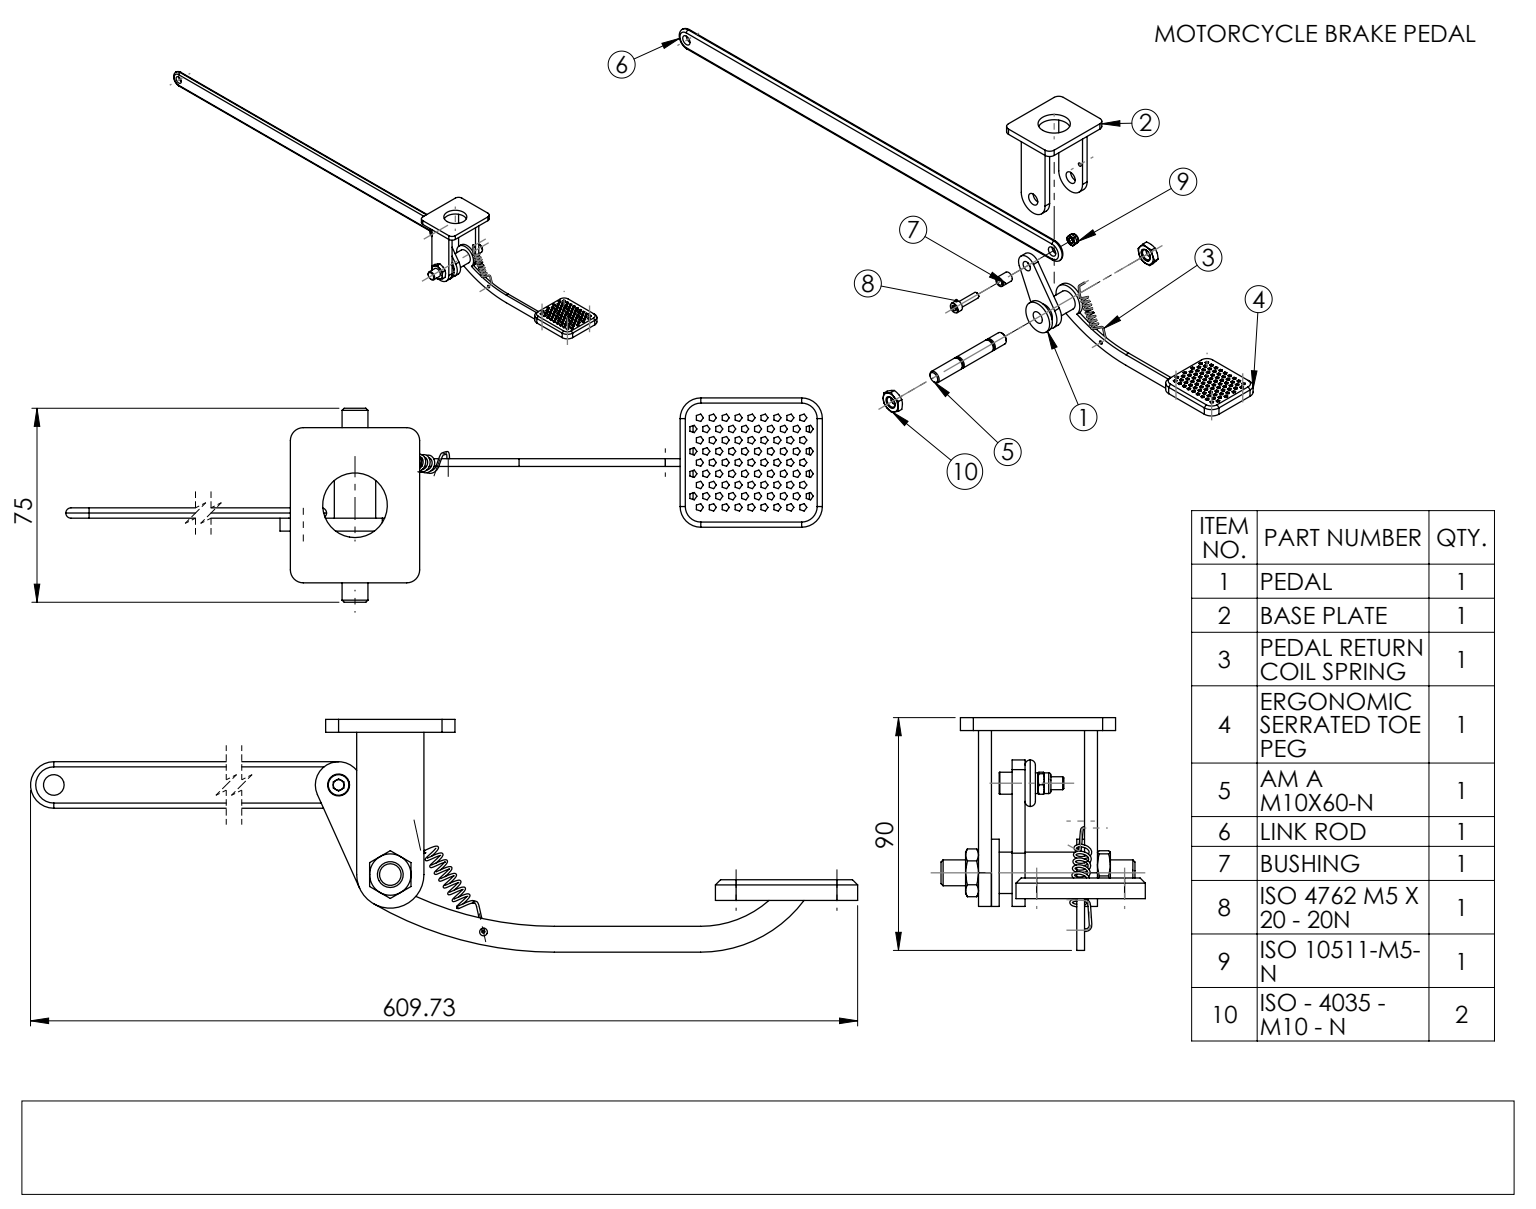
ISO-10303-21;
HEADER;
FILE_DESCRIPTION (('STEP AP214'),
    '1' );
FILE_NAME ('BR-593',
    '2026-09-30T16:28:02',
    ( '' ),
    ( '' ),
    'SwSTEP 2.0',
    'SolidWorks 2026',
    '' );
FILE_SCHEMA (( 'AUTOMOTIVE_DESIGN' ));
ENDSEC;

DATA;
#1 = CARTESIAN_POINT ( 'NONE',  ( 171.1922820468852819, -9.999999999999996447, -4.936203717676158398 ) ) ;
#2 = LINE ( 'NONE', #9287, #2166 ) ;
#3 = CARTESIAN_POINT ( 'NONE',  ( 10.46436961932593945, 16.48727764291732711, -17.33901581970886241 ) ) ;
#4 = PLANE ( 'NONE',  #18463 ) ;
#5 = CARTESIAN_POINT ( 'NONE',  ( 33.35202879388211983, -12.33251541790028760, -19.68467382345759376 ) ) ;
#6 = ORIENTED_EDGE ( 'NONE', *, *, #8201, .T. ) ;
#7 = CARTESIAN_POINT ( 'NONE',  ( 11.86544027865023843, 7.919735734555668039, -16.84125344233394372 ) ) ;
#8 = EDGE_LOOP ( 'NONE', ( #13410, #18933, #24855, #7147 ) ) ;
#9 = CARTESIAN_POINT ( 'NONE',  ( 158.6922820468853104, -1.999999999999974909, -0.6060766987539614181 ) ) ;
#10 = CARTESIAN_POINT ( 'NONE',  ( 20.51249478307574847, 1.942573248051725709, -13.31196225760961838 ) ) ;
#11 = CARTESIAN_POINT ( 'NONE',  ( 11.27738072919014911, 16.67146171448561276, -16.78403338633166442 ) ) ;
#12 = CARTESIAN_POINT ( 'NONE',  ( 35.03938282813840743, -19.89690018161999419, -20.20402626681843117 ) ) ;
#13 = AXIS2_PLACEMENT_3D ( 'NONE', #28994, #19329, #14737 ) ;
#14 = VERTEX_POINT ( 'NONE', #15281 ) ;
#15 = CARTESIAN_POINT ( 'NONE',  ( 9.776119957569173735, 17.05082265352876547, -16.72288386497739765 ) ) ;
#16 = CARTESIAN_POINT ( 'NONE',  ( 176.1922820468852535, -9.999999999999994671, -4.936203717676158398 ) ) ;
#17 = AXIS2_PLACEMENT_3D ( 'NONE', #6944, #25711, #22673 ) ;
#18 = CARTESIAN_POINT ( 'NONE',  ( 9.641351338355821810, 17.66888872024471624, -17.91303689663363130 ) ) ;
#19 = CARTESIAN_POINT ( 'NONE',  ( 129.5152310637605524, -10.00000000000000888, -21.71180489736090991 ) ) ;
#20 = LINE ( 'NONE', #28431, #3804 ) ;
#21 = ADVANCED_BREP_SHAPE_REPRESENTATION ( '', ( #979, #13190 ), #8326 ) ;
#22 = ORIENTED_EDGE ( 'NONE', *, *, #9858, .T. ) ;
#23 = DIRECTION ( 'NONE',  ( -0.5877852522924731371, 0.000000000000000000, 0.8090169943749474513 ) ) ;
#24 = EDGE_LOOP ( 'NONE', ( #18208, #203, #15820, #9762, #20509 ) ) ;
#25 = CARTESIAN_POINT ( 'NONE',  ( 10.43477690885096720, 16.62299358534909288, -17.37687480348504820 ) ) ;
#26 = EDGE_CURVE ( 'NONE', #4351, #19336, #2033, .T. ) ;
#27 = EDGE_CURVE ( 'NONE', #25495, #12783, #12701, .T. ) ;
#28 = CARTESIAN_POINT ( 'NONE',  ( 36.54859390953724585, -22.18451583373416014, -17.64281456791166036 ) ) ;
#29 = CARTESIAN_POINT ( 'NONE',  ( 24.62590367393082502, -9.567571807129121808, -15.85044010117769098 ) ) ;
#30 = ORIENTED_EDGE ( 'NONE', *, *, #5505, .F. ) ;
#31 = EDGE_CURVE ( 'NONE', #25811, #28060, #3559, .T. ) ;
#32 = FACE_OUTER_BOUND ( 'NONE', #14723, .T. ) ;
#33 = CARTESIAN_POINT ( 'NONE',  ( 142.0152310637605524, -1.999999999999978684, 1.702185954127501066 ) ) ;
#34 = VECTOR ( 'NONE', #18733, 1000.000000000000000 ) ;
#35 = CARTESIAN_POINT ( 'NONE',  ( 0.000000000000000000, 0.000000000000000000, 0.000000000000000000 ) ) ;
#36 = AXIS2_PLACEMENT_3D ( 'NONE', #24795, #28817, #15305 ) ;
#37 = CARTESIAN_POINT ( 'NONE',  ( 19.85258860919307367, 6.732389232436280402, -16.96582824858274208 ) ) ;
#38 = VECTOR ( 'NONE', #16062, 999.9999999999998863 ) ;
#39 = CARTESIAN_POINT ( 'NONE',  ( 29.40876261992080032, -8.787110225502646088, -16.42709622331022956 ) ) ;
#40 = ORIENTED_EDGE ( 'NONE', *, *, #8836, .F. ) ;
#41 = DIRECTION ( 'NONE',  ( -2.698458740408365879E-16, 1.000000000000000000, 0.000000000000000000 ) ) ;
#42 = STYLED_ITEM ( 'NONE', ( #6036 ), #28104 ) ;
#43 = EDGE_LOOP ( 'NONE', ( #10791, #17120, #27313, #27403, #18272 ) ) ;
#44 = CARTESIAN_POINT ( 'NONE',  ( 10.00000000000007816, 17.32050807568872486, -23.00000000000000711 ) ) ;
#45 = DIRECTION ( 'NONE',  ( 2.908569913943825554E-16, -1.000000000000000000, 0.000000000000000000 ) ) ;
#46 = ORIENTED_EDGE ( 'NONE', *, *, #12896, .F. ) ;
#47 = CARTESIAN_POINT ( 'NONE',  ( 149.7287565553229456, -10.00000000000000355, 0.8205080756887930260 ) ) ;
#48 = CARTESIAN_POINT ( 'NONE',  ( 10.33812866905494587, 18.38613571942487113, -17.90056368370468931 ) ) ;
#49 = LINE ( 'NONE', #2798, #15810 ) ;
#50 = EDGE_LOOP ( 'NONE', ( #6565, #21196, #16941, #11430, #26912 ) ) ;
#51 = CARTESIAN_POINT ( 'NONE',  ( 4.000000000000019540, 6.928203230275512325, 0.000000000000000000 ) ) ;
#52 = EDGE_LOOP ( 'NONE', ( #7879, #12886, #2199, #3337, #17093, #20123 ) ) ;
#53 = AXIS2_PLACEMENT_3D ( 'NONE', #5832, #6438, #24451 ) ;
#54 = CARTESIAN_POINT ( 'NONE',  ( 9.917712295358372288, 16.40146214360271770, -16.50402730409559027 ) ) ;
#55 = ORIENTED_EDGE ( 'NONE', *, *, #7367, .F. ) ;
#56 = CARTESIAN_POINT ( 'NONE',  ( 28.55476651072185845, -11.97999099613336504, -13.94805024529803994 ) ) ;
#57 = CARTESIAN_POINT ( 'NONE',  ( 142.2287565553230309, -10.00000000000000533, -29.49038105676660138 ) ) ;
#58 = CARTESIAN_POINT ( 'NONE',  ( 25.71553203045151292, -8.406338935355361031, -18.42709291467145150 ) ) ;
#59 = ORIENTED_EDGE ( 'NONE', *, *, #1895, .T. ) ;
#60 = LINE ( 'NONE', #7229, #30116 ) ;
#61 = CARTESIAN_POINT ( 'NONE',  ( 11.05541548581436118, 17.68942261459453036, -17.91440211708152574 ) ) ;
#62 = EDGE_CURVE ( 'NONE', #29710, #22500, #27244, .T. ) ;
#63 = CARTESIAN_POINT ( 'NONE',  ( 32.97927115036063839, -11.75136040154610662, -17.31233706439427067 ) ) ;
#64 = CARTESIAN_POINT ( 'NONE',  ( 14.34656430690936624, 9.113120221615268690, -15.03016663717492563 ) ) ;
#65 = ADVANCED_FACE ( 'NONE', ( #1579 ), #24770, .T. ) ;
#66 = CARTESIAN_POINT ( 'NONE',  ( 16.00000000000017053, 34.64101615137744972, 14.00000000000000178 ) ) ;
#67 = ADVANCED_FACE ( 'NONE', ( #10563 ), #23345, .T. ) ;
#68 = CARTESIAN_POINT ( 'NONE',  ( 23.37849240255853189, -5.075553540114302820, -18.86401745356084447 ) ) ;
#69 = EDGE_LOOP ( 'NONE', ( #19720, #1724, #9767, #14173 ) ) ;
#70 = PLANE ( 'NONE',  #26676 ) ;
#71 = ORIENTED_EDGE ( 'NONE', *, *, #5370, .F. ) ;
#72 =( NAMED_UNIT ( * ) PLANE_ANGLE_UNIT ( ) SI_UNIT ( $, .RADIAN. ) );
#73 = CARTESIAN_POINT ( 'NONE',  ( 16.00562779705659011, 2.776126820729137190, -17.20623408552720690 ) ) ;
#74 = CARTESIAN_POINT ( 'NONE',  ( 16.42253358145367415, 4.166353156564198024, -16.06924993952044289 ) ) ;
#75 = ORIENTED_EDGE ( 'NONE', *, *, #15408, .T. ) ;
#76 = VECTOR ( 'NONE', #4215, 1000.000000000000000 ) ;
#77 = CARTESIAN_POINT ( 'NONE',  ( 133.7287565553229456, -4.999999999999982236, 3.500000000000003109 ) ) ;
#78 = VECTOR ( 'NONE', #21293, 999.9999999999998863 ) ;
#79 = LINE ( 'NONE', #18686, #13812 ) ;
#80 = DIRECTION ( 'NONE',  ( 0.9510565162951536422, 0.000000000000000000, -0.3090169943749475623 ) ) ;
#81 = CARTESIAN_POINT ( 'NONE',  ( 164.5152310637605240, -9.999999999999996447, -28.60870317832789667 ) ) ;
#82 = DIRECTION ( 'NONE',  ( -1.110223024625156540E-16, 0.000000000000000000, -1.000000000000000000 ) ) ;
#83 = CARTESIAN_POINT ( 'NONE',  ( 9.641350810849047548, 17.66889113945805789, -17.91928203681695564 ) ) ;
#84 = CARTESIAN_POINT ( 'NONE',  ( 20.82548126942529976, -5.669333895406754031, -14.77195412306030420 ) ) ;
#85 = CARTESIAN_POINT ( 'NONE',  ( 23.74924978780510898, -3.048960050427876656, -13.27477993493952191 ) ) ;
#86 = EDGE_CURVE ( 'NONE', #12166, #722, #15592, .T. ) ;
#87 = CARTESIAN_POINT ( 'NONE',  ( 36.54859390953724585, -23.18451583373416014, -18.06010107863414405 ) ) ;
#88 = DIRECTION ( 'NONE',  ( 1.000000000000000000, 0.000000000000000000, 0.000000000000000000 ) ) ;
#89 = DIRECTION ( 'NONE',  ( -1.000000000000000000, 2.207829878515935943E-16, 0.000000000000000000 ) ) ;
#90 = PLANE ( 'NONE',  #29362 ) ;
#91 = DIRECTION ( 'NONE',  ( -2.698458740408365879E-16, 1.000000000000000000, 0.000000000000000000 ) ) ;
#92 = DIRECTION ( 'NONE',  ( -0.9510565162951536422, 0.000000000000000000, -0.3090169943749472292 ) ) ;
#93 = ORIENTED_EDGE ( 'NONE', *, *, #14811, .T. ) ;
#94 = CARTESIAN_POINT ( 'NONE',  ( -13.00000000000001243, 55.00000000000000711, 18.00000000000000000 ) ) ;
#95 = CARTESIAN_POINT ( 'NONE',  ( 10.33811987107833552, 18.38617606806709048, -17.90816805339326834 ) ) ;
#96 = ORIENTED_EDGE ( 'NONE', *, *, #21204, .F. ) ;
#97 = CARTESIAN_POINT ( 'NONE',  ( 164.5152310637604671, -9.999999999999998224, -11.28819510263909542 ) ) ;
#98 = CARTESIAN_POINT ( 'NONE',  ( 152.0152310637604671, -4.999999999999976907, -0.06116980274991495881 ) ) ;
#99 = ADVANCED_FACE ( 'NONE', ( #8123 ), #7974, .T. ) ;
#100 = CARTESIAN_POINT ( 'NONE',  ( 14.18486973814142793, 6.324582201221724098, -17.68508340245422872 ) ) ;
#101 = EDGE_CURVE ( 'NONE', #2266, #29239, #23530, .T. ) ;
#102 = VERTEX_POINT ( 'NONE', #17428 ) ;
#103 = EDGE_CURVE ( 'NONE', #184, #26603, #5846, .T. ) ;
#104 = CARTESIAN_POINT ( 'NONE',  ( 25.08912532741139501, -12.86307741315042108, -14.91192194027685147 ) ) ;
#105 = EDGE_LOOP ( 'NONE', ( #1685, #5636, #6833, #29745, #13110 ) ) ;
#106 = EDGE_CURVE ( 'NONE', #19956, #14105, #21866, .T. ) ;
#107 = CARTESIAN_POINT ( 'NONE',  ( 34.90271572771163733, -20.28292729397994876, -21.20502438346732887 ) ) ;
#108 = CARTESIAN_POINT ( 'NONE',  ( 24.18628427323349328, -0.8779346998738073449, -17.06787597161793357 ) ) ;
#109 = CARTESIAN_POINT ( 'NONE',  ( 18.93384218461971358, 6.651393094135895190, -15.21227712214292538 ) ) ;
#110 = ORIENTED_EDGE ( 'NONE', *, *, #8360, .T. ) ;
#111 = CARTESIAN_POINT ( 'NONE',  ( 28.58746438791548528, -7.443717211345676432, -18.79719194573140584 ) ) ;
#112 = AXIS2_PLACEMENT_3D ( 'NONE', #25183, #25333, #20434 ) ;
#113 = EDGE_LOOP ( 'NONE', ( #1842, #6412, #14178, #16562 ) ) ;
#114 = CARTESIAN_POINT ( 'NONE',  ( 141.1922820468854525, -10.00000000000000533, -30.91696583120935671 ) ) ;
#116 = ORIENTED_EDGE ( 'NONE', *, *, #15748, .F. ) ;
#115 = CARTESIAN_POINT ( 'NONE',  ( 171.1922820468853388, -4.999999999999971578, -19.40354224447947828 ) ) ;
#117 = VERTEX_POINT ( 'NONE', #8423 ) ;
#118 = CARTESIAN_POINT ( 'NONE',  ( 134.5152310637605524, -1.999999999999980460, -4.391296821672111328 ) ) ;
#119 = FACE_OUTER_BOUND ( 'NONE', #9403, .T. ) ;
#120 = CARTESIAN_POINT ( 'NONE',  ( 33.16581763841239194, -10.35476010881584052, -17.60936685258081624 ) ) ;
#121 = CARTESIAN_POINT ( 'NONE',  ( 9.641890818133653340, 17.66641459721583374, -17.82828029666912073 ) ) ;
#122 = ORIENTED_EDGE ( 'NONE', *, *, #28451, .T. ) ;
#123 = AXIS2_PLACEMENT_3D ( 'NONE', #1550, #9129, #25482 ) ;
#124 = DIRECTION ( 'NONE',  ( 0.9510565162951536422, 0.000000000000000000, -0.3090169943749475623 ) ) ;
#125 = CARTESIAN_POINT ( 'NONE',  ( 158.6922820468854241, -1.999999999999973133, -35.24709285013155835 ) ) ;
#126 = CARTESIAN_POINT ( 'NONE',  ( 10.46960557229346733, 16.46326489517938541, -17.33590790293451178 ) ) ;
#127 = CYLINDRICAL_SURFACE ( 'NONE', #6337, 13.00000000000000178 ) ;
#128 = CARTESIAN_POINT ( 'NONE',  ( 174.5152310637604955, -1.999999999999968914, -28.60870317832789667 ) ) ;
#129 = ORIENTED_EDGE ( 'NONE', *, *, #17959, .T. ) ;
#130 = DIRECTION ( 'NONE',  ( -0.5877852522924731371, -1.586114251531760728E-16, -0.8090169943749474513 ) ) ;
#131 = EDGE_CURVE ( 'NONE', #19668, #13066, #17725, .T. ) ;
#132 = LINE ( 'NONE', #2726, #539 ) ;
#134 = VERTEX_POINT ( 'NONE', #3860 ) ;
#133 = VECTOR ( 'NONE', #22097, 1000.000000000000000 ) ;
#135 = ADVANCED_FACE ( 'NONE', ( #10257 ), #20396, .T. ) ;
#136 = LINE ( 'NONE', #8159, #30161 ) ;
#137 = ORIENTED_EDGE ( 'NONE', *, *, #26787, .F. ) ;
#138 = EDGE_CURVE ( 'NONE', #19707, #18049, #20216, .T. ) ;
#139 = CARTESIAN_POINT ( 'NONE',  ( 11.09431937732777129, 9.685491096586417825, -17.29518830297554643 ) ) ;
#140 = CARTESIAN_POINT ( 'NONE',  ( 25.86320101420157158, -8.291784280105535032, -12.84902276017926859 ) ) ;
#141 = CARTESIAN_POINT ( 'NONE',  ( 19.89307947303188229, -2.966738011908462092, -16.73278295482091949 ) ) ;
#142 = ORIENTED_EDGE ( 'NONE', *, *, #977, .F. ) ;
#143 = CARTESIAN_POINT ( 'NONE',  ( 18.39996379557756256, 0.6904185378075045065, -15.43317298867526866 ) ) ;
#144 = FACE_OUTER_BOUND ( 'NONE', #11125, .T. ) ;
#145 = CARTESIAN_POINT ( 'NONE',  ( -2.644994884459112683, 7.710515798486374806, -0.08224679563972035756 ) ) ;
#146 = DIRECTION ( 'NONE',  ( 0.5877852522924731371, 1.586114251531760728E-16, 0.8090169943749474513 ) ) ;
#147 = CARTESIAN_POINT ( 'NONE',  ( 27.44219139316946965, -6.774709612358828181, -18.29578255718776703 ) ) ;
#148 = AXIS2_PLACEMENT_3D ( 'NONE', #18004, #8395, #8543 ) ;
#149 = CARTESIAN_POINT ( 'NONE',  ( 2.681483223904240987, -3.070647092368469000, -1.935399088488818784E-14 ) ) ;
#150 = DIRECTION ( 'NONE',  ( 0.000000000000000000, -0.000000000000000000, -1.000000000000000000 ) ) ;
#151 = PRESENTATION_STYLE_ASSIGNMENT (( #9284 ) ) ;
#152 = LINE ( 'NONE', #16311, #22917 ) ;
#153 = CARTESIAN_POINT ( 'NONE',  ( 2.681483223904239210, -3.070647092368469888, -2.449999999999981526 ) ) ;
#154 = VECTOR ( 'NONE', #27172, 1000.000000000000000 ) ;
#155 = EDGE_CURVE ( 'NONE', #6429, #19044, #27953, .T. ) ;
#156 = CARTESIAN_POINT ( 'NONE',  ( 10.35864918915110877, 16.97212501191939538, -17.92279151347709032 ) ) ;
#157 = CARTESIAN_POINT ( 'NONE',  ( 35.24964364652129234, -20.84149066036063047, -20.16262864730545346 ) ) ;
#158 = CARTESIAN_POINT ( 'NONE',  ( 31.39893620166130717, -10.86152586746012183, -14.84747879817187943 ) ) ;
#159 = EDGE_LOOP ( 'NONE', ( #26416, #20903, #28794, #24499, #27382, #1252 ) ) ;
#160 = CARTESIAN_POINT ( 'NONE',  ( 8.944584812045984989, 16.95159217075808655, -17.91472939532503261 ) ) ;
#161 = ORIENTED_EDGE ( 'NONE', *, *, #1761, .F. ) ;
#162 = LINE ( 'NONE', #17082, #29052 ) ;
#163 = CARTESIAN_POINT ( 'NONE',  ( 19.38992137333195842, 2.881095379261479739, -20.30776781288435373 ) ) ;
#164 = CARTESIAN_POINT ( 'NONE',  ( 11.27814055543051630, 16.66797705449195988, -16.78371917145281955 ) ) ;
#165 = CARTESIAN_POINT ( 'NONE',  ( 21.73040598723229877, -5.000000000000011546, -66.87931276303945083 ) ) ;
#166 = EDGE_LOOP ( 'NONE', ( #11300, #21186, #18431, #15934 ) ) ;
#167 = VECTOR ( 'NONE', #27934, 1000.000000000000000 ) ;
#168 = ORIENTED_EDGE ( 'NONE', *, *, #18099, .T. ) ;
#169 = CARTESIAN_POINT ( 'NONE',  ( 9.916551108984865692, 16.40678749232849398, -16.50450761325770443 ) ) ;
#170 = CARTESIAN_POINT ( 'NONE',  ( 125.7287565553229172, -4.000000000000003553, -33.50000000000000000 ) ) ;
#171 = CARTESIAN_POINT ( 'NONE',  ( 9.843778300897430000, 16.74053286659246709, -16.57516421589427225 ) ) ;
#172 = DIRECTION ( 'NONE',  ( -0.9510565162951536422, -2.566386769018988323E-16, 0.3090169943749475623 ) ) ;
#173 = CARTESIAN_POINT ( 'NONE',  ( 136.1922820468854241, -1.999999999999980460, -19.40354224447947473 ) ) ;
#174 = ORIENTED_EDGE ( 'NONE', *, *, #103, .T. ) ;
#175 = EDGE_CURVE ( 'NONE', #8969, #15955, #19420, .T. ) ;
#176 = CARTESIAN_POINT ( 'NONE',  ( 168.6922820468853104, -9.999999999999998224, -6.413161187712876909 ) ) ;
#177 = ORIENTED_EDGE ( 'NONE', *, *, #22974, .T. ) ;
#178 = EDGE_CURVE ( 'NONE', #21232, #6302, #23638, .T. ) ;
#179 = CARTESIAN_POINT ( 'NONE',  ( 10.35887147716723611, 16.97110557074245563, -17.87975733919941845 ) ) ;
#180 = ORIENTED_EDGE ( 'NONE', *, *, #14435, .F. ) ;
#181 = CARTESIAN_POINT ( 'NONE',  ( 36.04209255463945993, -19.90907354740926394, -20.43687144983462289 ) ) ;
#182 = CARTESIAN_POINT ( 'NONE',  ( 21.18945582756405344, -5.194394521544061227, -16.21196392551894405 ) ) ;
#183 = CARTESIAN_POINT ( 'NONE',  ( 27.21278356834291756, -7.014839303453253905, -18.45691071023835761 ) ) ;
#184 = VERTEX_POINT ( 'NONE', #293 ) ;
#185 = LINE ( 'NONE', #484, #11097 ) ;
#186 = CIRCLE ( 'NONE', #15750, 0.4999999999999998335 ) ;
#187 = DIRECTION ( 'NONE',  ( -0.5877852522924731371, -1.586114251531760728E-16, -0.8090169943749474513 ) ) ;
#188 = DIRECTION ( 'NONE',  ( 1.000000000000000000, 0.000000000000000000, 0.000000000000000000 ) ) ;
#189 = CARTESIAN_POINT ( 'NONE',  ( 19.09420370221858931, 5.586061004495046056, -18.95245686415860220 ) ) ;
#190 = CARTESIAN_POINT ( 'NONE',  ( 26.02011856185544048, -9.832954462109395166, -14.66174570188732140 ) ) ;
#191 = ORIENTED_EDGE ( 'NONE', *, *, #12444, .F. ) ;
#192 = FACE_BOUND ( 'NONE', #6466, .T. ) ;
#193 = ORIENTED_EDGE ( 'NONE', *, *, #2861, .F. ) ;
#194 = EDGE_CURVE ( 'NONE', #21176, #29420, #19051, .T. ) ;
#195 = ADVANCED_FACE ( 'NONE', ( #2293 ), #12020, .T. ) ;
#196 = FACE_OUTER_BOUND ( 'NONE', #7916, .T. ) ;
#197 = DIRECTION ( 'NONE',  ( -0.5877852522924731371, -1.586114251531760728E-16, -0.8090169943749474513 ) ) ;
#198 = LINE ( 'NONE', #11177, #23639 ) ;
#199 = VECTOR ( 'NONE', #16621, 1000.000000000000000 ) ;
#200 = CARTESIAN_POINT ( 'NONE',  ( 10.73095126193553028, 16.58460123524055874, -15.94999808000346242 ) ) ;
#201 = CARTESIAN_POINT ( 'NONE',  ( 11.95300070842526274, -5.000000000000014211, 36.78755350016455594 ) ) ;
#202 = CARTESIAN_POINT ( 'NONE',  ( 1.313474075707222521, 8.479269695850875976, -0.3167204509598505746 ) ) ;
#203 = ORIENTED_EDGE ( 'NONE', *, *, #27651, .T. ) ;
#204 = CARTESIAN_POINT ( 'NONE',  ( 9.916551108984865692, 16.40678749232849398, -16.50450761325770443 ) ) ;
#205 = ORIENTED_EDGE ( 'NONE', *, *, #21724, .F. ) ;
#206 = CARTESIAN_POINT ( 'NONE',  ( 18.72855672543857608, 2.184447897796080174, -13.82944682127929426 ) ) ;
#207 = DIRECTION ( 'NONE',  ( -0.9510565162951536422, -2.566386769018988323E-16, 0.3090169943749475623 ) ) ;
#208 = CARTESIAN_POINT ( 'NONE',  ( 161.1922820468853388, -9.999999999999998224, -13.59645775552055902 ) ) ;
#209 = VERTEX_POINT ( 'NONE', #7460 ) ;
#210 = CARTESIAN_POINT ( 'NONE',  ( 25.79824969357368047, -12.24460132778619226, -15.92960863319586906 ) ) ;
#211 = ORIENTED_EDGE ( 'NONE', *, *, #18755, .T. ) ;
#212 = FACE_OUTER_BOUND ( 'NONE', #25235, .T. ) ;
#213 = CARTESIAN_POINT ( 'NONE',  ( 11.05541700792677062, 17.68941563399299710, -17.91138715956864047 ) ) ;
#214 = ORIENTED_EDGE ( 'NONE', *, *, #14160, .F. ) ;
#215 = CARTESIAN_POINT ( 'NONE',  ( 33.76744293605320024, -13.18274801178271005, -18.77722780292321758 ) ) ;
#216 = CARTESIAN_POINT ( 'NONE',  ( 172.7287565553229456, -1.999999999999974021, -33.50000000000000000 ) ) ;
#217 = ORIENTED_EDGE ( 'NONE', *, *, #1804, .F. ) ;
#218 = CARTESIAN_POINT ( 'NONE',  ( 164.5152310637604671, -4.999999999999973355, -1.826485974285146553E-14 ) ) ;
#219 = CARTESIAN_POINT ( 'NONE',  ( 23.38597214775318278, -9.778565425610747042, -17.35394146810280347 ) ) ;
#220 = VERTEX_POINT ( 'NONE', #14001 ) ;
#221 = DIRECTION ( 'NONE',  ( 0.9510565162951536422, 0.000000000000000000, -0.3090169943749475623 ) ) ;
#222 = ORIENTED_EDGE ( 'NONE', *, *, #14772, .T. ) ;
#223 = CARTESIAN_POINT ( 'NONE',  ( 21.13650371987585075, 4.769999862021419901, -15.38713752973847448 ) ) ;
#224 = CARTESIAN_POINT ( 'NONE',  ( 17.80416238081608071, 8.561068417093343541, -18.87148919878627140 ) ) ;
#225 = VECTOR ( 'NONE', #26675, 1000.000000000000000 ) ;
#226 = ORIENTED_EDGE ( 'NONE', *, *, #24841, .F. ) ;
#227 = ORIENTED_EDGE ( 'NONE', *, *, #21857, .F. ) ;
#228 = CARTESIAN_POINT ( 'NONE',  ( 163.6922820468852819, -9.999999999999998224, -0.6060766987539614181 ) ) ;
#229 = CARTESIAN_POINT ( 'NONE',  ( 151.1922820468853672, -1.999999999999976685, -2.083034168790677043 ) ) ;
#230 = EDGE_CURVE ( 'NONE', #17843, #12321, #21337, .T. ) ;
#231 = EDGE_CURVE ( 'NONE', #23545, #23604, #24924, .T. ) ;
#232 = DIRECTION ( 'NONE',  ( -2.698458740408365879E-16, 1.000000000000000000, 0.000000000000000000 ) ) ;
#233 = DIRECTION ( 'NONE',  ( -2.698458740408365879E-16, 1.000000000000000000, 0.000000000000000000 ) ) ;
#234 = EDGE_CURVE ( 'NONE', #25907, #1746, #23486, .T. ) ;
#235 = DIRECTION ( 'NONE',  ( 0.3090169943749475623, 8.338696094058001131E-17, 0.9510565162951536422 ) ) ;
#236 = EDGE_LOOP ( 'NONE', ( #22910, #13879, #24086, #12025 ) ) ;
#237 = ADVANCED_FACE ( 'NONE', ( #2593 ), #18453, .T. ) ;
#238 = CARTESIAN_POINT ( 'NONE',  ( 9.921764701973689426, 16.38287729030320250, -16.50235149140834778 ) ) ;
#239 = CARTESIAN_POINT ( 'NONE',  ( 23.58034929565730309, -2.629172400889816075, -20.70693660786654888 ) ) ;
#240 = CARTESIAN_POINT ( 'NONE',  ( 19.50876870223950377, -1.661710298099399630, -15.95382585723518432 ) ) ;
#242 = ORIENTED_EDGE ( 'NONE', *, *, #15818, .F. ) ;
#241 = CARTESIAN_POINT ( 'NONE',  ( 32.24963562184495203, -10.43994945000269148, -19.19593526939238970 ) ) ;
#243 =( NAMED_UNIT ( * ) PLANE_ANGLE_UNIT ( ) SI_UNIT ( $, .RADIAN. ) );
#244 = DIRECTION ( 'NONE',  ( 0.3090169943749475623, 8.338696094058001131E-17, 0.9510565162951536422 ) ) ;
#245 = VECTOR ( 'NONE', #20484, 999.9999999999998863 ) ;
#246 = CARTESIAN_POINT ( 'NONE',  ( 157.0152310637605808, -4.999999999999975131, -32.93883019725009120 ) ) ;
#247 = DIRECTION ( 'NONE',  ( -0.9510565162951536422, -2.566386769018988816E-16, -0.3090169943749472292 ) ) ;
#248 = CARTESIAN_POINT ( 'NONE',  ( 14.39533340154967433, 6.572929804808670617, -18.54476805420031837 ) ) ;
#249 = ORIENTED_EDGE ( 'NONE', *, *, #10382, .F. ) ;
#250 = CARTESIAN_POINT ( 'NONE',  ( 169.5152310637604955, -1.999999999999970024, -30.37205893520531319 ) ) ;
#251 = CARTESIAN_POINT ( 'NONE',  ( 10.68867725192709273, 16.77847523382220984, -15.97313786900300059 ) ) ;
#252 = EDGE_LOOP ( 'NONE', ( #8891, #22753, #23266, #17300 ) ) ;
#253 = LINE ( 'NONE', #12283, #20751 ) ;
#254 = LINE ( 'NONE', #28368, #19057 ) ;
#255 = CARTESIAN_POINT ( 'NONE',  ( 19.20291185354690811, 8.143073066566493878, -16.32372945079811188 ) ) ;
#256 = CARTESIAN_POINT ( 'NONE',  ( 16.48605814428184857, 11.34583003460130435, -14.75612992736757256 ) ) ;
#257 = ORIENTED_EDGE ( 'NONE', *, *, #15684, .T. ) ;
#258 = CARTESIAN_POINT ( 'NONE',  ( 35.54859390953724585, -23.18451583373416014, -16.11276402859391510 ) ) ;
#259 = CARTESIAN_POINT ( 'NONE',  ( 20.30498772102510685, -2.023023832184298154, -16.94527736422809028 ) ) ;
#260 = CARTESIAN_POINT ( 'NONE',  ( 18.10666546173949953, 1.615696121519054618, -15.79491705146812563 ) ) ;
#261 = ORIENTED_EDGE ( 'NONE', *, *, #3073, .F. ) ;
#262 = CARTESIAN_POINT ( 'NONE',  ( 25.27233071153842303, -10.58027458246514207, -17.53878701932553952 ) ) ;
#263 = ORIENTED_EDGE ( 'NONE', *, *, #16267, .F. ) ;
#264 = AXIS2_PLACEMENT_3D ( 'NONE', #8989, #18309, #27664 ) ;
#265 = ORIENTED_EDGE ( 'NONE', *, *, #4022, .T. ) ;
#266 = DIRECTION ( 'NONE',  ( 0.9510565162951536422, 0.000000000000000000, -0.3090169943749475623 ) ) ;
#267 = PLANE ( 'NONE',  #1442 ) ;
#268 = ADVANCED_FACE ( 'NONE', ( #28096 ), #13304, .T. ) ;
#269 = PLANE ( 'NONE',  #1205 ) ;
#270 = EDGE_CURVE ( 'NONE', #13418, #14798, #2444, .T. ) ;
#271 = DIRECTION ( 'NONE',  ( -2.698458740408365879E-16, 1.000000000000000000, 0.000000000000000000 ) ) ;
#272 = CARTESIAN_POINT ( 'NONE',  ( 36.32827445255054499, -20.19473721995742821, -19.46526261299151983 ) ) ;
#273 = CARTESIAN_POINT ( 'NONE',  ( 15.87304960759194650, 9.003283391651189405, -12.44179493704351280 ) ) ;
#274 = ORIENTED_EDGE ( 'NONE', *, *, #12172, .T. ) ;
#275 = LINE ( 'NONE', #12157, #28348 ) ;
#276 = DIRECTION ( 'NONE',  ( 0.9510565162951536422, 0.000000000000000000, -0.3090169943749475623 ) ) ;
#277 = CARTESIAN_POINT ( 'NONE',  ( 10.55304143273637330, 16.08061740358965253, -17.30129946959702281 ) ) ;
#278 = DIRECTION ( 'NONE',  ( -2.698458740408365879E-16, 1.000000000000000000, 0.000000000000000000 ) ) ;
#279 = DIRECTION ( 'NONE',  ( -0.5877852522924731371, -1.586114251531760728E-16, -0.8090169943749474513 ) ) ;
#280 = VERTEX_POINT ( 'NONE', #21039 ) ;
#281 = VECTOR ( 'NONE', #14887, 1000.000000000000000 ) ;
#282 = DIRECTION ( 'NONE',  ( -0.8090169943749474513, -2.183098979609982436E-16, 0.5877852522924731371 ) ) ;
#283 = CONICAL_SURFACE ( 'NONE', #26615, 4.513000000000000789, 0.2131563744996339549 ) ;
#284 = LINE ( 'NONE', #14293, #25869 ) ;
#285 = ORIENTED_EDGE ( 'NONE', *, *, #11613, .T. ) ;
#286 = ORIENTED_EDGE ( 'NONE', *, *, #25521, .T. ) ;
#287 = DIRECTION ( 'NONE',  ( 0.9510565162951536422, 2.566386769018988816E-16, 0.3090169943749472292 ) ) ;
#288 = VERTEX_POINT ( 'NONE', #4857 ) ;
#289 = CARTESIAN_POINT ( 'NONE',  ( 9.667856465286563505, 16.22743184293591057, -17.88508098240584587 ) ) ;
#290 = CARTESIAN_POINT ( 'NONE',  ( 26.82298874931487020, -4.830090842487210878, -14.67398021261910301 ) ) ;
#291 = CARTESIAN_POINT ( 'NONE',  ( 23.41849298471255381, -3.203224238779429633, -13.27670244232306018 ) ) ;
#292 = DIRECTION ( 'NONE',  ( -0.5877852522924731371, -1.586114251531760235E-16, 0.8090169943749474513 ) ) ;
#293 = CARTESIAN_POINT ( 'NONE',  ( 5.000000000000004441, 0.000000000000000000, 4.250000000000000000 ) ) ;
#294 = CARTESIAN_POINT ( 'NONE',  ( 176.1922820468852535, -1.999999999999970024, -4.936203717676158398 ) ) ;
#295 = EDGE_CURVE ( 'NONE', #18615, #29151, #11869, .T. ) ;
#296 = CARTESIAN_POINT ( 'NONE',  ( 25.26806593431409453, -8.821542497490490575, -18.05414547114721557 ) ) ;
#297 = VECTOR ( 'NONE', #130, 1000.000000000000000 ) ;
#298 = ORIENTED_EDGE ( 'NONE', *, *, #1039, .F. ) ;
#299 = DIRECTION ( 'NONE',  ( -0.9510565162951536422, -2.566386769018988323E-16, 0.3090169943749475623 ) ) ;
#300 = LINE ( 'NONE', #23185, #15709 ) ;
#301 = VECTOR ( 'NONE', #6965, 1000.000000000000000 ) ;
#302 = ADVANCED_FACE ( 'NONE', ( #28256 ), #7306, .T. ) ;
#303 = EDGE_CURVE ( 'NONE', #13765, #18617, #4330, .T. ) ;
#304 = CARTESIAN_POINT ( 'NONE',  ( 0.000000000000000000, 0.000000000000000000, -0.5251556536572770106 ) ) ;
#306 = CARTESIAN_POINT ( 'NONE',  ( 169.7287565553228887, -9.999999999999998224, -7.839745962155603820 ) ) ;
#305 = AXIS2_PLACEMENT_3D ( 'NONE', #1101, #17395, #12671 ) ;
#307 = EDGE_CURVE ( 'NONE', #30043, #633, #23795, .T. ) ;
#308 = EDGE_CURVE ( 'NONE', #11681, #9083, #21945, .T. ) ;
#309 = CARTESIAN_POINT ( 'NONE',  ( 10.47103768343372288, 16.45669705093847313, -17.33522727542475295 ) ) ;
#310 = CARTESIAN_POINT ( 'NONE',  ( 20.00000000000017053, 34.64101615137744972, 14.00000000000000178 ) ) ;
#311 = LINE ( 'NONE', #12188, #27806 ) ;
#312 = ORIENTED_EDGE ( 'NONE', *, *, #15522, .T. ) ;
#313 = CARTESIAN_POINT ( 'NONE',  ( 13.40647825129878612, 7.637826363492710158, -15.68645975549014082 ) ) ;
#314 = VERTEX_POINT ( 'NONE', #24094 ) ;
#315 = DIRECTION ( 'NONE',  ( -0.5877852522924731371, -1.586114251531760728E-16, -0.8090169943749474513 ) ) ;
#316 = CARTESIAN_POINT ( 'NONE',  ( 23.66272512268759343, 2.894330346666426745, -16.12005855839824520 ) ) ;
#317 = CARTESIAN_POINT ( 'NONE',  ( 11.27662090294977837, 16.67494637447927275, -16.78434760121053060 ) ) ;
#318 = FACE_BOUND ( 'NONE', #13580, .T. ) ;
#319 = VERTEX_POINT ( 'NONE', #1201 ) ;
#320 = ORIENTED_EDGE ( 'NONE', *, *, #6013, .F. ) ;
#321 = CARTESIAN_POINT ( 'NONE',  ( 9.641350835837977584, 17.66889102485563612, -17.91507476468484938 ) ) ;
#322 = CARTESIAN_POINT ( 'NONE',  ( 174.7287565553229172, -9.999999999999994671, -25.16025403784440329 ) ) ;
#323 = VECTOR ( 'NONE', #10436, 1000.000000000000000 ) ;
#324 = CARTESIAN_POINT ( 'NONE',  ( 9.916953853453376766, 16.40494045485788632, -16.50434094533541085 ) ) ;
#325 = DIRECTION ( 'NONE',  ( -0.5877852522924731371, -1.586114251531760235E-16, 0.8090169943749474513 ) ) ;
#326 = PLANE ( 'NONE',  #24744 ) ;
#327 = ORIENTED_EDGE ( 'NONE', *, *, #10733, .F. ) ;
#328 = CARTESIAN_POINT ( 'NONE',  ( 4.680456609903983711, 6.535341423375600201, -4.983111142572226981 ) ) ;
#329 = ORIENTED_EDGE ( 'NONE', *, *, #5122, .F. ) ;
#330 = CARTESIAN_POINT ( 'NONE',  ( 10.47325967749744180, 16.44650670292386607, -17.33429203187744250 ) ) ;
#331 = ORIENTED_EDGE ( 'NONE', *, *, #10865, .F. ) ;
#333 = CARTESIAN_POINT ( 'NONE',  ( 32.72409873491027099, -9.637868425582460929, -18.36260606011342844 ) ) ;
#332 = VECTOR ( 'NONE', #22511, 1000.000000000000000 ) ;
#334 = CARTESIAN_POINT ( 'NONE',  ( 29.22485947447185595, -8.910266539455653501, -18.36689805200119707 ) ) ;
#335 = CARTESIAN_POINT ( 'NONE',  ( 25.23810427664335165, -6.496417100615061280, -13.69959235629456629 ) ) ;
#336 = VECTOR ( 'NONE', #15406, 1000.000000000000000 ) ;
#337 = DIRECTION ( 'NONE',  ( 0.000000000000000000, 0.000000000000000000, 1.000000000000000000 ) ) ;
#338 = CARTESIAN_POINT ( 'NONE',  ( 34.33515578781254618, -12.24072284059296933, -19.92088757525016973 ) ) ;
#339 = DIRECTION ( 'NONE',  ( 0.000000000000000000, 0.000000000000000000, 1.000000000000000000 ) ) ;
#340 = CARTESIAN_POINT ( 'NONE',  ( 15.71409287621466788, 5.292507472020409942, -15.15310296786427635 ) ) ;
#341 = CARTESIAN_POINT ( 'NONE',  ( 26.65048721414892086, -11.67344998524500355, -15.88597958324129777 ) ) ;
#342 = ORIENTED_EDGE ( 'NONE', *, *, #14480, .T. ) ;
#343 = FACE_BOUND ( 'NONE', #27021, .T. ) ;
#344 = VECTOR ( 'NONE', #10715, 1000.000000000000000 ) ;
#345 = ORIENTED_EDGE ( 'NONE', *, *, #10601, .T. ) ;
#346 = ADVANCED_FACE ( 'NONE', ( #19194 ), #5318, .T. ) ;
#347 = CARTESIAN_POINT ( 'NONE',  ( 0.000000000000000000, 0.000000000000000000, -25.03750572909317285 ) ) ;
#348 = PLANE ( 'NONE',  #22330 ) ;
#349 = LINE ( 'NONE', #4913, #4348 ) ;
#350 = VECTOR ( 'NONE', #1226, 1000.000000000000000 ) ;
#351 = PLANE ( 'NONE',  #28566 ) ;
#352 = AXIS2_PLACEMENT_3D ( 'NONE', #15421, #11403, #30099 ) ;
#353 = CARTESIAN_POINT ( 'NONE',  ( 10.71275814632708823, 16.66803718250374899, -15.95787532639072914 ) ) ;
#354 = CARTESIAN_POINT ( 'NONE',  ( 151.1922820468853672, -4.999999999999976907, -4.936203717676158398 ) ) ;
#355 = AXIS2_PLACEMENT_3D ( 'NONE', #20040, #29561, #1592 ) ;
#356 = FACE_OUTER_BOUND ( 'NONE', #20596, .T. ) ;
#357 = VERTEX_POINT ( 'NONE', #9882 ) ;
#358 = CARTESIAN_POINT ( 'NONE',  ( 9.914377700407460026, 16.41675502110963336, -16.50544604630902867 ) ) ;
#359 = CARTESIAN_POINT ( 'NONE',  ( 9.667469407758799704, 16.22920693809672343, -17.88529630510330293 ) ) ;
#360 = CARTESIAN_POINT ( 'NONE',  ( 17.70496941102466693, 2.403166580496164606, -19.15355645582771871 ) ) ;
#361 = DIRECTION ( 'NONE',  ( 0.000000000000000000, -1.000000000000000000, 0.000000000000000000 ) ) ;
#362 = CARTESIAN_POINT ( 'NONE',  ( 180.7287565553229456, -3.999999999999989786, 0.5000000000000029976 ) ) ;
#363 = CARTESIAN_POINT ( 'NONE',  ( 29.90031526554274777, -7.862644070287768905, -16.42500436498598049 ) ) ;
#364 = LINE ( 'NONE', #23553, #20283 ) ;
#365 = CARTESIAN_POINT ( 'NONE',  ( 11.27712745377669101, 16.67262326781682802, -16.78413812462462573 ) ) ;
#366 = ORIENTED_EDGE ( 'NONE', *, *, #25702, .F. ) ;
#367 = CARTESIAN_POINT ( 'NONE',  ( 35.54859390953724585, -21.18451583373416014, -16.94733705004010105 ) ) ;
#368 = LINE ( 'NONE', #18674, #9316 ) ;
#369 = CARTESIAN_POINT ( 'NONE',  ( 173.6922820468853104, -9.999999999999994671, -17.92658477444275889 ) ) ;
#370 = CARTESIAN_POINT ( 'NONE',  ( 9.112490548836888138, 16.18155505883174783, -17.05474119751274031 ) ) ;
#371 = CARTESIAN_POINT ( 'NONE',  ( 28.50845745928996067, -4.315366227951761502, -16.60164569054668604 ) ) ;
#372 = ORIENTED_EDGE ( 'NONE', *, *, #2420, .F. ) ;
#373 = DIRECTION ( 'NONE',  ( -1.000000000000000000, -0.000000000000000000, -0.000000000000000000 ) ) ;
#374 = EDGE_CURVE ( 'NONE', #25209, #19520, #2893, .T. ) ;
#375 = CARTESIAN_POINT ( 'NONE',  ( 18.32179412900206827, 3.681508181950223335, -14.15692665485406643 ) ) ;
#376 = CIRCLE ( 'NONE', #18872, 3.000000000000002665 ) ;
#377 = CARTESIAN_POINT ( 'NONE',  ( 16.45434084995319424, 8.990804261541395448, -14.78801614696073408 ) ) ;
#378 = ORIENTED_EDGE ( 'NONE', *, *, #6683, .T. ) ;
#379 = VERTEX_POINT ( 'NONE', #12319 ) ;
#380 = CARTESIAN_POINT ( 'NONE',  ( 144.5152310637605240, -4.999999999999978684, -4.391296821672111328 ) ) ;
#381 = CARTESIAN_POINT ( 'NONE',  ( 172.7287565553229456, -3.999999999999989786, -41.50000000000000711 ) ) ;
#382 = CARTESIAN_POINT ( 'NONE',  ( 1.214306433183764966E-14, 4.618802153517016507, -2.092734410091829034 ) ) ;
#383 = DIRECTION ( 'NONE',  ( 1.000000000000000000, 2.891205793294675861E-16, 0.000000000000000000 ) ) ;
#384 = CARTESIAN_POINT ( 'NONE',  ( 174.5152310637604103, -4.999999999999970690, -1.937508276747661576E-14 ) ) ;
#385 = AXIS2_PLACEMENT_3D ( 'NONE', #29992, #3996, #22923 ) ;
#386 = ORIENTED_EDGE ( 'NONE', *, *, #10034, .F. ) ;
#387 = CARTESIAN_POINT ( 'NONE',  ( 9.926830210242822972, 16.35964622367879784, -16.50025672554925293 ) ) ;
#388 = CARTESIAN_POINT ( 'NONE',  ( 29.32553208039167458, -8.962988822949116141, -16.84503999589972523 ) ) ;
#389 = CARTESIAN_POINT ( 'NONE',  ( 19.55718041265476970, -1.390565517676688900, -17.79492730709450754 ) ) ;
#391 = ORIENTED_EDGE ( 'NONE', *, *, #6783, .T. ) ;
#390 = CARTESIAN_POINT ( 'NONE',  ( 36.54859390953724585, -23.18451583373416014, -16.94733705004010105 ) ) ;
#392 = AXIS2_PLACEMENT_3D ( 'NONE', #4305, #4004, #27842 ) ;
#393 = LINE ( 'NONE', #19002, #17550 ) ;
#394 = CARTESIAN_POINT ( 'NONE',  ( 151.1922820468853956, -10.00000000000000178, -10.74328820663507678 ) ) ;
#395 = DIRECTION ( 'NONE',  ( 1.000000000000000000, 0.000000000000000000, -0.000000000000000000 ) ) ;
#396 = CARTESIAN_POINT ( 'NONE',  ( 14.03850921439652311, 8.975161913830900673, -15.18271992443145635 ) ) ;
#397 = EDGE_LOOP ( 'NONE', ( #19913, #23499 ) ) ;
#398 = CARTESIAN_POINT ( 'NONE',  ( 1.734723475976807094E-15, 2.928571428571426161, 2.549999999999999378 ) ) ;
#399 = CARTESIAN_POINT ( 'NONE',  ( 10.35722669462089840, 18.29854973974792998, -17.31575102165233915 ) ) ;
#400 = CARTESIAN_POINT ( 'NONE',  ( -20.00000000000017053, 34.64101615137744972, 0.000000000000000000 ) ) ;
#401 = CARTESIAN_POINT ( 'NONE',  ( 0.000000000000000000, 0.000000000000000000, -5.000000000000000888 ) ) ;
#402 = EDGE_LOOP ( 'NONE', ( #24156, #22408, #9241, #18567 ) ) ;
#403 = CARTESIAN_POINT ( 'NONE',  ( 15.14574614762244487, 6.587483969391940697, -15.14885142785537830 ) ) ;
#404 = EDGE_LOOP ( 'NONE', ( #3779, #2242, #2825, #27348 ) ) ;
#405 = CARTESIAN_POINT ( 'NONE',  ( 12.96291568738609890, 5.695260009123724210, -16.43886026595064109 ) ) ;
#406 = ORIENTED_EDGE ( 'NONE', *, *, #21308, .T. ) ;
#407 = CARTESIAN_POINT ( 'NONE',  ( 32.30218501430429967, -10.99871056796995816, -17.40035725849610060 ) ) ;
#408 = ADVANCED_FACE ( 'NONE', ( #24392 ), #12626, .T. ) ;
#409 = EDGE_CURVE ( 'NONE', #5044, #29035, #5775, .T. ) ;
#410 = CARTESIAN_POINT ( 'NONE',  ( 23.12480016457037379, 1.528454477237789488, -15.53356264363713102 ) ) ;
#411 = EDGE_CURVE ( 'NONE', #18619, #29440, #26701, .T. ) ;
#412 = CARTESIAN_POINT ( 'NONE',  ( 19.55510877418759819, -0.09764134006120470111, -19.21341144728512518 ) ) ;
#413 = VECTOR ( 'NONE', #9450, 1000.000000000000000 ) ;
#414 = CARTESIAN_POINT ( 'NONE',  ( 27.32534031592636836, -8.675155620653059785, -19.25315075663615971 ) ) ;
#415 = VECTOR ( 'NONE', #2292, 1000.000000000000000 ) ;
#416 = ORIENTED_EDGE ( 'NONE', *, *, #15789, .T. ) ;
#417 = DIRECTION ( 'NONE',  ( 0.3090169943749475623, 8.338696094058001131E-17, 0.9510565162951536422 ) ) ;
#419 = EDGE_LOOP ( 'NONE', ( #26721, #25285, #4227, #20986 ) ) ;
#418 = DIRECTION ( 'NONE',  ( -2.698458740408365879E-16, 1.000000000000000000, 0.000000000000000000 ) ) ;
#420 = DIRECTION ( 'NONE',  ( 0.3090169943749475623, 8.338696094058001131E-17, 0.9510565162951536422 ) ) ;
#421 = LINE ( 'NONE', #18729, #12178 ) ;
#422 = CARTESIAN_POINT ( 'NONE',  ( 35.57309713841538468, -16.80212557611773505, -19.25277297559858525 ) ) ;
#423 = CARTESIAN_POINT ( 'NONE',  ( 9.641566850259106758, 17.66790035518494051, -17.86107206016944460 ) ) ;
#424 = ORIENTED_EDGE ( 'NONE', *, *, #5508, .F. ) ;
#425 = CARTESIAN_POINT ( 'NONE',  ( 18.07240892486890615, -5.000000000000012434, -55.62115542516819744 ) ) ;
#426 = CARTESIAN_POINT ( 'NONE',  ( 131.1922820468854241, -1.999999999999981792, -28.06379628232387446 ) ) ;
#427 = CARTESIAN_POINT ( 'NONE',  ( 12.02823749386838514, 9.315180647891255106, -16.69125397286443047 ) ) ;
#428 = DIRECTION ( 'NONE',  ( -0.000000000000000000, -0.000000000000000000, -1.000000000000000000 ) ) ;
#429 = LINE ( 'NONE', #19037, #21295 ) ;
#430 = ORIENTED_EDGE ( 'NONE', *, *, #4985, .T. ) ;
#431 = VECTOR ( 'NONE', #12408, 1000.000000000000000 ) ;
#432 = CARTESIAN_POINT ( 'NONE',  ( 159.5152310637604955, -4.999999999999974243, -11.28819510263909542 ) ) ;
#433 = CARTESIAN_POINT ( 'NONE',  ( -13.00000000000001243, 55.00000000000000711, -23.00000000000000000 ) ) ;
#434 = ORIENTED_EDGE ( 'NONE', *, *, #645, .T. ) ;
#435 = CARTESIAN_POINT ( 'NONE',  ( 134.5152310637605524, -1.999999999999980460, -13.05155085951650840 ) ) ;
#436 = VERTEX_POINT ( 'NONE', #19791 ) ;
#437 = CARTESIAN_POINT ( 'NONE',  ( 9.667845848563926481, 16.22748053257927126, -17.88508528815513543 ) ) ;
#438 = VERTEX_POINT ( 'NONE', #10483 ) ;
#439 = EDGE_CURVE ( 'NONE', #26227, #4517, #895, .T. ) ;
#440 = AXIS2_PLACEMENT_3D ( 'NONE', #10772, #20082, #29458 ) ;
#441 = CARTESIAN_POINT ( 'NONE',  ( 25.04433344647707571, -4.420048373160954114, -18.22226412361657921 ) ) ;
#442 = EDGE_CURVE ( 'NONE', #18552, #1065, #26238, .T. ) ;
#443 = CARTESIAN_POINT ( 'NONE',  ( 21.55249387529322647, -4.041031698679099726, -14.19001464829599435 ) ) ;
#444 = LINE ( 'NONE', #2443, #25266 ) ;
#445 = CARTESIAN_POINT ( 'NONE',  ( -1.310872448937995705, 8.480771745766411129, -0.3173508448886640521 ) ) ;
#446 = EDGE_CURVE ( 'NONE', #20723, #20491, #23957, .T. ) ;
#447 = DIRECTION ( 'NONE',  ( -0.7172983783020613346, 0.6967661275386690667, -3.330669073875468142E-16 ) ) ;
#448 = CARTESIAN_POINT ( 'NONE',  ( 26.72181814967143509, -3.137724904577397389, -15.69709663067708050 ) ) ;
#449 = ORIENTED_EDGE ( 'NONE', *, *, #11568, .T. ) ;
#450 = DIRECTION ( 'NONE',  ( -1.110223024625156540E-16, 0.000000000000000000, -1.000000000000000000 ) ) ;
#451 = FACE_OUTER_BOUND ( 'NONE', #23218, .T. ) ;
#452 = VECTOR ( 'NONE', #19393, 1000.000000000000000 ) ;
#453 = DIRECTION ( 'NONE',  ( 0.3090169943749472292, 8.338696094057992503E-17, -0.9510565162951536422 ) ) ;
#454 = CARTESIAN_POINT ( 'NONE',  ( 63.44486372867152824, 109.8897274573438096, -186.4312945166758482 ) ) ;
#455 = LINE ( 'NONE', #21049, #14790 ) ;
#456 = CARTESIAN_POINT ( 'NONE',  ( 12.02305193244137449, 9.338961869187645704, -16.69339841729684437 ) ) ;
#457 = DIRECTION ( 'NONE',  ( 1.000000000000000000, 2.698458740408365879E-16, -1.110223024625156540E-16 ) ) ;
#458 = CARTESIAN_POINT ( 'NONE',  ( 34.96805304670973413, -19.57645325810014114, -20.18246498508359466 ) ) ;
#459 = ORIENTED_EDGE ( 'NONE', *, *, #24414, .T. ) ;
#460 = CARTESIAN_POINT ( 'NONE',  ( 13.81482270056995532, 7.818281081198240834, -15.36100202165747675 ) ) ;
#461 = VERTEX_POINT ( 'NONE', #21635 ) ;
#462 = DIRECTION ( 'NONE',  ( -1.000000000000000000, -4.440892098500623203E-16, 0.000000000000000000 ) ) ;
#463 = CARTESIAN_POINT ( 'NONE',  ( 21.66440995182641416, 5.535554982823286174, -17.57621636221614025 ) ) ;
#464 = CARTESIAN_POINT ( 'NONE',  ( 12.84801357566967717, 9.517348710814296453, -16.13078356789775469 ) ) ;
#465 = CARTESIAN_POINT ( 'NONE',  ( 130.7287565553229456, -4.999999999999983125, 3.500000000000003109 ) ) ;
#466 = ORIENTED_EDGE ( 'NONE', *, *, #9296, .T. ) ;
#467 = EDGE_CURVE ( 'NONE', #22249, #23534, #732, .T. ) ;
#468 = ORIENTED_EDGE ( 'NONE', *, *, #9842, .F. ) ;
#469 = CARTESIAN_POINT ( 'NONE',  ( 11.40798482813988635, 9.566882342703072695, -15.88774718835883348 ) ) ;
#470 = FACE_OUTER_BOUND ( 'NONE', #17896, .T. ) ;
#471 = CARTESIAN_POINT ( 'NONE',  ( 10.24089172292967298, 14.91932009296530559, -16.37038124228770997 ) ) ;
#472 = FACE_OUTER_BOUND ( 'NONE', #16901, .T. ) ;
#473 = ORIENTED_EDGE ( 'NONE', *, *, #13528, .T. ) ;
#474 = CARTESIAN_POINT ( 'NONE',  ( -4.000000000000010658, -2.309401076758525573, -0.3572655899081716435 ) ) ;
#475 = VERTEX_POINT ( 'NONE', #12779 ) ;
#476 = CARTESIAN_POINT ( 'NONE',  ( 10.40163623209820365, 16.77498095339038287, -17.46874319472340176 ) ) ;
#477 = ORIENTED_EDGE ( 'NONE', *, *, #15791, .T. ) ;
#478 = VECTOR ( 'NONE', #30246, 1000.000000000000000 ) ;
#479 = CARTESIAN_POINT ( 'NONE',  ( 32.45862320860160821, -9.597537451891041016, -17.61229109800368064 ) ) ;
#480 = CARTESIAN_POINT ( 'NONE',  ( 29.62588713853392264, -10.65184931322849060, -12.76488833982454629 ) ) ;
#481 = CARTESIAN_POINT ( 'NONE',  ( 29.46565128511723586, -7.689737916804423534, -14.82739468409561567 ) ) ;
#482 = ORIENTED_EDGE ( 'NONE', *, *, #14397, .T. ) ;
#483 = EDGE_CURVE ( 'NONE', #29391, #7152, #10029, .T. ) ;
#484 = CARTESIAN_POINT ( 'NONE',  ( 12.50940683846913970, -5.000000000000014211, 38.49999548658399107 ) ) ;
#485 = EDGE_CURVE ( 'NONE', #18308, #9388, #28550, .T. ) ;
#486 = VERTEX_POINT ( 'NONE', #7602 ) ;
#487 = EDGE_CURVE ( 'NONE', #4418, #10786, #7903, .T. ) ;
#488 = CIRCLE ( 'NONE', #12639, 4.000000000000000000 ) ;
#489 = EDGE_CURVE ( 'NONE', #20712, #9080, #7254, .T. ) ;
#490 = DIRECTION ( 'NONE',  ( -2.698458740408365879E-16, 1.000000000000000000, 0.000000000000000000 ) ) ;
#491 = SHAPE_DEFINITION_REPRESENTATION ( #26931, #5250 ) ;
#492 = CARTESIAN_POINT ( 'NONE',  ( 28.92040988821396752, -12.03996551347764132, -12.87516188627701474 ) ) ;
#493 = CARTESIAN_POINT ( 'NONE',  ( 26.45169718342334164, -9.008644514675534509, -18.11399877363951205 ) ) ;
#494 = ORIENTED_EDGE ( 'NONE', *, *, #2114, .T. ) ;
#495 = FACE_BOUND ( 'NONE', #28944, .T. ) ;
#496 =( GEOMETRIC_REPRESENTATION_CONTEXT ( 3 ) GLOBAL_UNCERTAINTY_ASSIGNED_CONTEXT ( ( #4915 ) ) GLOBAL_UNIT_ASSIGNED_CONTEXT ( ( #25066, #15887, #27085 ) ) REPRESENTATION_CONTEXT ( 'NONE', 'WORKASPACE' ) );
#497 = CARTESIAN_POINT ( 'NONE',  ( -2.500000000000002665, -1.110223024625156738E-15, -2.424599999999998978 ) ) ;
#498 = FACE_OUTER_BOUND ( 'NONE', #5684, .T. ) ;
#499 = VECTOR ( 'NONE', #27812, 1000.000000000000000 ) ;
#500 = DIRECTION ( 'NONE',  ( 0.9510565162951536422, 2.566386769018988816E-16, 0.3090169943749472292 ) ) ;
#501 = DIRECTION ( 'NONE',  ( -1.000000000000000000, -4.440892098500622217E-16, 0.000000000000000000 ) ) ;
#502 = CIRCLE ( 'NONE', #23914, 4.000000000000003553 ) ;
#503 = CARTESIAN_POINT ( 'NONE',  ( 10.33813570737955700, 18.38610344077106973, -17.89676158639688452 ) ) ;
#504 = DIRECTION ( 'NONE',  ( -2.698458740408365879E-16, 1.000000000000000000, 0.000000000000000000 ) ) ;
#505 = CARTESIAN_POINT ( 'NONE',  ( 162.0152310637605240, -9.999999999999998224, -34.70218595412750773 ) ) ;
#506 = VERTEX_POINT ( 'NONE', #26086 ) ;
#507 = CARTESIAN_POINT ( 'NONE',  ( 9.917965570771830386, 16.40030059027150600, -16.50392256580263606 ) ) ;
#508 = CARTESIAN_POINT ( 'NONE',  ( 20.43163981785493988, 0.2187255735321424754, -20.49791845872360341 ) ) ;
#509 = LINE ( 'NONE', #21850, #18033 ) ;
#510 = LINE ( 'NONE', #23703, #12518 ) ;
#511 = CARTESIAN_POINT ( 'NONE',  ( 137.0152310637605808, -1.999999999999980016, 1.702185954127501066 ) ) ;
#512 = ORIENTED_EDGE ( 'NONE', *, *, #5043, .F. ) ;
#513 = LINE ( 'NONE', #12092, #15899 ) ;
#514 = CARTESIAN_POINT ( 'NONE',  ( 11.27864710625743427, 16.66565394782951515, -16.78350969486689692 ) ) ;
#515 = AXIS2_PLACEMENT_3D ( 'NONE', #15266, #13594, #10844 ) ;
#516 = EDGE_LOOP ( 'NONE', ( #242, #27504, #8040, #18443, #3018 ) ) ;
#518 = VECTOR ( 'NONE', #4177, 1000.000000000000000 ) ;
#517 = CARTESIAN_POINT ( 'NONE',  ( 35.24753590068310416, -19.83202167481471889, -19.22462439892593977 ) ) ;
#519 = CARTESIAN_POINT ( 'NONE',  ( 17.72480397827495224, 1.356124466512965476, -19.40231245121514903 ) ) ;
#520 = EDGE_CURVE ( 'NONE', #12932, #5386, #5166, .T. ) ;
#521 = CARTESIAN_POINT ( 'NONE',  ( 130.7287565553229456, -4.999999999999983125, 3.500000000000003109 ) ) ;
#522 = CARTESIAN_POINT ( 'NONE',  ( 9.112135424753279977, 16.18318370314694832, -17.05489040841110437 ) ) ;
#523 = CARTESIAN_POINT ( 'NONE',  ( 24.27832910178602788, -5.559203070376852018, -13.12236226054620047 ) ) ;
#524 = ADVANCED_FACE ( 'NONE', ( #22562 ), #3633, .T. ) ;
#525 = ORIENTED_EDGE ( 'NONE', *, *, #27075, .F. ) ;
#526 = ADVANCED_FACE ( 'NONE', ( #15359 ), #12926, .T. ) ;
#527 = LINE ( 'NONE', #9813, #17849 ) ;
#528 =( NAMED_UNIT ( * ) SI_UNIT ( $, .STERADIAN. ) SOLID_ANGLE_UNIT ( ) );
#529 = MECHANICAL_DESIGN_GEOMETRIC_PRESENTATION_REPRESENTATION (  '', ( #42 ), #25882 ) ;
#530 = CARTESIAN_POINT ( 'NONE',  ( 21.58357356133149807, 4.347441036859617469, -17.91576365920758107 ) ) ;
#531 = CARTESIAN_POINT ( 'NONE',  ( 18.42634509371275797, 7.189141296957872740, -15.94500943014882210 ) ) ;
#532 = VECTOR ( 'NONE', #22824, 1000.000000000000000 ) ;
#533 = ORIENTED_EDGE ( 'NONE', *, *, #15684, .F. ) ;
#534 = LINE ( 'NONE', #822, #24024 ) ;
#535 = EDGE_LOOP ( 'NONE', ( #7211, #6231, #28486, #4893 ) ) ;
#536 = ORIENTED_EDGE ( 'NONE', *, *, #4318, .F. ) ;
#537 = CARTESIAN_POINT ( 'NONE',  ( 146.1922820468854525, -10.00000000000000178, -22.25671179336496053 ) ) ;
#538 = CARTESIAN_POINT ( 'NONE',  ( 139.5152310637605808, -10.00000000000000533, -21.71180489736090991 ) ) ;
#539 = VECTOR ( 'NONE', #19186, 999.9999999999998863 ) ;
#540 = CARTESIAN_POINT ( 'NONE',  ( 1.310872448937984602, -8.480771745766441327, -0.3173508448886784294 ) ) ;
#541 = DIRECTION ( 'NONE',  ( 0.000000000000000000, 0.000000000000000000, -1.000000000000000000 ) ) ;
#542 = VECTOR ( 'NONE', #24235, 1000.000000000000000 ) ;
#543 = CARTESIAN_POINT ( 'NONE',  ( 12.10607290817362092, -5.000000000000014211, -37.25866128932931787 ) ) ;
#544 = ORIENTED_EDGE ( 'NONE', *, *, #13525, .F. ) ;
#545 = CARTESIAN_POINT ( 'NONE',  ( 9.916411867603999397, 16.40742607105030260, -16.50456570466356965 ) ) ;
#546 = CARTESIAN_POINT ( 'NONE',  ( 28.54819463643023880, -8.737303380947411213, -14.37855314081258307 ) ) ;
#547 = CARTESIAN_POINT ( 'NONE',  ( 20.97044927184332508, -4.289323992320570156, -15.06659861376252429 ) ) ;
#548 = EDGE_CURVE ( 'NONE', #20384, #24083, #19953, .T. ) ;
#550 = ORIENTED_EDGE ( 'NONE', *, *, #23991, .F. ) ;
#549 = CARTESIAN_POINT ( 'NONE',  ( 32.45272648307624053, -11.02157468472264412, -17.82583700188536824 ) ) ;
#551 = FACE_OUTER_BOUND ( 'NONE', #15661, .T. ) ;
#552 = DIRECTION ( 'NONE',  ( 0.9510565162951536422, 0.000000000000000000, -0.3090169943749475623 ) ) ;
#553 = DIRECTION ( 'NONE',  ( -0.000000000000000000, -1.000000000000000000, -0.000000000000000000 ) ) ;
#554 = CARTESIAN_POINT ( 'NONE',  ( 148.6922820468854525, -4.999999999999976907, -23.73366926340167637 ) ) ;
#555 = CARTESIAN_POINT ( 'NONE',  ( 16.09764958744793262, 8.143416238145906760, -19.84970969296679044 ) ) ;
#556 = EDGE_LOOP ( 'NONE', ( #3105, #12356, #15207, #22632, #19486 ) ) ;
#557 = FACE_OUTER_BOUND ( 'NONE', #419, .T. ) ;
#558 = CARTESIAN_POINT ( 'NONE',  ( 10.33819201225523621, 18.38584521943398187, -17.87775236254758227 ) ) ;
#559 = LINE ( 'NONE', #9844, #18339 ) ;
#560 = DIRECTION ( 'NONE',  ( 2.698458740408365879E-16, -1.000000000000000000, 0.000000000000000000 ) ) ;
#561 = CARTESIAN_POINT ( 'NONE',  ( 17.32695330507268494, 5.471673316493076200, -20.08600194542987794 ) ) ;
#562 = CARTESIAN_POINT ( 'NONE',  ( 16.38450301900381945, 9.168174629645104545, -21.04437084800770918 ) ) ;
#563 = VERTEX_POINT ( 'NONE', #10643 ) ;
#565 = AXIS2_PLACEMENT_3D ( 'NONE', #8777, #15341, #10624 ) ;
#564 = CARTESIAN_POINT ( 'NONE',  ( 32.45272648307624053, -11.02157468472264412, -17.82583700188536824 ) ) ;
#566 = CARTESIAN_POINT ( 'NONE',  ( 23.60892706051935619, -2.861763136178346212, -14.25286661070829908 ) ) ;
#567 = AXIS2_PLACEMENT_3D ( 'NONE', #11521, #19011, #13959 ) ;
#568 = CARTESIAN_POINT ( 'NONE',  ( 22.48601049859325585, 2.925819830077934558, -17.76611561182923893 ) ) ;
#569 = CARTESIAN_POINT ( 'NONE',  ( 28.63790973356518776, -5.888324979419876648, -13.82040474618100312 ) ) ;
#570 = VERTEX_POINT ( 'NONE', #8354 ) ;
#571 = CARTESIAN_POINT ( 'NONE',  ( 129.5152310637605808, -10.00000000000000888, -11.28819510263909187 ) ) ;
#573 = ORIENTED_EDGE ( 'NONE', *, *, #19437, .T. ) ;
#572 = DIRECTION ( 'NONE',  ( -0.9510565162951536422, 0.000000000000000000, -0.3090169943749472292 ) ) ;
#574 = DIRECTION ( 'NONE',  ( -0.8090169943749474513, -2.183098979609982436E-16, -0.5877852522924731371 ) ) ;
#575 = DIRECTION ( 'NONE',  ( 0.9510565162951536422, 0.000000000000000000, -0.3090169943749475623 ) ) ;
#576 = ADVANCED_FACE ( 'NONE', ( #3939 ), #15213, .T. ) ;
#577 = CARTESIAN_POINT ( 'NONE',  ( 32.71419323209526908, -10.28616775856061416, -16.33292762241428520 ) ) ;
#578 = AXIS2_PLACEMENT_3D ( 'NONE', #20455, #15424, #27383 ) ;
#579 = CARTESIAN_POINT ( 'NONE',  ( 9.641354186875979337, 17.66887565656821124, -17.90893343548146177 ) ) ;
#580 = PRODUCT_DEFINITION ( 'UNKNOWN', '', #1483, #2194 ) ;
#581 = DIRECTION ( 'NONE',  ( 0.3090169943749472292, 8.338696094057992503E-17, -0.9510565162951536422 ) ) ;
#582 = CARTESIAN_POINT ( 'NONE',  ( 106.2677862141057545, -4.999999999999988454, -77.20806604152963359 ) ) ;
#583 = CARTESIAN_POINT ( 'NONE',  ( 13.10707286029108865, 8.563798077496334926, -15.92507172258792281 ) ) ;
#584 = CARTESIAN_POINT ( 'NONE',  ( 138.6922820468854525, -4.999999999999980460, -23.73366926340167282 ) ) ;
#585 = CARTESIAN_POINT ( 'NONE',  ( 153.6922820468854241, -1.999999999999974465, -23.73366926340167637 ) ) ;
#586 = ORIENTED_EDGE ( 'NONE', *, *, #25073, .T. ) ;
#587 = DIRECTION ( 'NONE',  ( -0.5877852522924731371, 0.000000000000000000, 0.8090169943749474513 ) ) ;
#588 = CARTESIAN_POINT ( 'NONE',  ( 142.0152310637605808, -1.999999999999978018, -26.04193191628310800 ) ) ;
#589 = ORIENTED_EDGE ( 'NONE', *, *, #23254, .T. ) ;
#590 = VERTEX_POINT ( 'NONE', #3789 ) ;
#591 = EDGE_LOOP ( 'NONE', ( #6929, #8428, #23827, #25905 ) ) ;
#592 = ORIENTED_EDGE ( 'NONE', *, *, #18201, .T. ) ;
#593 = CARTESIAN_POINT ( 'NONE',  ( 11.22273001195053155, 9.096583557657577757, -17.24208598844832352 ) ) ;
#594 = CARTESIAN_POINT ( 'NONE',  ( 27.63487812444411418, -5.020849242181972372, -17.14317672846274831 ) ) ;
#595 = CARTESIAN_POINT ( 'NONE',  ( 26.02348467347448491, -3.622150272347476108, -19.21400332953221124 ) ) ;
#596 = CARTESIAN_POINT ( 'NONE',  ( 143.6922820468854525, -10.00000000000000355, -17.92658477444275889 ) ) ;
#597 = DIRECTION ( 'NONE',  ( -2.207829878515935943E-16, 1.000000000000000000, 0.000000000000000000 ) ) ;
#598 = VECTOR ( 'NONE', #146, 1000.000000000000000 ) ;
#599 = CARTESIAN_POINT ( 'NONE',  ( 15.12871522451188788, -5.000000000000013323, -46.56139778509288618 ) ) ;
#600 = VERTEX_POINT ( 'NONE', #24546 ) ;
#601 = CARTESIAN_POINT ( 'NONE',  ( 175.7287565553229456, -4.999999999999969802, -4.785595155761525277 ) ) ;
#602 = CARTESIAN_POINT ( 'NONE',  ( 35.54859390953723874, -22.18451583373416014, -15.00000000000000000 ) ) ;
#603 = CARTESIAN_POINT ( 'NONE',  ( 34.54859390953723874, -22.18451583373416014, -18.00000000000000000 ) ) ;
#604 = CARTESIAN_POINT ( 'NONE',  ( 148.6922820468854525, -1.999999999999977129, -32.39392330124607611 ) ) ;
#605 = CARTESIAN_POINT ( 'NONE',  ( 12.02786405831828986, 9.316892843345049968, -16.69140843421181231 ) ) ;
#606 = ADVANCED_FACE ( 'NONE', ( #5928 ), #17657, .T. ) ;
#607 = ADVANCED_FACE ( 'NONE', ( #6073 ), #13083, .T. ) ;
#608 = PLANE ( 'NONE',  #6779 ) ;
#609 = CARTESIAN_POINT ( 'NONE',  ( 32.54305136433941215, -11.03529315477374517, -18.08112484791816499 ) ) ;
#610 = ORIENTED_EDGE ( 'NONE', *, *, #3790, .F. ) ;
#611 = CARTESIAN_POINT ( 'NONE',  ( 8.944584663113916534, 16.95159285377954461, -17.91618150236991269 ) ) ;
#612 = EDGE_CURVE ( 'NONE', #12774, #3207, #13241, .T. ) ;
#613 = FACE_OUTER_BOUND ( 'NONE', #14035, .T. ) ;
#614 = AXIS2_PLACEMENT_3D ( 'NONE', #19499, #24547, #12781 ) ;
#615 = ADVANCED_FACE ( 'NONE', ( #17802 ), #27165, .T. ) ;
#616 = CARTESIAN_POINT ( 'NONE',  ( 23.86551563699305234, 2.542095107771292106, -17.79649620197707094 ) ) ;
#617 = CARTESIAN_POINT ( 'NONE',  ( 12.83210864641033844, 9.541281304504437344, -16.14109870176968897 ) ) ;
#618 = CARTESIAN_POINT ( 'NONE',  ( 162.0152310637604955, -4.999999999999974243, -26.04193191628311155 ) ) ;
#619 = VERTEX_POINT ( 'NONE', #5420 ) ;
#620 = CARTESIAN_POINT ( 'NONE',  ( 11.47029057985033340, 9.281140223223081520, -15.86198156829250117 ) ) ;
#621 = CARTESIAN_POINT ( 'NONE',  ( 416.0000000000002274, 34.64101615137744972, 14.00000000000000178 ) ) ;
#622 = CARTESIAN_POINT ( 'NONE',  ( 9.745779815811758340, 17.18996641109745482, -16.82979807527155458 ) ) ;
#623 = CARTESIAN_POINT ( 'NONE',  ( 175.7287565553229456, -9.999999999999971578, 0.5000000000000029976 ) ) ;
#624 = ORIENTED_EDGE ( 'NONE', *, *, #10904, .F. ) ;
#625 = CARTESIAN_POINT ( 'NONE',  ( 173.6922820468853388, -9.999999999999994671, -26.58683881228715862 ) ) ;
#626 = ORIENTED_EDGE ( 'NONE', *, *, #26015, .T. ) ;
#627 = CARTESIAN_POINT ( 'NONE',  ( 12.00785540763395254, 9.408655069060824161, -16.69968271487400813 ) ) ;
#628 = ORIENTED_EDGE ( 'NONE', *, *, #27617, .T. ) ;
#629 = CARTESIAN_POINT ( 'NONE',  ( 36.54859390954303677, -22.18451583373416014, -15.55638201429745848 ) ) ;
#630 = CARTESIAN_POINT ( 'NONE',  ( 30.24922550192677306, -10.40856591028444278, -13.02298783260255988 ) ) ;
#631 = CARTESIAN_POINT ( 'NONE',  ( 27.11191462667604313, -11.78482644060662743, -13.28705938033944989 ) ) ;
#632 = CIRCLE ( 'NONE', #16698, 4.000000000000000000 ) ;
#633 = VERTEX_POINT ( 'NONE', #8295 ) ;
#634 = CARTESIAN_POINT ( 'NONE',  ( -5.000000000000006217, -1.608122649676636551E-15, -25.03750572909317285 ) ) ;
#635 = CARTESIAN_POINT ( 'NONE',  ( 112.3900446700832845, -4.999999999999986677, -81.65614717723775584 ) ) ;
#636 = CARTESIAN_POINT ( 'NONE',  ( 17.00902653454025071, 3.367308883600929281, -16.20218648120260951 ) ) ;
#637 = CARTESIAN_POINT ( 'NONE',  ( 26.84622329165386745, -11.42663724297536554, -16.80226328336580366 ) ) ;
#638 = VECTOR ( 'NONE', #15059, 1000.000000000000000 ) ;
#639 = CARTESIAN_POINT ( 'NONE',  ( 0.000000000000000000, 0.000000000000000000, -5.000000000000000888 ) ) ;
#640 = FACE_BOUND ( 'NONE', #17221, .T. ) ;
#641 = ORIENTED_EDGE ( 'NONE', *, *, #6603, .T. ) ;
#642 = CARTESIAN_POINT ( 'NONE',  ( 17.67390002678752126, -5.000000000000013323, -54.39467115012526932 ) ) ;
#643 = DIRECTION ( 'NONE',  ( 0.000000000000000000, -1.000000000000000000, 0.000000000000000000 ) ) ;
#644 = CARTESIAN_POINT ( 'NONE',  ( 95.18167920860219056, -4.999999999999991118, -69.15353783201314286 ) ) ;
#645 = EDGE_CURVE ( 'NONE', #3816, #11753, #19590, .T. ) ;
#646 = DIRECTION ( 'NONE',  ( -0.9510565162951536422, -2.566386769018988323E-16, 0.3090169943749475623 ) ) ;
#647 = EDGE_CURVE ( 'NONE', #21669, #19416, #14705, .T. ) ;
#648 = ADVANCED_FACE ( 'NONE', ( #29106 ), #6773, .F. ) ;
#649 = CARTESIAN_POINT ( 'NONE',  ( 12.26681336913932974, 9.540941834721429871, -15.31486507153535648 ) ) ;
#650 = CARTESIAN_POINT ( 'NONE',  ( -8.000000000000000000, 4.618802153517001408, -0.7145311798163294092 ) ) ;
#651 = ORIENTED_EDGE ( 'NONE', *, *, #17517, .T. ) ;
#652 = FACE_OUTER_BOUND ( 'NONE', #21709, .T. ) ;
#653 = VERTEX_POINT ( 'NONE', #12872 ) ;
#654 = CARTESIAN_POINT ( 'NONE',  ( 12.23783994716398560, 8.515526397163364791, -15.33449341356891615 ) ) ;
#655 = VECTOR ( 'NONE', #19725, 1000.000000000000000 ) ;
#656 = CARTESIAN_POINT ( 'NONE',  ( 17.93652952100233833, 4.843921488302829204, -14.86957952233187896 ) ) ;
#657 = CARTESIAN_POINT ( 'NONE',  ( -16.00000000000017053, 34.64101615137744972, 4.999999999999998224 ) ) ;
#658 = CARTESIAN_POINT ( 'NONE',  ( 10.52062816623737618, -5.000000000000015099, 32.37916410797102884 ) ) ;
#659 = DIRECTION ( 'NONE',  ( -0.8090169943749474513, -2.183098979609982436E-16, -0.5877852522924731371 ) ) ;
#660 = DIRECTION ( 'NONE',  ( 0.9510565162951536422, 0.000000000000000000, -0.3090169943749475623 ) ) ;
#661 = CARTESIAN_POINT ( 'NONE',  ( 12.83625023806442655, 9.529724225483313660, -16.13881881377442795 ) ) ;
#662 = EDGE_LOOP ( 'NONE', ( #30038, #11644, #23930, #20941 ) ) ;
#663 = CARTESIAN_POINT ( 'NONE',  ( 33.57416420788476330, -12.34692739235205217, -18.69991813917680190 ) ) ;
#664 = CARTESIAN_POINT ( 'NONE',  ( 14.33367420948735393, 6.252843122977492563, -16.41390433006782956 ) ) ;
#665 = DIRECTION ( 'NONE',  ( -0.5877852522924731371, 0.000000000000000000, 0.8090169943749474513 ) ) ;
#666 = CARTESIAN_POINT ( 'NONE',  ( 22.02790516022008660, -6.446180030103099590, -16.19395709203531197 ) ) ;
#667 = EDGE_LOOP ( 'NONE', ( #22957, #26404, #26057, #11822 ) ) ;
#668 = PLANE ( 'NONE',  #10055 ) ;
#669 = AXIS2_PLACEMENT_3D ( 'NONE', #29808, #9407, #6697 ) ;
#670 = CARTESIAN_POINT ( 'NONE',  ( 21.81760893248375766, -3.923850722439390815, -13.93537712798182682 ) ) ;
#671 = CARTESIAN_POINT ( 'NONE',  ( 15.53255613197921647, 5.987779765840379298, -16.04456276566740058 ) ) ;
#672 = FACE_OUTER_BOUND ( 'NONE', #3393, .T. ) ;
#673 = ORIENTED_EDGE ( 'NONE', *, *, #5089, .F. ) ;
#674 = EDGE_LOOP ( 'NONE', ( #23723, #129, #3090, #8885 ) ) ;
#675 = DIRECTION ( 'NONE',  ( -0.000000000000000000, 1.000000000000000000, -0.000000000000000000 ) ) ;
#676 = AXIS2_PLACEMENT_3D ( 'NONE', #24862, #20114, #1970 ) ;
#677 = DIRECTION ( 'NONE',  ( -1.000000000000000000, 0.000000000000000000, -0.000000000000000000 ) ) ;
#678 = CARTESIAN_POINT ( 'NONE',  ( 2.309976723937608778, -7.903938623646900474, -0.1306530452038287271 ) ) ;
#679 = LINE ( 'NONE', #23575, #7743 ) ;
#680 = EDGE_CURVE ( 'NONE', #19492, #2298, #29262, .T. ) ;
#681 = EDGE_CURVE ( 'NONE', #10452, #25209, #7995, .T. ) ;
#682 = FACE_BOUND ( 'NONE', #6347, .T. ) ;
#683 = ADVANCED_FACE ( 'NONE', ( #15154 ), #3431, .F. ) ;
#684 = CARTESIAN_POINT ( 'NONE',  ( 11.47748818427356987, 9.248962635895034978, -15.85894168489154765 ) ) ;
#685 = EDGE_CURVE ( 'NONE', #16894, #18003, #12723, .T. ) ;
#686 = CARTESIAN_POINT ( 'NONE',  ( 29.25528888857379783, -9.059906918047152757, -17.02304095575280130 ) ) ;
#687 = CARTESIAN_POINT ( 'NONE',  ( 21.37428249720081297, 2.009508332918806151, -14.44682725892062614 ) ) ;
#689 = ORIENTED_EDGE ( 'NONE', *, *, #5256, .F. ) ;
#688 = CARTESIAN_POINT ( 'NONE',  ( 35.54750751241274287, -23.17963522693337453, -18.53372063443203999 ) ) ;
#690 = CARTESIAN_POINT ( 'NONE',  ( 173.6922820468853388, -1.999999999999969580, -26.58683881228715862 ) ) ;
#691 = CARTESIAN_POINT ( 'NONE',  ( -1.321505333908961966, 3.855830693249140406, -2.415789719053470730 ) ) ;
#692 = LINE ( 'NONE', #7853, #7318 ) ;
#693 = DIRECTION ( 'NONE',  ( -2.698458740408365879E-16, 1.000000000000000000, 0.000000000000000000 ) ) ;
#694 = CARTESIAN_POINT ( 'NONE',  ( 3.673643420401897508, 2.497823135841249709, -2.201519936625011553 ) ) ;
#695 = CARTESIAN_POINT ( 'NONE',  ( 20.52488529563827058, 3.974637744936419637, -19.97762432673833288 ) ) ;
#696 = ORIENTED_EDGE ( 'NONE', *, *, #23243, .F. ) ;
#697 = CARTESIAN_POINT ( 'NONE',  ( 137.2287565553230309, -10.00000000000000533, -12.16987298107780013 ) ) ;
#698 = CARTESIAN_POINT ( 'NONE',  ( 10.72031594518761466, 16.63337615353409760, -15.95439753950889106 ) ) ;
#699 = DIRECTION ( 'NONE',  ( 1.000000000000000000, 2.908569913943825554E-16, -6.938893903907227392E-16 ) ) ;
#700 = CARTESIAN_POINT ( 'NONE',  ( 0.000000000000000000, 2.357898499370430834, -3.469446951953614189E-15 ) ) ;
#701 = ORIENTED_EDGE ( 'NONE', *, *, #6410, .F. ) ;
#702 = CARTESIAN_POINT ( 'NONE',  ( 22.29983652437130814, 0.6627547066652448304, -20.09853802436992964 ) ) ;
#703 = AXIS2_PLACEMENT_3D ( 'NONE', #17964, #20256, #19964 ) ;
#704 = CARTESIAN_POINT ( 'NONE',  ( 28.86700826148938859, -9.048814421258168039, -19.66053155205330683 ) ) ;
#705 = VERTEX_POINT ( 'NONE', #19891 ) ;
#706 = CARTESIAN_POINT ( 'NONE',  ( 35.32886446602115171, -21.19738783794349857, -20.03221113960638178 ) ) ;
#707 = CARTESIAN_POINT ( 'NONE',  ( 22.40033610297568956, 1.362009800809227178, -14.54093962742820700 ) ) ;
#708 = CARTESIAN_POINT ( 'NONE',  ( 19.97593658988278165, 3.663230212540239616, -18.70116431613266883 ) ) ;
#709 = PLANE ( 'NONE',  #9392 ) ;
#710 = CARTESIAN_POINT ( 'NONE',  ( 143.6922820468854525, -1.999999999999977573, -32.39392330124607611 ) ) ;
#711 = LINE ( 'NONE', #7438, #3635 ) ;
#712 = VECTOR ( 'NONE', #11065, 1000.000000000000000 ) ;
#713 = EDGE_CURVE ( 'NONE', #23249, #7514, #4350, .T. ) ;
#714 = CARTESIAN_POINT ( 'NONE',  ( -4.000000000000005329, 0.7862748000878123644, -2.415527722372433406 ) ) ;
#715 = CARTESIAN_POINT ( 'NONE',  ( 34.70514358766799745, -13.90287004036446739, -20.03273298744158737 ) ) ;
#716 = CARTESIAN_POINT ( 'NONE',  ( 12.81042928357508970, 7.649856678006609734, -14.88275739421262855 ) ) ;
#717 = CARTESIAN_POINT ( 'NONE',  ( 174.5152310637604103, -9.999999999999994671, -13.05155085951651195 ) ) ;
#718 = CARTESIAN_POINT ( 'NONE',  ( 19.66267869901929188, -5.000000000000012434, -60.51550252873825286 ) ) ;
#719 = CARTESIAN_POINT ( 'NONE',  ( 13.12048998592846871, 8.569482736746577345, -15.91439669260688561 ) ) ;
#720 = CARTESIAN_POINT ( 'NONE',  ( 0.2500000000000002220, 5.204748896376250699E-16, -4.250000000000000000 ) ) ;
#721 = DIRECTION ( 'NONE',  ( -1.000000000000000000, 0.000000000000000000, -0.000000000000000000 ) ) ;
#722 = VERTEX_POINT ( 'NONE', #26337 ) ;
#723 = FACE_OUTER_BOUND ( 'NONE', #23667, .T. ) ;
#724 = PLANE ( 'NONE',  #2987 ) ;
#725 = ORIENTED_EDGE ( 'NONE', *, *, #25327, .F. ) ;
#726 = ORIENTED_EDGE ( 'NONE', *, *, #7705, .F. ) ;
#727 = ORIENTED_EDGE ( 'NONE', *, *, #5882, .T. ) ;
#728 = CARTESIAN_POINT ( 'NONE',  ( 11.21893088074867073, 9.114006857625895464, -17.24365706284262600 ) ) ;
#729 = CARTESIAN_POINT ( 'NONE',  ( 24.63339645208565543, -5.721020077635508905, -14.05062826560360278 ) ) ;
#730 = CARTESIAN_POINT ( 'NONE',  ( 20.05514754915220266, -1.452567280579552866, -14.87399747198034738 ) ) ;
#731 = DIRECTION ( 'NONE',  ( -0.5877852522924731371, -1.586114251531760235E-16, 0.8090169943749474513 ) ) ;
#732 = LINE ( 'NONE', #12472, #2865 ) ;
#733 = CARTESIAN_POINT ( 'NONE',  ( 175.7287565553229456, -9.999999999999971578, 3.500000000000003109 ) ) ;
#734 = ADVANCED_FACE ( 'NONE', ( #24048 ), #17453, .T. ) ;
#735 = PRODUCT_DEFINITION ( 'UNKNOWN', '', #23906, #23852 ) ;
#736 = ORIENTED_EDGE ( 'NONE', *, *, #27325, .F. ) ;
#737 = ORIENTED_EDGE ( 'NONE', *, *, #24223, .F. ) ;
#738 = FACE_OUTER_BOUND ( 'NONE', #7045, .T. ) ;
#739 = CARTESIAN_POINT ( 'NONE',  ( 162.0152310637604387, -9.999999999999998224, -8.721423840594312082 ) ) ;
#740 = LINE ( 'NONE', #17220, #4845 ) ;
#741 = LINE ( 'NONE', #28713, #2500 ) ;
#742 = PLANE ( 'NONE',  #29494 ) ;
#743 = CARTESIAN_POINT ( 'NONE',  ( 10.79618582965528439, 14.96552620561766567, -17.20075070836251996 ) ) ;
#744 = CARTESIAN_POINT ( 'NONE',  ( 173.6922820468853388, -1.999999999999969580, -26.58683881228715862 ) ) ;
#745 = CARTESIAN_POINT ( 'NONE',  ( 33.55945865873172096, -12.30028340163019607, -18.68418013052470883 ) ) ;
#746 = ORIENTED_EDGE ( 'NONE', *, *, #23165, .F. ) ;
#747 = CARTESIAN_POINT ( 'NONE',  ( 13.39286676965551059, 7.631811206235384226, -15.69730834661896424 ) ) ;
#748 = PLANE ( 'NONE',  #14393 ) ;
#749 = VECTOR ( 'NONE', #646, 999.9999999999998863 ) ;
#750 = CARTESIAN_POINT ( 'NONE',  ( 21.69765170278760280, -5.035756590920279940, -14.89200278627170881 ) ) ;
#751 = CARTESIAN_POINT ( 'NONE',  ( 12.86751881037522871, 9.515731068868671372, -16.11601834121851340 ) ) ;
#752 = CARTESIAN_POINT ( 'NONE',  ( 19.99999999999998934, 55.00000000000000711, -30.00000000000000000 ) ) ;
#753 = ORIENTED_EDGE ( 'NONE', *, *, #7733, .T. ) ;
#754 = ORIENTED_EDGE ( 'NONE', *, *, #14477, .F. ) ;
#755 = ORIENTED_EDGE ( 'NONE', *, *, #24801, .T. ) ;
#756 = VERTEX_POINT ( 'NONE', #10428 ) ;
#757 = CARTESIAN_POINT ( 'NONE',  ( 11.47155695691762212, 9.275332456566969697, -15.86145787682774078 ) ) ;
#758 = LINE ( 'NONE', #26413, #24784 ) ;
#759 = CARTESIAN_POINT ( 'NONE',  ( 9.870716668364401869, 16.61699007954640805, -16.53972800451630931 ) ) ;
#760 = PLANE ( 'NONE',  #1860 ) ;
#761 = EDGE_LOOP ( 'NONE', ( #18408, #5576, #23225, #4103 ) ) ;
#762 = ORIENTED_EDGE ( 'NONE', *, *, #27042, .F. ) ;
#763 = CARTESIAN_POINT ( 'NONE',  ( 154.7287565553229456, -10.00000000000000178, -7.839745962155603820 ) ) ;
#764 = EDGE_LOOP ( 'NONE', ( #22617, #12498, #2134, #26269 ) ) ;
#765 = CARTESIAN_POINT ( 'NONE',  ( 12.02932678857878734, 9.310239991255825132, -16.69079931733866218 ) ) ;
#766 = VECTOR ( 'NONE', #5113, 1000.000000000000000 ) ;
#767 = ORIENTED_EDGE ( 'NONE', *, *, #14651, .T. ) ;
#768 = CARTESIAN_POINT ( 'NONE',  ( 36.54859682288668665, -23.18452892187019643, -18.24988411864624993 ) ) ;
#769 = CARTESIAN_POINT ( 'NONE',  ( 24.62590367393082502, -9.567571807129121808, -15.85044010117769098 ) ) ;
#770 = CARTESIAN_POINT ( 'NONE',  ( 31.22280883588763700, -10.09333740185288875, -13.86128061636125786 ) ) ;
#771 = AXIS2_PLACEMENT_3D ( 'NONE', #11121, #24875, #20422 ) ;
#772 = CARTESIAN_POINT ( 'NONE',  ( 131.1922820468854241, -10.00000000000000888, -28.06379628232387446 ) ) ;
#773 = CARTESIAN_POINT ( 'NONE',  ( 34.31936231504242585, -12.17391896401218609, -19.91370162440023250 ) ) ;
#774 = PRODUCT_CONTEXT ( 'NONE', #9279, 'mechanical' ) ;
#775 = EDGE_CURVE ( 'NONE', #20254, #13743, #1148, .T. ) ;
#776 = EDGE_CURVE ( 'NONE', #8035, #18677, #840, .T. ) ;
#777 = CARTESIAN_POINT ( 'NONE',  ( 18.73405575602592776, 1.888441813480535414, -14.99786396448725156 ) ) ;
#778 = VECTOR ( 'NONE', #13223, 1000.000000000000000 ) ;
#779 = EDGE_CURVE ( 'NONE', #2626, #23142, #19737, .T. ) ;
#780 = CARTESIAN_POINT ( 'NONE',  ( 14.79111372287554715, 6.954724682967856175, -19.27298399620107361 ) ) ;
#781 = AXIS2_PLACEMENT_3D ( 'NONE', #25947, #14624, #462 ) ;
#782 = ORIENTED_EDGE ( 'NONE', *, *, #29502, .F. ) ;
#783 = EDGE_CURVE ( 'NONE', #2732, #4135, #16160, .T. ) ;
#784 = DIRECTION ( 'NONE',  ( -2.698458740408365879E-16, 1.000000000000000000, 0.000000000000000000 ) ) ;
#785 = LINE ( 'NONE', #3830, #14240 ) ;
#786 = CIRCLE ( 'NONE', #8089, 4.000000000000004441 ) ;
#787 = CARTESIAN_POINT ( 'NONE',  ( 173.6922820468852819, -1.999999999999970468, -9.266330736598359152 ) ) ;
#788 = DIRECTION ( 'NONE',  ( -0.5877852522924731371, -1.586114251531760235E-16, 0.8090169943749474513 ) ) ;
#789 = CARTESIAN_POINT ( 'NONE',  ( 2.500000000000000444, -1.178949249685215417, 2.042000000000002036 ) ) ;
#790 = CARTESIAN_POINT ( 'NONE',  ( 0.000000000000000000, 0.000000000000000000, 23.00000000000000000 ) ) ;
#791 = VECTOR ( 'NONE', #22194, 1000.000000000000000 ) ;
#792 = CARTESIAN_POINT ( 'NONE',  ( 12.27691635572497830, 9.494607244959519576, -15.31068720787289728 ) ) ;
#793 = DIRECTION ( 'NONE',  ( -0.8090169943749474513, -2.183098979609982436E-16, 0.5877852522924731371 ) ) ;
#794 = ORIENTED_EDGE ( 'NONE', *, *, #25575, .T. ) ;
#795 = LINE ( 'NONE', #12527, #27612 ) ;
#796 = ORIENTED_EDGE ( 'NONE', *, *, #28150, .F. ) ;
#797 = CIRCLE ( 'NONE', #26173, 8.000000000000003553 ) ;
#798 = CARTESIAN_POINT ( 'NONE',  ( 12.50226005284522657, 8.571700941790735939, -15.12837371066060221 ) ) ;
#799 = EDGE_LOOP ( 'NONE', ( #24798, #19228, #20118, #16821 ) ) ;
#800 = VECTOR ( 'NONE', #21735, 1000.000000000000000 ) ;
#801 = CARTESIAN_POINT ( 'NONE',  ( 19.55603740332541918, 4.113176889600292263, -19.54140316641015573 ) ) ;
#802 = CARTESIAN_POINT ( 'NONE',  ( 152.0152310637604955, -4.999999999999976907, 1.702185954127501066 ) ) ;
#803 = LINE ( 'NONE', #7961, #4727 ) ;
#804 = CARTESIAN_POINT ( 'NONE',  ( 133.6922820468854241, -10.00000000000000711, -23.73366926340167282 ) ) ;
#805 = LINE ( 'NONE', #26606, #5198 ) ;
#806 = ORIENTED_EDGE ( 'NONE', *, *, #20326, .T. ) ;
#807 = CARTESIAN_POINT ( 'NONE',  ( 12.57288446902313872, 10.73011642529405307, -16.24829701787703939 ) ) ;
#808 = ORIENTED_EDGE ( 'NONE', *, *, #14405, .T. ) ;
#809 = CARTESIAN_POINT ( 'NONE',  ( 34.19542162461613799, -15.10542955289956346, -18.90659549333309286 ) ) ;
#810 = CARTESIAN_POINT ( 'NONE',  ( 15.14574614762244487, 6.587483969391940697, -15.14885142785537830 ) ) ;
#811 = CARTESIAN_POINT ( 'NONE',  ( 132.2287565553230024, -1.999999999999981348, -20.83012701892220164 ) ) ;
#812 = CARTESIAN_POINT ( 'NONE',  ( 16.96387855261641775, 8.441957738943033362, -20.67322241009641814 ) ) ;
#813 = ORIENTED_EDGE ( 'NONE', *, *, #2594, .T. ) ;
#814 = CARTESIAN_POINT ( 'NONE',  ( 137.0152310637605808, -4.999999999999980460, -8.721423840594312082 ) ) ;
#815 = EDGE_CURVE ( 'NONE', #4780, #461, #13982, .T. ) ;
#816 = CARTESIAN_POINT ( 'NONE',  ( 21.34960977245966873, -3.524359730468174412, -18.69795900347392248 ) ) ;
#817 = EDGE_CURVE ( 'NONE', #1754, #23532, #7703, .T. ) ;
#818 = CARTESIAN_POINT ( 'NONE',  ( 17.70496941102466693, 2.403166580496164606, -19.15355645582771871 ) ) ;
#819 = EDGE_CURVE ( 'NONE', #18037, #28074, #13165, .T. ) ;
#820 = AXIS2_PLACEMENT_3D ( 'NONE', #9199, #2219, #20356 ) ;
#821 = ORIENTED_EDGE ( 'NONE', *, *, #21331, .F. ) ;
#822 = CARTESIAN_POINT ( 'NONE',  ( 168.6922820468853388, -9.999999999999996447, -17.92658477444275889 ) ) ;
#823 = EDGE_CURVE ( 'NONE', #15263, #5003, #24622, .T. ) ;
#824 = EDGE_LOOP ( 'NONE', ( #12649, #746, #9170, #22264 ) ) ;
#825 = CARTESIAN_POINT ( 'NONE',  ( 134.7287565553230024, -10.00000000000000711, -16.50000000000000000 ) ) ;
#826 = AXIS2_PLACEMENT_3D ( 'NONE', #24727, #13267, #11272 ) ;
#827 = AXIS2_PLACEMENT_3D ( 'NONE', #15460, #13176, #18050 ) ;
#828 = DIRECTION ( 'NONE',  ( 1.665334536937734318E-16, -2.498001805406601723E-16, -1.000000000000000000 ) ) ;
#829 = CARTESIAN_POINT ( 'NONE',  ( 110.8088082477345750, -4.999999999999987566, -80.50731166957035612 ) ) ;
#830 = VECTOR ( 'NONE', #26631, 1000.000000000000000 ) ;
#831 = LINE ( 'NONE', #16848, #1420 ) ;
#832 = CARTESIAN_POINT ( 'NONE',  ( -8.000000000000003553, -4.618802153517037823, -0.7145311798163362926 ) ) ;
#833 = CARTESIAN_POINT ( 'NONE',  ( 11.55687758731922798, 9.016417257711555777, -15.81607864292198329 ) ) ;
#834 = CARTESIAN_POINT ( 'NONE',  ( 26.64397501440380012, -9.555891369342745634, -14.23407566704858951 ) ) ;
#835 = CARTESIAN_POINT ( 'NONE',  ( 24.30592326428028827, -5.273034306582022879, -19.67074064463221106 ) ) ;
#837 = ORIENTED_EDGE ( 'NONE', *, *, #25148, .F. ) ;
#836 = CARTESIAN_POINT ( 'NONE',  ( 33.41663030065195272, -12.60673267154789201, -19.71350710734569134 ) ) ;
#838 = DIRECTION ( 'NONE',  ( 0.5877852522924731371, 1.586114251531760728E-16, -0.8090169943749474513 ) ) ;
#839 = FACE_OUTER_BOUND ( 'NONE', #11884, .T. ) ;
#840 = LINE ( 'NONE', #12570, #26282 ) ;
#841 = DIRECTION ( 'NONE',  ( 0.000000000000000000, 0.000000000000000000, 1.000000000000000000 ) ) ;
#842 = VECTOR ( 'NONE', #21103, 1000.000000000000000 ) ;
#843 = LINE ( 'NONE', #28961, #20475 ) ;
#844 = DIRECTION ( 'NONE',  ( 0.000000000000000000, 0.000000000000000000, 1.000000000000000000 ) ) ;
#845 = CARTESIAN_POINT ( 'NONE',  ( 18.21616227284554057, 4.699354889203569918, -13.86658597208997179 ) ) ;
#846 = VERTEX_POINT ( 'NONE', #9130 ) ;
#847 = DIRECTION ( 'NONE',  ( -0.9510565162951536422, -2.566386769018988323E-16, 0.3090169943749475623 ) ) ;
#848 = CARTESIAN_POINT ( 'NONE',  ( 12.27693042220145969, 9.494543488390625896, -15.31068133337694803 ) ) ;
#849 = AXIS2_PLACEMENT_3D ( 'NONE', #1764, #20801, #6484 ) ;
#850 = LINE ( 'NONE', #11826, #24678 ) ;
#851 = DIRECTION ( 'NONE',  ( -0.9510565162951536422, -2.566386769018988323E-16, 0.3090169943749475623 ) ) ;
#852 = ORIENTED_EDGE ( 'NONE', *, *, #16824, .T. ) ;
#853 = CARTESIAN_POINT ( 'NONE',  ( 18.34549112274340033, 0.9605221043122941227, -13.99314825615798341 ) ) ;
#854 = CARTESIAN_POINT ( 'NONE',  ( 18.76228799092704236, 0.4007544294800896578, -19.29634928253052806 ) ) ;
#855 = ORIENTED_EDGE ( 'NONE', *, *, #1035, .F. ) ;
#856 = CARTESIAN_POINT ( 'NONE',  ( 33.54145741815126058, -13.16751478770765793, -19.75123935038191192 ) ) ;
#857 =( NAMED_UNIT ( * ) PLANE_ANGLE_UNIT ( ) SI_UNIT ( $, .RADIAN. ) );
#858 = CARTESIAN_POINT ( 'NONE',  ( 25.72734949418555317, -2.696321649843969936, -17.76569039084671786 ) ) ;
#859 = CARTESIAN_POINT ( 'NONE',  ( 17.76107737582129431, 3.703408080355245158, -15.36634439411934316 ) ) ;
#860 = ADVANCED_FACE ( 'NONE', ( #29558 ), #23186, .T. ) ;
#861 = EDGE_CURVE ( 'NONE', #7930, #18591, #27811, .T. ) ;
#862 = ADVANCED_FACE ( 'NONE', ( #11571 ), #27254, .T. ) ;
#863 = ORIENTED_EDGE ( 'NONE', *, *, #8321, .F. ) ;
#864 = ADVANCED_FACE ( 'NONE', ( #26946 ), #28757, .T. ) ;
#865 = VECTOR ( 'NONE', #21365, 1000.000000000000000 ) ;
#866 = ORIENTED_EDGE ( 'NONE', *, *, #19340, .T. ) ;
#867 = CARTESIAN_POINT ( 'NONE',  ( 175.7287565553229456, -9.999999999999971578, -33.50000000000000000 ) ) ;
#868 = ORIENTED_EDGE ( 'NONE', *, *, #10306, .T. ) ;
#869 = SURFACE_SIDE_STYLE ('',( #21768 ) ) ;
#870 = VECTOR ( 'NONE', #18675, 1000.000000000000000 ) ;
#871 = CYLINDRICAL_SURFACE ( 'NONE', #19866, 2.500000000000000888 ) ;
#872 = PLANE ( 'NONE',  #23612 ) ;
#873 = DIRECTION ( 'NONE',  ( 0.000000000000000000, 0.000000000000000000, 1.000000000000000000 ) ) ;
#874 = CARTESIAN_POINT ( 'NONE',  ( 33.36027191889437660, -10.38700102556154903, -18.15738432823107473 ) ) ;
#875 = CIRCLE ( 'NONE', #26731, 0.4999999999999998335 ) ;
#876 = CARTESIAN_POINT ( 'NONE',  ( 9.905109554012803130, 16.45925992188944420, -16.51025697316969953 ) ) ;
#877 = DIRECTION ( 'NONE',  ( 0.5877852522924731371, 0.000000000000000000, 0.8090169943749474513 ) ) ;
#878 = DIRECTION ( 'NONE',  ( 0.000000000000000000, 0.000000000000000000, 1.000000000000000000 ) ) ;
#879 = CARTESIAN_POINT ( 'NONE',  ( 12.02558468657594659, 9.327346335875439820, -16.69235103436730938 ) ) ;
#880 = FACE_OUTER_BOUND ( 'NONE', #27488, .T. ) ;
#881 = DIRECTION ( 'NONE',  ( 0.3090169943749472292, 8.338696094057992503E-17, -0.9510565162951536422 ) ) ;
#882 = EDGE_LOOP ( 'NONE', ( #8366, #4789, #29727, #9280 ) ) ;
#883 = CARTESIAN_POINT ( 'NONE',  ( -24.99999999999999289, 60.00000000000000711, -30.00000000000000711 ) ) ;
#884 = CARTESIAN_POINT ( 'NONE',  ( 153.6922820468854525, -4.999999999999976907, -35.24709285013155835 ) ) ;
#885 = CIRCLE ( 'NONE', #17917, 4.250000000000000000 ) ;
#886 = DIRECTION ( 'NONE',  ( -2.698458740408365879E-16, 1.000000000000000000, 0.000000000000000000 ) ) ;
#887 = VERTEX_POINT ( 'NONE', #29093 ) ;
#888 = VERTEX_POINT ( 'NONE', #12859 ) ;
#889 = CARTESIAN_POINT ( 'NONE',  ( 13.34629304935920757, 7.611730149031187054, -15.73439023580873730 ) ) ;
#890 = VECTOR ( 'NONE', #25219, 1000.000000000000000 ) ;
#891 = CARTESIAN_POINT ( 'NONE',  ( 14.42366234001531922, 7.375548675892134476, -20.85295579936483179 ) ) ;
#892 = EDGE_CURVE ( 'NONE', #29509, #10549, #17732, .T. ) ;
#893 = CARTESIAN_POINT ( 'NONE',  ( 19.95076809599375878, -1.008983920988137495, -18.52968236344498720 ) ) ;
#894 = CARTESIAN_POINT ( 'NONE',  ( 161.1922820468853672, -4.999999999999974243, -22.25671179336496053 ) ) ;
#895 = LINE ( 'NONE', #15056, #12119 ) ;
#896 = DIRECTION ( 'NONE',  ( -2.698458740408365879E-16, 1.000000000000000000, 0.000000000000000000 ) ) ;
#897 = EDGE_CURVE ( 'NONE', #28202, #19572, #20324, .T. ) ;
#898 = DIRECTION ( 'NONE',  ( -0.9510565162951536422, 0.000000000000000000, -0.3090169943749472292 ) ) ;
#899 = DIRECTION ( 'NONE',  ( -0.8090169943749474513, -2.183098979609982436E-16, 0.5877852522924731371 ) ) ;
#900 = LINE ( 'NONE', #27023, #12161 ) ;
#901 = CIRCLE ( 'NONE', #17942, 3.000000000000002665 ) ;
#902 = FACE_OUTER_BOUND ( 'NONE', #26467, .T. ) ;
#903 = DIRECTION ( 'NONE',  ( -0.9510565162951536422, -2.566386769018988323E-16, 0.3090169943749475623 ) ) ;
#904 = CARTESIAN_POINT ( 'NONE',  ( 11.70392491148546732, 10.80251906652491556, -16.82536866641744311 ) ) ;
#905 = CARTESIAN_POINT ( 'NONE',  ( 35.32886446602115171, -21.19738783794349857, -20.03221113960638178 ) ) ;
#906 = CIRCLE ( 'NONE', #8193, 4.000000000000003553 ) ;
#907 = ORIENTED_EDGE ( 'NONE', *, *, #8004, .T. ) ;
#908 = CARTESIAN_POINT ( 'NONE',  ( 9.274674406624409784, 15.43775921338471413, -16.98767239532306661 ) ) ;
#909 = CARTESIAN_POINT ( 'NONE',  ( 21.18945582756405344, -5.194394521544061227, -16.21196392551894405 ) ) ;
#910 = CARTESIAN_POINT ( 'NONE',  ( 12.86796368952119174, 9.515911916162036022, -16.11566496612908139 ) ) ;
#911 = FACE_BOUND ( 'NONE', #4279, .T. ) ;
#912 = VECTOR ( 'NONE', #20314, 1000.000000000000000 ) ;
#913 = EDGE_CURVE ( 'NONE', #9720, #12877, #3381, .T. ) ;
#914 = VECTOR ( 'NONE', #25269, 1000.000000000000000 ) ;
#915 = ORIENTED_EDGE ( 'NONE', *, *, #8153, .T. ) ;
#916 = CARTESIAN_POINT ( 'NONE',  ( 162.0152310637604671, -1.999999999999973133, -6.958068083716895558 ) ) ;
#917 = CARTESIAN_POINT ( 'NONE',  ( 11.45661370752365116, 9.343864103108954211, -15.86763743611193789 ) ) ;
#918 = LINE ( 'NONE', #1085, #25237 ) ;
#919 = ORIENTED_EDGE ( 'NONE', *, *, #21721, .F. ) ;
#920 = ORIENTED_EDGE ( 'NONE', *, *, #6229, .F. ) ;
#921 = DIRECTION ( 'NONE',  ( 0.9510565162951535312, 2.566386769018988816E-16, -0.3090169943749475623 ) ) ;
#922 = ORIENTED_EDGE ( 'NONE', *, *, #22458, .F. ) ;
#923 = CARTESIAN_POINT ( 'NONE',  ( 12.67163634847678644, 8.538173360731750705, -16.25940050138558135 ) ) ;
#924 = EDGE_LOOP ( 'NONE', ( #4638, #12101, #16492, #28325 ) ) ;
#925 = CARTESIAN_POINT ( 'NONE',  ( 36.54859390953723874, -23.18451583373416014, -14.99999999999999822 ) ) ;
#926 = CARTESIAN_POINT ( 'NONE',  ( 22.35254782987788147, 5.884919045556002537, -15.62344653218675283 ) ) ;
#927 = CARTESIAN_POINT ( 'NONE',  ( 13.40325769311605164, 6.909072298322937122, -18.40730773563142719 ) ) ;
#928 = EDGE_LOOP ( 'NONE', ( #6024, #1799, #821, #18334 ) ) ;
#929 = VERTEX_POINT ( 'NONE', #8132 ) ;
#930 = VERTEX_POINT ( 'NONE', #27092 ) ;
#931 =( REPRESENTATION_RELATIONSHIP ('NONE','NONE', #5250, #22819 ) REPRESENTATION_RELATIONSHIP_WITH_TRANSFORMATION ( #7496 )SHAPE_REPRESENTATION_RELATIONSHIP( ) );
#932 = DIRECTION ( 'NONE',  ( -1.000000000000000000, -2.698458740408365879E-16, -0.000000000000000000 ) ) ;
#933 = ORIENTED_EDGE ( 'NONE', *, *, #13523, .T. ) ;
#934 = ADVANCED_FACE ( 'NONE', ( #1735 ), #10868, .T. ) ;
#935 = CARTESIAN_POINT ( 'NONE',  ( 116.9310667037121618, -4.999999999999985789, -84.95539280527852100 ) ) ;
#936 = SHAPE_DEFINITION_REPRESENTATION ( #13498, #29092 ) ;
#937 = B_SPLINE_CURVE_WITH_KNOTS ( 'NONE', 3,
 ( #12217, #16653, #16799, #14042, #25971, #23835, #3091, #9467, #19090, #18790, #19231, #11762, #12361, #23371, #21080, #2781, #7645, #14198, #9921, #2488, #23526, #26128, #5207, #16949, #7203, #14498, #21672, #773, #338, #10070, #4901, #19384, #5052, #7051, #16340, #21223, #9623, #18944, #14342, #23677, #28297, #21832, #13117, #24429, #12817, #29046, #10826, #1235, #22130, #8082, #3826, #19679, #28904, #28749, #6107, #19534, #29196, #3524, #17392, #8232, #15096, #1095, #24735, #7936, #26736, #5809, #17250, #12967, #29361, #24582, #17544, #10524, #19992, #26578, #3231, #10681, #5662, #10373 ),
 .UNSPECIFIED., .F., .F.,
 ( 4, 2, 2, 2, 2, 2, 2, 2, 2, 2, 2, 2, 2, 2, 2, 2, 2, 2, 2, 2, 2, 2, 2, 2, 2, 2, 2, 2, 2, 2, 2, 2, 2, 2, 2, 2, 2, 2, 4 ),
 ( 0.04625696548573639266, 0.1003381136405422785, 0.1505071704608134109, 0.1755916988709489979, 0.1881339630760167636, 0.1944050951785506465, 0.2006762272810845293, 0.2086934065084689038, 0.2167105857358532783, 0.2327449441906219718, 0.2648136611001593588, 0.2968823780096967457, 0.3129167364644654947, 0.3209339156918498137, 0.3289510949192341327, 0.3346579968240730452, 0.3403648987289118466, 0.3517787025385894495, 0.3746063101579446553, 0.4202615253966550668, 0.5115719558740758899, 0.6028823863514967130, 0.6485376015902071245, 0.6713652092095623303, 0.6827790130192399332, 0.6941928168289175360, 0.7036545619149295883, 0.7131163070009416405, 0.7320397971729657449, 0.7698867775170139538, 0.8077337578610621627, 0.8266572480330862671, 0.8361189931190984304, 0.8455807382051104826, 0.8552319420672911399, 0.8648831459294716861, 0.8841855536538327787, 0.9227903691025551858, 1.000000000000000000 ),
 .UNSPECIFIED. ) ;
#938 = CARTESIAN_POINT ( 'NONE',  ( 18.22321846687148650, 1.664438589611230812, -15.57940112478783945 ) ) ;
#939 = VECTOR ( 'NONE', #6224, 1000.000000000000000 ) ;
#940 = CARTESIAN_POINT ( 'NONE',  ( 19.91209246711783010, 5.411768277715644615, -14.29674560697521457 ) ) ;
#941 = PRESENTATION_LAYER_ASSIGNMENT (  '', '', ( #23841 ) ) ;
#942 = DIRECTION ( 'NONE',  ( 1.000000000000000000, 4.440892098500622217E-16, 0.000000000000000000 ) ) ;
#943 = FACE_BOUND ( 'NONE', #7642, .T. ) ;
#944 = LINE ( 'NONE', #28304, #14996 ) ;
#945 = DIRECTION ( 'NONE',  ( 0.000000000000000000, 0.000000000000000000, -1.000000000000000000 ) ) ;
#946 = DIRECTION ( 'NONE',  ( 0.000000000000000000, -0.000000000000000000, 1.000000000000000000 ) ) ;
#947 = DIRECTION ( 'NONE',  ( -0.8090169943749474513, -2.183098979609982436E-16, 0.5877852522924731371 ) ) ;
#948 = CARTESIAN_POINT ( 'NONE',  ( 12.25159070717542065, 9.517778977577904698, -15.32825133053543887 ) ) ;
#949 = CARTESIAN_POINT ( 'NONE',  ( -6.686525924292797463, 5.377136764700167326, -0.3167204509598451900 ) ) ;
#950 = EDGE_CURVE ( 'NONE', #2754, #23037, #3716, .T. ) ;
#951 = EDGE_CURVE ( 'NONE', #20254, #12966, #17007, .T. ) ;
#952 = VERTEX_POINT ( 'NONE', #1434 ) ;
#953 = VECTOR ( 'NONE', #9784, 999.9999999999998863 ) ;
#954 = DIRECTION ( 'NONE',  ( 0.5877852522924731371, 1.586114251531760728E-16, -0.8090169943749474513 ) ) ;
#955 = ORIENTED_EDGE ( 'NONE', *, *, #19484, .F. ) ;
#956 = CARTESIAN_POINT ( 'NONE',  ( 12.49977518293622758, 8.570603418560722275, -15.13035415120363325 ) ) ;
#957 = EDGE_CURVE ( 'NONE', #10350, #9967, #5858, .T. ) ;
#958 = ORIENTED_EDGE ( 'NONE', *, *, #11692, .F. ) ;
#959 = CARTESIAN_POINT ( 'NONE',  ( 10.58765414998594245, 9.416266744339480965, -16.44470908465386572 ) ) ;
#960 = LINE ( 'NONE', #16817, #5391 ) ;
#961 = FACE_OUTER_BOUND ( 'NONE', #9465, .T. ) ;
#962 = LINE ( 'NONE', #19256, #20960 ) ;
#963 = AXIS2_PLACEMENT_3D ( 'NONE', #19317, #1029, #19468 ) ;
#964 = ORIENTED_EDGE ( 'NONE', *, *, #15893, .F. ) ;
#965 = CARTESIAN_POINT ( 'NONE',  ( 130.7287565553229456, -4.999999999999983125, -13.44584919360585928 ) ) ;
#966 = VERTEX_POINT ( 'NONE', #15601 ) ;
#967 = CARTESIAN_POINT ( 'NONE',  ( 12.81602886594196988, 9.615025227323064527, -16.14774825664093783 ) ) ;
#968 = VERTEX_POINT ( 'NONE', #15141 ) ;
#969 = CARTESIAN_POINT ( 'NONE',  ( 33.33106278064285277, -11.02967194543584029, -16.07471553095689742 ) ) ;
#970 = CARTESIAN_POINT ( 'NONE',  ( 21.19279910686179846, 4.720633506281588510, -19.26595127233560234 ) ) ;
#971 = ORIENTED_EDGE ( 'NONE', *, *, #28242, .T. ) ;
#972 = LINE ( 'NONE', #10255, #5266 ) ;
#973 = CARTESIAN_POINT ( 'NONE',  ( 18.51594006248351931, 7.284897756227690202, -14.24483590514913089 ) ) ;
#974 = CARTESIAN_POINT ( 'NONE',  ( 0.000000000000000000, 0.000000000000000000, 1.700000000000000178 ) ) ;
#975 = CARTESIAN_POINT ( 'NONE',  ( 168.6922820468853104, -9.999999999999998224, -9.266330736598359152 ) ) ;
#976 =( NAMED_UNIT ( * ) SI_UNIT ( $, .STERADIAN. ) SOLID_ANGLE_UNIT ( ) );
#977 = EDGE_CURVE ( 'NONE', #15701, #26572, #20177, .T. ) ;
#978 = CARTESIAN_POINT ( 'NONE',  ( 21.30888034401541731, -0.8953576338359930942, -14.03585182699830369 ) ) ;
#979 = MANIFOLD_SOLID_BREP ( 'BaseBody', #6798 ) ;
#980 = CARTESIAN_POINT ( 'NONE',  ( 23.16309603597909472, 3.730466837354933674, -16.34659541137592598 ) ) ;
#981 = VERTEX_POINT ( 'NONE', #7016 ) ;
#982 = ORIENTED_EDGE ( 'NONE', *, *, #22137, .F. ) ;
#983 = VERTEX_POINT ( 'NONE', #25625 ) ;
#984 = DIRECTION ( 'NONE',  ( 0.000000000000000000, 0.000000000000000000, 1.000000000000000000 ) ) ;
#985 = AXIS2_PLACEMENT_3D ( 'NONE', #22908, #27222, #11143 ) ;
#986 = AXIS2_PLACEMENT_3D ( 'NONE', #29053, #17398, #15258 ) ;
#987 = DIRECTION ( 'NONE',  ( -0.9510565162951536422, -2.566386769018988816E-16, -0.3090169943749472292 ) ) ;
#988 = AXIS2_PLACEMENT_3D ( 'NONE', #21614, #17036, #3172 ) ;
#989 = CARTESIAN_POINT ( 'NONE',  ( 3.319543390096043378, -7.321065037175453760, -0.01688885742778342344 ) ) ;
#990 = DIRECTION ( 'NONE',  ( -2.698458740408365879E-16, 1.000000000000000000, 0.000000000000000000 ) ) ;
#991 = LINE ( 'NONE', #3138, #6095 ) ;
#992 = CARTESIAN_POINT ( 'NONE',  ( 11.47464782381437587, 9.261287281732329291, -15.86016978468419936 ) ) ;
#993 = CARTESIAN_POINT ( 'NONE',  ( 27.10702390817755614, -8.414881854042032927, -18.30456363717458146 ) ) ;
#994 = CARTESIAN_POINT ( 'NONE',  ( 27.50962693642323131, -9.092369620780022643, -12.61635453147917474 ) ) ;
#995 = EDGE_CURVE ( 'NONE', #29111, #15160, #24932, .T. ) ;
#996 = VECTOR ( 'NONE', #1452, 1000.000000000000000 ) ;
#998 = ORIENTED_EDGE ( 'NONE', *, *, #19067, .T. ) ;
#997 = CARTESIAN_POINT ( 'NONE',  ( 32.00110207675911767, -10.95298233446834502, -16.54939777171900417 ) ) ;
#999 = DIRECTION ( 'NONE',  ( 0.000000000000000000, 0.000000000000000000, 1.000000000000000000 ) ) ;
#1000 = CARTESIAN_POINT ( 'NONE',  ( 91.73376360168730059, -4.999999999999992006, 66.64848051061605361 ) ) ;
#1001 = DIRECTION ( 'NONE',  ( 0.5877852522924731371, 1.586114251531760728E-16, -0.8090169943749474513 ) ) ;
#1002 = VECTOR ( 'NONE', #17125, 1000.000000000000000 ) ;
#1003 = DIRECTION ( 'NONE',  ( 1.000000000000000000, 2.698458740408365879E-16, -1.110223024625156540E-16 ) ) ;
#1004 = EDGE_CURVE ( 'NONE', #7228, #23153, #12618, .T. ) ;
#1005 = DIRECTION ( 'NONE',  ( -2.698458740408365879E-16, 1.000000000000000000, 0.000000000000000000 ) ) ;
#1006 = CARTESIAN_POINT ( 'NONE',  ( 169.5152310637604671, -9.999999999999996447, -11.28819510263909542 ) ) ;
#1007 = ADVANCED_FACE ( 'NONE', ( #23338 ), #28556, .T. ) ;
#1008 = CARTESIAN_POINT ( 'NONE',  ( 16.89369580670022941, 0.5033910033923695293, -17.32063897790030893 ) ) ;
#1009 = ORIENTED_EDGE ( 'NONE', *, *, #19272, .F. ) ;
#1010 = LINE ( 'NONE', #28820, #28606 ) ;
#1011 = CARTESIAN_POINT ( 'NONE',  ( 12.24452513275510235, 9.643158527868859409, -15.32408204131529317 ) ) ;
#1012 = VECTOR ( 'NONE', #14521, 1000.000000000000000 ) ;
#1013 = LINE ( 'NONE', #17759, #10031 ) ;
#1014 = CARTESIAN_POINT ( 'NONE',  ( 146.1922820468853956, -1.999999999999978018, -4.936203717676158398 ) ) ;
#1015 = VECTOR ( 'NONE', #8319, 1000.000000000000000 ) ;
#1016 = CARTESIAN_POINT ( 'NONE',  ( 19.61192361542596529, -2.405681417800469291, -14.70675912396028906 ) ) ;
#1017 = LINE ( 'NONE', #22058, #24247 ) ;
#1018 = CARTESIAN_POINT ( 'NONE',  ( 18.97422388862426601, -0.1098198481195374748, -14.77765307979439058 ) ) ;
#1019 = ORIENTED_EDGE ( 'NONE', *, *, #21791, .T. ) ;
#1020 = CARTESIAN_POINT ( 'NONE',  ( 35.49237112349044310, -21.93193663806729887, -19.32748734164077931 ) ) ;
#1021 =( NAMED_UNIT ( * ) PLANE_ANGLE_UNIT ( ) SI_UNIT ( $, .RADIAN. ) );
#1022 = CARTESIAN_POINT ( 'NONE',  ( 30.37590262355644910, -7.260401249342992358, -13.74898149931492775 ) ) ;
#1023 = CARTESIAN_POINT ( 'NONE',  ( 24.20684193479931068, 1.026663266619176840, -14.52337054612115708 ) ) ;
#1024 = AXIS2_PLACEMENT_3D ( 'NONE', #17499, #29628, #18407 ) ;
#1025 = CARTESIAN_POINT ( 'NONE',  ( 28.47856004806874353, -11.16640101040803401, -12.66155532224275149 ) ) ;
#1026 = VECTOR ( 'NONE', #2101, 1000.000000000000000 ) ;
#1027 = PLANE ( 'NONE',  #29947 ) ;
#1028 = ORIENTED_EDGE ( 'NONE', *, *, #20544, .T. ) ;
#1029 = DIRECTION ( 'NONE',  ( 0.3090169943749475623, 8.338696094058001131E-17, 0.9510565162951536422 ) ) ;
#1030 = PLANE ( 'NONE',  #3315 ) ;
#1031 = DIRECTION ( 'NONE',  ( -0.9510565162951536422, 0.000000000000000000, -0.3090169943749472292 ) ) ;
#1032 = CARTESIAN_POINT ( 'NONE',  ( 137.0152310637605808, -1.999999999999979572, -8.721423840594312082 ) ) ;
#1033 = CARTESIAN_POINT ( 'NONE',  ( 34.06228043176686526, -11.34293828116054037, -19.64761387034043949 ) ) ;
#1034 = CARTESIAN_POINT ( 'NONE',  ( 11.21346931060482000, 10.45895530107994098, -15.96818619734747458 ) ) ;
#1035 = EDGE_CURVE ( 'NONE', #19382, #17985, #28108, .T. ) ;
#1036 = CARTESIAN_POINT ( 'NONE',  ( 175.7287565553229456, -4.999999999999970690, -13.44584919360591257 ) ) ;
#1037 = DIRECTION ( 'NONE',  ( 0.000000000000000000, 0.000000000000000000, 1.000000000000000000 ) ) ;
#1038 = ADVANCED_FACE ( 'NONE', ( #7466, #11728, #5018 ), #7170, .F. ) ;
#1039 = EDGE_CURVE ( 'NONE', #12109, #19638, #23490, .T. ) ;
#1040 = CARTESIAN_POINT ( 'NONE',  ( 11.98759337455738816, 9.501579335558542283, -16.70806177831036976 ) ) ;
#1041 = DIRECTION ( 'NONE',  ( 1.000000000000000000, 4.440892098500622217E-16, 0.000000000000000000 ) ) ;
#1042 = EDGE_CURVE ( 'NONE', #18885, #9954, #9589, .T. ) ;
#1043 = CARTESIAN_POINT ( 'NONE',  ( 175.7287565553229456, -4.999999999999970690, 3.500000000000003109 ) ) ;
#1044 = VECTOR ( 'NONE', #19933, 999.9999999999998863 ) ;
#1045 = EDGE_LOOP ( 'NONE', ( #15324, #2019, #2265, #5446 ) ) ;
#1046 = AXIS2_PLACEMENT_3D ( 'NONE', #21210, #26849, #5919 ) ;
#1047 = DIRECTION ( 'NONE',  ( 0.000000000000000000, 0.000000000000000000, 1.000000000000000000 ) ) ;
#1048 = DIRECTION ( 'NONE',  ( -0.8090169943749474513, -2.183098979609982436E-16, 0.5877852522924731371 ) ) ;
#1049 = CARTESIAN_POINT ( 'NONE',  ( 15.37415192284491638, -5.000000000000013323, 47.31677427097104527 ) ) ;
#1050 = ORIENTED_EDGE ( 'NONE', *, *, #15240, .T. ) ;
#1051 = ORIENTED_EDGE ( 'NONE', *, *, #13820, .T. ) ;
#1052 = CARTESIAN_POINT ( 'NONE',  ( 13.10901043280714084, 7.538357286119017786, -15.92110722978107873 ) ) ;
#1053 = VERTEX_POINT ( 'NONE', #14614 ) ;
#1054 = PRESENTATION_LAYER_ASSIGNMENT (  '', '', ( #1531 ) ) ;
#1055 = CARTESIAN_POINT ( 'NONE',  ( 15.78898853071975061, 11.08777142890889245, -14.37707943039971781 ) ) ;
#1056 = CARTESIAN_POINT ( 'NONE',  ( 26.53548354394225228, -12.81408696708834860, -17.07385457597708367 ) ) ;
#1057 = DIRECTION ( 'NONE',  ( 1.000000000000000000, 4.440892098500622217E-16, 0.000000000000000000 ) ) ;
#1058 = CARTESIAN_POINT ( 'NONE',  ( 136.1922820468854241, -1.999999999999980460, -13.59645775552055547 ) ) ;
#1059 = LINE ( 'NONE', #26702, #13282 ) ;
#1060 = ORIENTED_EDGE ( 'NONE', *, *, #27134, .T. ) ;
#1061 = DIRECTION ( 'NONE',  ( -2.698458740408365879E-16, 1.000000000000000000, 0.000000000000000000 ) ) ;
#1062 = AXIS2_PLACEMENT_3D ( 'NONE', #26492, #7854, #7556 ) ;
#1063 = CARTESIAN_POINT ( 'NONE',  ( 157.2287565553229456, -1.999999999999974021, -12.16987298107780369 ) ) ;
#1065 = VERTEX_POINT ( 'NONE', #9889 ) ;
#1064 = DIRECTION ( 'NONE',  ( 0.000000000000000000, 0.000000000000000000, 1.000000000000000000 ) ) ;
#1066 = VECTOR ( 'NONE', #30185, 1000.000000000000114 ) ;
#1067 = CARTESIAN_POINT ( 'NONE',  ( 172.7287565553229456, -9.999999999999971578, 3.500000000000003109 ) ) ;
#1068 = CARTESIAN_POINT ( 'NONE',  ( 142.0152310637605524, -10.00000000000000355, -8.721423840594312082 ) ) ;
#1069 = CARTESIAN_POINT ( 'NONE',  ( 12.67163634847678644, 8.538173360731750705, -16.25940050138558135 ) ) ;
#1070 = EDGE_LOOP ( 'NONE', ( #27500, #26319, #424, #13784 ) ) ;
#1071 = CARTESIAN_POINT ( 'NONE',  ( 33.63121621376239290, -12.57075016180469262, -18.73605167971255980 ) ) ;
#1072 = ORIENTED_EDGE ( 'NONE', *, *, #2270, .F. ) ;
#1073 = CARTESIAN_POINT ( 'NONE',  ( 9.106918858820071350, 16.20710753947419747, -17.05743340929950946 ) ) ;
#1074 = PRODUCT ( 'Ergonomic Serrated Toe Peg', 'Ergonomic Serrated Toe Peg', '', ( #14944 ) ) ;
#1075 = EDGE_CURVE ( 'NONE', #18592, #20355, #19201, .T. ) ;
#1076 = CARTESIAN_POINT ( 'NONE',  ( 26.72358035960067824, -3.685970424986596772, -17.59444040205794835 ) ) ;
#1077 = ADVANCED_FACE ( 'NONE', ( #25938 ), #14310, .T. ) ;
#1078 = CARTESIAN_POINT ( 'NONE',  ( 12.83223741744420288, 9.540690758033102625, -16.14104544935691976 ) ) ;
#1079 = FACE_BOUND ( 'NONE', #21974, .T. ) ;
#1080 = EDGE_CURVE ( 'NONE', #23153, #15583, #23963, .T. ) ;
#1081 = VERTEX_POINT ( 'NONE', #21346 ) ;
#1082 = EDGE_LOOP ( 'NONE', ( #14610, #10358, #28180, #8654 ) ) ;
#1083 = DIRECTION ( 'NONE',  ( -0.000000000000000000, -0.000000000000000000, -1.000000000000000000 ) ) ;
#1084 = CARTESIAN_POINT ( 'NONE',  ( 12.48484057295006977, 8.564241722236854315, -15.14223913367768759 ) ) ;
#1085 = CARTESIAN_POINT ( 'NONE',  ( 18.47091782295028395, -5.000000000000012434, -56.84763970021110424 ) ) ;
#1086 = ORIENTED_EDGE ( 'NONE', *, *, #25834, .F. ) ;
#1087 = CARTESIAN_POINT ( 'NONE',  ( 161.1922820468853956, -9.999999999999998224, -28.06379628232387802 ) ) ;
#1088 = VERTEX_POINT ( 'NONE', #16914 ) ;
#1089 = CARTESIAN_POINT ( 'NONE',  ( 12.02685106364323531, 9.321538569219327997, -16.69182734290254899 ) ) ;
#1090 = ORIENTED_EDGE ( 'NONE', *, *, #23380, .T. ) ;
#1091 = CARTESIAN_POINT ( 'NONE',  ( 13.93547621865856634, 6.828337171336619882, -15.16703734247451507 ) ) ;
#1092 = CARTESIAN_POINT ( 'NONE',  ( 26.48263329513011755, -12.06126822337667903, -13.95730679897583038 ) ) ;
#1093 = DIRECTION ( 'NONE',  ( 1.000000000000000000, 1.226925503391459091E-16, -0.000000000000000000 ) ) ;
#1094 = ORIENTED_EDGE ( 'NONE', *, *, #17074, .F. ) ;
#1095 = CARTESIAN_POINT ( 'NONE',  ( 36.52322468491136220, -22.07054534594105988, -19.04503427665075321 ) ) ;
#1096 = APPLICATION_PROTOCOL_DEFINITION ( 'draft international standard', 'automotive_design', 1998, #18251 ) ;
#1097 = ORIENTED_EDGE ( 'NONE', *, *, #3574, .T. ) ;
#1098 = CARTESIAN_POINT ( 'NONE',  ( 19.48014203372339992, 3.175912578606837844, -18.88683143354647243 ) ) ;
#1099 = CARTESIAN_POINT ( 'NONE',  ( 20.23291344124205793, 5.521974472852556381, -14.51730806008046137 ) ) ;
#1100 = AXIS2_PLACEMENT_3D ( 'NONE', #1586, #6152, #22173 ) ;
#1101 = CARTESIAN_POINT ( 'NONE',  ( 168.6922820468853956, -9.999999999999996447, -35.24709285013155835 ) ) ;
#1102 = FACE_BOUND ( 'NONE', #26455, .T. ) ;
#1103 = VECTOR ( 'NONE', #29704, 1000.000000000000000 ) ;
#1104 = LINE ( 'NONE', #24437, #1621 ) ;
#1105 = CARTESIAN_POINT ( 'NONE',  ( 132.0152310637605524, -1.999999999999981348, -0.06116980274991495881 ) ) ;
#1106 = CARTESIAN_POINT ( 'NONE',  ( 153.6922820468853672, -10.00000000000000178, -6.413161187712876909 ) ) ;
#1107 = LINE ( 'NONE', #19843, #27108 ) ;
#1108 = CARTESIAN_POINT ( 'NONE',  ( 12.27009251048667160, 9.509012028593735621, -15.31479730457434307 ) ) ;
#1109 = EDGE_CURVE ( 'NONE', #15010, #3555, #29256, .T. ) ;
#1110 = CARTESIAN_POINT ( 'NONE',  ( 157.0152310637604671, -10.00000000000000000, 1.702185954127501066 ) ) ;
#1111 = CARTESIAN_POINT ( 'NONE',  ( 148.6922820468854525, -10.00000000000000178, -32.39392330124607611 ) ) ;
#1112 = EDGE_LOOP ( 'NONE', ( #26693, #23174, #25311, #28389 ) ) ;
#1113 = CARTESIAN_POINT ( 'NONE',  ( 12.49860086554322436, 8.570087612320898884, -15.13128986298120537 ) ) ;
#1114 = VERTEX_POINT ( 'NONE', #16770 ) ;
#1115 = VECTOR ( 'NONE', #2153, 1000.000000000000000 ) ;
#1116 = CARTESIAN_POINT ( 'NONE',  ( 10.90022735844294388, 8.411956631741958290, -16.28271526948893921 ) ) ;
#1117 = DIRECTION ( 'NONE',  ( 1.000000000000000000, 0.000000000000000000, 0.000000000000000000 ) ) ;
#1118 =( NAMED_UNIT ( * ) PLANE_ANGLE_UNIT ( ) SI_UNIT ( $, .RADIAN. ) );
#1119 = DIRECTION ( 'NONE',  ( 0.000000000000000000, 0.000000000000000000, 1.000000000000000000 ) ) ;
#1120 = EDGE_LOOP ( 'NONE', ( #11525, #6792, #20761, #8444 ) ) ;
#1121 = CARTESIAN_POINT ( 'NONE',  ( 2.500000000000000444, 2.357898499370430834, -3.469446951953614189E-15 ) ) ;
#1122 = ORIENTED_EDGE ( 'NONE', *, *, #9629, .T. ) ;
#1123 = CARTESIAN_POINT ( 'NONE',  ( 11.60030688134799171, 15.19048121717941768, -16.65049206281727479 ) ) ;
#1124 = CARTESIAN_POINT ( 'NONE',  ( 33.69236230569678980, -11.08454582564024449, -17.09586691508924972 ) ) ;
#1125 = CARTESIAN_POINT ( 'NONE',  ( 19.23836061553175369, 5.151828676608854352, -13.99136221198299168 ) ) ;
#1126 = CARTESIAN_POINT ( 'NONE',  ( 163.6922820468853956, -4.999999999999973355, -35.24709285013155835 ) ) ;
#1127 = VECTOR ( 'NONE', #896, 1000.000000000000000 ) ;
#1128 = CARTESIAN_POINT ( 'NONE',  ( 16.36264732604271899, 7.873549196589271659, -20.78255227469630739 ) ) ;
#1129 = DIRECTION ( 'NONE',  ( 1.000000000000000000, 4.440892098500622217E-16, 0.000000000000000000 ) ) ;
#1130 = DIRECTION ( 'NONE',  ( -2.698458740408365879E-16, 1.000000000000000000, 0.000000000000000000 ) ) ;
#1131 = CARTESIAN_POINT ( 'NONE',  ( 26.39122182234759961, -2.132411660323914049, -15.07701415690354274 ) ) ;
#1132 = CARTESIAN_POINT ( 'NONE',  ( 20.97462796522363959, -1.010871063906457534, -12.65628865346789134 ) ) ;
#1133 = ORIENTED_EDGE ( 'NONE', *, *, #2497, .F. ) ;
#1134 = ADVANCED_FACE ( 'NONE', ( #23801 ), #21499, .T. ) ;
#1135 = EDGE_CURVE ( 'NONE', #14797, #15637, #8052, .T. ) ;
#1136 = CARTESIAN_POINT ( 'NONE',  ( 161.1922820468853672, -9.999999999999998224, -19.40354224447947828 ) ) ;
#1137 = DIRECTION ( 'NONE',  ( 1.000000000000000000, 2.698458740408365879E-16, 0.000000000000000000 ) ) ;
#1138 = CARTESIAN_POINT ( 'NONE',  ( -4.000000000000008882, 6.928203230275508773, -5.000000000000000888 ) ) ;
#1139 = LINE ( 'NONE', #10420, #27314 ) ;
#1140 = DIRECTION ( 'NONE',  ( 0.000000000000000000, 0.000000000000000000, 1.000000000000000000 ) ) ;
#1141 = AXIS2_PLACEMENT_3D ( 'NONE', #20849, #9242, #6980 ) ;
#1142 = CARTESIAN_POINT ( 'NONE',  ( 11.47257016429183452, 9.270685755423764718, -15.86103888016343255 ) ) ;
#1143 = CARTESIAN_POINT ( 'NONE',  ( 16.53304876882650731, 8.555045913257369961, -19.77053526944897754 ) ) ;
#1144 = CARTESIAN_POINT ( 'NONE',  ( 22.75855789899217640, -7.280205122891536540, -14.30210469086359915 ) ) ;
#1145 = ORIENTED_EDGE ( 'NONE', *, *, #2863, .T. ) ;
#1146 = CARTESIAN_POINT ( 'NONE',  ( 125.7287565553229456, -4.000000000000003553, 0.5000000000000143219 ) ) ;
#1147 = CARTESIAN_POINT ( 'NONE',  ( 133.6922820468854241, -10.00000000000000711, -0.6060766987539614181 ) ) ;
#1148 = LINE ( 'NONE', #3294, #1929 ) ;
#1149 = DIRECTION ( 'NONE',  ( -2.698458740408365879E-16, 1.000000000000000000, 0.000000000000000000 ) ) ;
#1150 = CARTESIAN_POINT ( 'NONE',  ( 175.7287565553229456, -9.999999999999994671, -28.21440484423853690 ) ) ;
#1151 = CARTESIAN_POINT ( 'NONE',  ( 174.7287565553228319, -1.999999999999970024, 0.8205080756887930260 ) ) ;
#1153 = ORIENTED_EDGE ( 'NONE', *, *, #17753, .F. ) ;
#1152 = CARTESIAN_POINT ( 'NONE',  ( 20.99533150354982070, 4.487273811465053441, -19.54336078777620500 ) ) ;
#1154 = ORIENTED_EDGE ( 'NONE', *, *, #23808, .T. ) ;
#1155 = CARTESIAN_POINT ( 'NONE',  ( 139.5152310637606092, -1.999999999999978684, -28.60870317832789311 ) ) ;
#1156 = CARTESIAN_POINT ( 'NONE',  ( 12.27630411038995106, 9.497004473356668086, -15.31097170929839812 ) ) ;
#1157 = CARTESIAN_POINT ( 'NONE',  ( 32.57315965809380742, -11.03986597812349935, -18.16622079659612510 ) ) ;
#1158 = CARTESIAN_POINT ( 'NONE',  ( 132.0152310637605524, -1.999999999999981348, -34.70218595412750773 ) ) ;
#1159 = CARTESIAN_POINT ( 'NONE',  ( 17.72480397827495224, 1.356124466512965476, -19.40231245121514903 ) ) ;
#1160 = LINE ( 'NONE', #1616, #29159 ) ;
#1161 = CARTESIAN_POINT ( 'NONE',  ( 20.68391251823057075, 0.6588762160484964436, -13.99488169736409304 ) ) ;
#1162 = ORIENTED_EDGE ( 'NONE', *, *, #30234, .F. ) ;
#1163 = CARTESIAN_POINT ( 'NONE',  ( 147.2287565553230309, -1.999999999999976241, -29.49038105676660138 ) ) ;
#1164 = CARTESIAN_POINT ( 'NONE',  ( 30.91631662189391250, -8.208988707411489116, -18.28093047724294351 ) ) ;
#1165 = CARTESIAN_POINT ( 'NONE',  ( 22.59259966355045890, -3.831908474886262184, -12.47183693924707804 ) ) ;
#1166 = VECTOR ( 'NONE', #19580, 1000.000000000000000 ) ;
#1167 = ORIENTED_EDGE ( 'NONE', *, *, #26607, .F. ) ;
#1168 = EDGE_CURVE ( 'NONE', #13842, #18112, #10665, .T. ) ;
#1169 = EDGE_CURVE ( 'NONE', #8937, #4557, #27768, .T. ) ;
#1170 = CARTESIAN_POINT ( 'NONE',  ( 151.1922820468854525, -1.999999999999974909, -28.06379628232387802 ) ) ;
#1171 = ADVANCED_FACE ( 'NONE', ( #19504 ), #21952, .T. ) ;
#1172 = EDGE_LOOP ( 'NONE', ( #6000, #17827, #10475, #18155 ) ) ;
#1173 = ADVANCED_FACE ( 'NONE', ( #24550 ), #12478, .T. ) ;
#1174 = DIRECTION ( 'NONE',  ( 0.3090169943749472292, 8.338696094057992503E-17, -0.9510565162951536422 ) ) ;
#1175 = ORIENTED_EDGE ( 'NONE', *, *, #14689, .F. ) ;
#1176 = CARTESIAN_POINT ( 'NONE',  ( 63.44486372867152824, -29.99999999999998934, -186.4312945166758482 ) ) ;
#1177 = CARTESIAN_POINT ( 'NONE',  ( 143.6922820468854525, -4.999999999999978684, -35.24709285013155835 ) ) ;
#1178 = DIRECTION ( 'NONE',  ( 0.5877852522924731371, 1.586114251531760728E-16, 0.8090169943749474513 ) ) ;
#1179 = DIRECTION ( 'NONE',  ( 1.000000000000000000, 0.000000000000000000, 0.000000000000000000 ) ) ;
#1180 = CARTESIAN_POINT ( 'NONE',  ( 34.36632712588347260, -12.38074715364594347, -19.93031689919964222 ) ) ;
#1181 = CARTESIAN_POINT ( 'NONE',  ( 9.916411867603999397, 16.40742607105030260, -16.50456570466356965 ) ) ;
#1182 = AXIS2_PLACEMENT_3D ( 'NONE', #27480, #22255, #20556 ) ;
#1183 = PLANE ( 'NONE',  #10266 ) ;
#1184 = CARTESIAN_POINT ( 'NONE',  ( 4.000000000000019540, 6.928203230275512325, -5.000000000000000888 ) ) ;
#1185 = CARTESIAN_POINT ( 'NONE',  ( 9.661883061612440926, 16.25482663361732705, -17.91796598306941135 ) ) ;
#1186 = CARTESIAN_POINT ( 'NONE',  ( 20.00000000000017053, 34.64101615137744972, 10.00000000000000178 ) ) ;
#1187 = EDGE_LOOP ( 'NONE', ( #17493, #27791 ) ) ;
#1188 = CARTESIAN_POINT ( 'NONE',  ( 174.5152310637604103, -1.999999999999969580, -13.05155085951651195 ) ) ;
#1189 = EDGE_LOOP ( 'NONE', ( #30137, #13203, #16635, #25070, #21703 ) ) ;
#1190 = CARTESIAN_POINT ( 'NONE',  ( 129.5152310637605524, -10.00000000000000888, -13.05155085951650840 ) ) ;
#1191 = CARTESIAN_POINT ( 'NONE',  ( 10.44167955025612926, -5.000000000000015099, 32.13618525228277889 ) ) ;
#1192 = DIRECTION ( 'NONE',  ( -2.698458740408365879E-16, 1.000000000000000000, 0.000000000000000000 ) ) ;
#1193 = EDGE_LOOP ( 'NONE', ( #18358, #3083, #23610, #782 ) ) ;
#1194 = VERTEX_POINT ( 'NONE', #21803 ) ;
#1195 = ORIENTED_EDGE ( 'NONE', *, *, #86, .T. ) ;
#1196 = CARTESIAN_POINT ( 'NONE',  ( 8.944584663113916534, 16.95159285377954461, -17.91618150236991269 ) ) ;
#1197 = ORIENTED_EDGE ( 'NONE', *, *, #25697, .T. ) ;
#1198 = CARTESIAN_POINT ( 'NONE',  ( 15.41439956623108642, 10.93483300904300215, -14.25553973300288568 ) ) ;
#1199 = CARTESIAN_POINT ( 'NONE',  ( 27.03959252790357581, -7.665547941290169476, -19.57376043866218041 ) ) ;
#1200 = CARTESIAN_POINT ( 'NONE',  ( 138.6922820468854525, -1.999999999999979572, -26.58683881228715506 ) ) ;
#1201 = CARTESIAN_POINT ( 'NONE',  ( 138.6922820468854525, -4.999999999999980460, -9.266330736598359152 ) ) ;
#1202 = DIRECTION ( 'NONE',  ( 0.3090169943749472292, 8.338696094057992503E-17, -0.9510565162951536422 ) ) ;
#1203 = EDGE_CURVE ( 'NONE', #20918, #28729, #900, .T. ) ;
#1204 = ADVANCED_FACE ( 'NONE', ( #14760 ), #29330, .T. ) ;
#1205 = AXIS2_PLACEMENT_3D ( 'NONE', #17330, #24367, #28843 ) ;
#1206 = ORIENTED_EDGE ( 'NONE', *, *, #21520, .T. ) ;
#1207 = EDGE_CURVE ( 'NONE', #30188, #16793, #8258, .T. ) ;
#1208 = DIRECTION ( 'NONE',  ( 0.9510565162951536422, 2.566386769018988816E-16, 0.3090169943749472292 ) ) ;
#1209 = DIRECTION ( 'NONE',  ( -1.387778780781445922E-16, 0.000000000000000000, 1.000000000000000000 ) ) ;
#1210 = CARTESIAN_POINT ( 'NONE',  ( 168.6922820468853388, -1.999999999999971356, -15.07341522555727664 ) ) ;
#1211 = CARTESIAN_POINT ( 'NONE',  ( 131.1922820468854241, -10.00000000000000888, -2.083034168790677043 ) ) ;
#1212 = CARTESIAN_POINT ( 'NONE',  ( 12.02859841272590735, 9.313533661810568631, -16.69110409223909741 ) ) ;
#1213 = CARTESIAN_POINT ( 'NONE',  ( 33.51257387524950815, -12.16639167148776224, -18.62538556556795655 ) ) ;
#1214 = ORIENTED_EDGE ( 'NONE', *, *, #194, .T. ) ;
#1215 = CARTESIAN_POINT ( 'NONE',  ( 9.008298112641352162, 16.65939485267133335, -17.25320607661530303 ) ) ;
#1216 = CARTESIAN_POINT ( 'NONE',  ( 23.21730923944814506, -4.364887171357101359, -13.63095412955673247 ) ) ;
#1217 = CARTESIAN_POINT ( 'NONE',  ( 10.35865474790814211, 16.97209951875106526, -17.91014213605047445 ) ) ;
#1218 = FACE_BOUND ( 'NONE', #105, .T. ) ;
#1219 = EDGE_LOOP ( 'NONE', ( #14532, #205, #5357, #26295 ) ) ;
#1220 = PLANE ( 'NONE',  #21848 ) ;
#1221 = VECTOR ( 'NONE', #25377, 1000.000000000000000 ) ;
#1222 = CARTESIAN_POINT ( 'NONE',  ( 11.47304865262203499, 9.268493388164605662, -15.86084085272616484 ) ) ;
#1223 = DIRECTION ( 'NONE',  ( 0.5877852522924731371, 1.586114251531760728E-16, 0.8090169943749474513 ) ) ;
#1224 = ORIENTED_EDGE ( 'NONE', *, *, #18694, .F. ) ;
#1225 = ORIENTED_EDGE ( 'NONE', *, *, #29517, .T. ) ;
#1226 = DIRECTION ( 'NONE',  ( -2.698458740408365879E-16, 1.000000000000000000, 0.000000000000000000 ) ) ;
#1227 = ORIENTED_EDGE ( 'NONE', *, *, #6644, .T. ) ;
#1228 = CARTESIAN_POINT ( 'NONE',  ( 12.14965596459611774, 8.983642127099937369, -16.62385966901067391 ) ) ;
#1229 = EDGE_LOOP ( 'NONE', ( #14138, #4239, #19331, #10820, #23032 ) ) ;
#1230 = CARTESIAN_POINT ( 'NONE',  ( 20.25609397779747312, 2.611002146465201346, -20.92159891259701610 ) ) ;
#1231 = CARTESIAN_POINT ( 'NONE',  ( 20.53425600248055005, 0.8933117467920750343, -13.02782074225586406 ) ) ;
#1232 = ORIENTED_EDGE ( 'NONE', *, *, #25979, .F. ) ;
#1233 = FACE_OUTER_BOUND ( 'NONE', #4292, .T. ) ;
#1234 = ORIENTED_EDGE ( 'NONE', *, *, #23247, .T. ) ;
#1235 = CARTESIAN_POINT ( 'NONE',  ( 35.97124720801268438, -19.59080293283771823, -20.41544573823858144 ) ) ;
#1237 = VECTOR ( 'NONE', #26071, 1000.000000000000000 ) ;
#1236 = CONTEXT_DEPENDENT_SHAPE_REPRESENTATION ( #4050, #20562 ) ;
#1238 = CARTESIAN_POINT ( 'NONE',  ( 17.88091890332929523, 4.544920326333207861, -13.91018511019278669 ) ) ;
#1239 = EDGE_CURVE ( 'NONE', #12966, #20254, #11655, .T. ) ;
#1240 = EDGE_CURVE ( 'NONE', #9967, #24305, #740, .T. ) ;
#1241 = CARTESIAN_POINT ( 'NONE',  ( 144.5152310637605240, -10.00000000000000355, -4.391296821672111328 ) ) ;
#1242 = EDGE_CURVE ( 'NONE', #20723, #18076, #17360, .T. ) ;
#1243 = CARTESIAN_POINT ( 'NONE',  ( 162.0152310637605240, -9.999999999999998224, -24.27857615940569502 ) ) ;
#1244 = VECTOR ( 'NONE', #10046, 1000.000000000000000 ) ;
#1245 = DIRECTION ( 'NONE',  ( -2.698458740408365879E-16, 1.000000000000000000, 0.000000000000000000 ) ) ;
#1246 = CARTESIAN_POINT ( 'NONE',  ( 31.49119590023542870, -10.87553819600004701, -15.10823507476435523 ) ) ;
#1247 = LINE ( 'NONE', #10385, #19941 ) ;
#1248 = CARTESIAN_POINT ( 'NONE',  ( 161.1922820468853104, -10.00000000000000000, -4.936203717676158398 ) ) ;
#1249 = CARTESIAN_POINT ( 'NONE',  ( 11.05541531668977662, 17.68942339022145305, -17.92454625180715411 ) ) ;
#1250 = CARTESIAN_POINT ( 'NONE',  ( 143.6922820468854525, -4.999999999999978684, -32.39392330124607611 ) ) ;
#1251 = CIRCLE ( 'NONE', #12936, 5.000000000000000888 ) ;
#1252 = ORIENTED_EDGE ( 'NONE', *, *, #2182, .F. ) ;
#1253 = CARTESIAN_POINT ( 'NONE',  ( 7.345652830558766055, -4.996589667937400669, -4.503584543331195178 ) ) ;
#1254 = EDGE_LOOP ( 'NONE', ( #813, #8774, #21079, #1162 ) ) ;
#1255 = CARTESIAN_POINT ( 'NONE',  ( 12.49957999542663600, 8.570517509188613658, -15.13050969259218981 ) ) ;
#1256 = ORIENTED_EDGE ( 'NONE', *, *, #10863, .F. ) ;
#1257 = AXIS2_PLACEMENT_3D ( 'NONE', #13555, #9262, #9415 ) ;
#1258 = CARTESIAN_POINT ( 'NONE',  ( 10.67240773364005868, 9.027839897374207112, -16.40964036978800777 ) ) ;
#1259 = DIRECTION ( 'NONE',  ( 0.5877852522924731371, 1.586114251531760728E-16, 0.8090169943749474513 ) ) ;
#1260 = CARTESIAN_POINT ( 'NONE',  ( 167.2287565553228887, -9.999999999999998224, -3.509618943233403510 ) ) ;
#1261 = ORIENTED_EDGE ( 'NONE', *, *, #2384, .T. ) ;
#1262 = ORIENTED_EDGE ( 'NONE', *, *, #18176, .T. ) ;
#1263 = CARTESIAN_POINT ( 'NONE',  ( 130.7287565553229172, -4.999999999999983125, -4.785595155761463104 ) ) ;
#1264 = ORIENTED_EDGE ( 'NONE', *, *, #29614, .F. ) ;
#1265 = CARTESIAN_POINT ( 'NONE',  ( 12.83192189813640738, 9.542137755788996145, -16.14117592875819440 ) ) ;
#1267 = CARTESIAN_POINT ( 'NONE',  ( 34.59231264378541937, -12.39598037772099559, -18.95630535174095499 ) ) ;
#1266 = VECTOR ( 'NONE', #954, 1000.000000000000000 ) ;
#1268 = CARTESIAN_POINT ( 'NONE',  ( 22.34083945069921739, -4.755659482961629436, -14.12236044035638116 ) ) ;
#1269 = ORIENTED_EDGE ( 'NONE', *, *, #25835, .F. ) ;
#1270 = ORIENTED_EDGE ( 'NONE', *, *, #7022, .T. ) ;
#1271 = LINE ( 'NONE', #10560, #11580 ) ;
#1272 = CARTESIAN_POINT ( 'NONE',  ( 18.47844294452917424, 10.16049799425131361, -18.92511192449534718 ) ) ;
#1273 = CARTESIAN_POINT ( 'NONE',  ( 151.1922820468854525, -10.00000000000000178, -30.91696583120936026 ) ) ;
#1274 = LINE ( 'NONE', #5847, #25670 ) ;
#1275 = CARTESIAN_POINT ( 'NONE',  ( 21.00058363250239069, -3.857595149258782996, -18.17417979037076847 ) ) ;
#1276 = CARTESIAN_POINT ( 'NONE',  ( 18.66675855576620791, -1.414919486740021881, -19.12600662388792117 ) ) ;
#1277 = EDGE_CURVE ( 'NONE', #21320, #24253, #5934, .T. ) ;
#1279 = ORIENTED_EDGE ( 'NONE', *, *, #13693, .T. ) ;
#1278 = EDGE_CURVE ( 'NONE', #14937, #21885, #26548, .T. ) ;
#1280 = ORIENTED_EDGE ( 'NONE', *, *, #28806, .T. ) ;
#1281 = DIRECTION ( 'NONE',  ( -0.000000000000000000, -0.000000000000000000, 1.000000000000000000 ) ) ;
#1282 = CARTESIAN_POINT ( 'NONE',  ( 153.6922820468853672, -1.999999999999975797, -9.266330736598359152 ) ) ;
#1283 = VECTOR ( 'NONE', #27792, 1000.000000000000000 ) ;
#1284 = CARTESIAN_POINT ( 'NONE',  ( 167.0152310637605240, -4.999999999999972466, -24.27857615940569502 ) ) ;
#1285 = DIRECTION ( 'NONE',  ( 0.5877852522924731371, 1.586114251531760728E-16, 0.8090169943749474513 ) ) ;
#1286 = LINE ( 'NONE', #10577, #5814 ) ;
#1287 = AXIS2_PLACEMENT_3D ( 'NONE', #24642, #17167, #24199 ) ;
#1288 = CARTESIAN_POINT ( 'NONE',  ( 142.0152310637606092, -4.999999999999979572, -24.27857615940569147 ) ) ;
#1289 = CONICAL_SURFACE ( 'NONE', #16877, 4.000000000000003553, 1.047197551196597853 ) ;
#1290 = CARTESIAN_POINT ( 'NONE',  ( 11.47250673971808688, 9.270976631574885829, -15.86106510822916249 ) ) ;
#1291 = CARTESIAN_POINT ( 'NONE',  ( 26.84208138670940968, -2.489200896322508516, -17.35162900556907317 ) ) ;
#1292 = ORIENTED_EDGE ( 'NONE', *, *, #6329, .F. ) ;
#1293 = DIRECTION ( 'NONE',  ( 1.000000000000000000, 4.440892098500622217E-16, 0.000000000000000000 ) ) ;
#1294 = DIRECTION ( 'NONE',  ( -0.8090169943749474513, -2.183098979609982436E-16, 0.5877852522924731371 ) ) ;
#1295 = DIRECTION ( 'NONE',  ( -0.000000000000000000, -0.000000000000000000, 1.000000000000000000 ) ) ;
#1296 = DIRECTION ( 'NONE',  ( 0.9510565162951535312, 2.566386769018988816E-16, -0.3090169943749475623 ) ) ;
#1297 = DIRECTION ( 'NONE',  ( 1.000000000000000000, 4.440892098500622217E-16, 0.000000000000000000 ) ) ;
#1298 = SURFACE_STYLE_USAGE ( .BOTH. , #24196 ) ;
#1300 = ORIENTED_EDGE ( 'NONE', *, *, #3032, .F. ) ;
#1299 = CARTESIAN_POINT ( 'NONE',  ( 19.25770813156441008, -2.543370271471735222, -15.40753146551623587 ) ) ;
#1301 = EDGE_LOOP ( 'NONE', ( #27535, #10792, #12334, #6173 ) ) ;
#1302 = CARTESIAN_POINT ( 'NONE',  ( 148.6922820468854525, -4.999999999999977796, -32.39392330124607611 ) ) ;
#1303 = CARTESIAN_POINT ( 'NONE',  ( 12.25668235260104844, 9.587403967970216101, -15.31905460325341117 ) ) ;
#1304 = ADVANCED_FACE ( 'NONE', ( #10036 ), #15218, .F. ) ;
#1305 = ORIENTED_EDGE ( 'NONE', *, *, #467, .F. ) ;
#1306 = CARTESIAN_POINT ( 'NONE',  ( 32.00110207675911767, -10.95298233446834502, -16.54939777171900417 ) ) ;
#1307 = DIRECTION ( 'NONE',  ( 0.9510565162951535312, 2.566386769018988816E-16, -0.3090169943749475623 ) ) ;
#1308 = CIRCLE ( 'NONE', #27647, 5.000000000000005329 ) ;
#1309 = CARTESIAN_POINT ( 'NONE',  ( 19.50856600871340873, -1.908691058934758100, -18.90332006808282728 ) ) ;
#1310 = DIRECTION ( 'NONE',  ( -2.698458740408365879E-16, 1.000000000000000000, 0.000000000000000000 ) ) ;
#1311 = CARTESIAN_POINT ( 'NONE',  ( 18.41232452102509143, -0.3525767977158695277, -15.58598945151665305 ) ) ;
#1312 = ORIENTED_EDGE ( 'NONE', *, *, #16099, .F. ) ;
#1313 = CARTESIAN_POINT ( 'NONE',  ( 166.1922820468853672, -4.999999999999973355, -30.91696583120936026 ) ) ;
#1314 = CARTESIAN_POINT ( 'NONE',  ( 22.23398510282979146, -6.138177547518383292, -17.55864386164050472 ) ) ;
#1315 = VECTOR ( 'NONE', #24304, 1000.000000000000000 ) ;
#1316 = CARTESIAN_POINT ( 'NONE',  ( 22.08361411416106534, -2.618483922437499611, -20.46533185456077319 ) ) ;
#1317 = VECTOR ( 'NONE', #2050, 1000.000000000000000 ) ;
#1318 = EDGE_CURVE ( 'NONE', #29111, #22823, #24707, .T. ) ;
#1319 = ORIENTED_EDGE ( 'NONE', *, *, #27218, .F. ) ;
#1320 = CARTESIAN_POINT ( 'NONE',  ( -2.645508037661914003, -7.710219529346629130, -0.06809871960544379432 ) ) ;
#1321 = DIRECTION ( 'NONE',  ( 0.5877852522924731371, 0.000000000000000000, 0.8090169943749474513 ) ) ;
#1322 = PLANE ( 'NONE',  #24864 ) ;
#1323 = CARTESIAN_POINT ( 'NONE',  ( 153.6922820468853672, -1.999999999999975797, -6.413161187712877798 ) ) ;
#1324 = CARTESIAN_POINT ( 'NONE',  ( 158.6922820468853388, -10.00000000000000000, -6.413161187712876909 ) ) ;
#1325 = CIRCLE ( 'NONE', #9068, 4.187999999999997947 ) ;
#1326 = CARTESIAN_POINT ( 'NONE',  ( 154.5152310637604671, -10.00000000000000178, -4.391296821672111328 ) ) ;
#1327 = CARTESIAN_POINT ( 'NONE',  ( 28.80153578082395427, -7.039779562103731791, -13.29052886957691371 ) ) ;
#1328 = CARTESIAN_POINT ( 'NONE',  ( 13.15390973649967599, 8.859676595473322536, -14.60899741038990562 ) ) ;
#1329 = CARTESIAN_POINT ( 'NONE',  ( 36.54779501103016770, -22.18092680593016652, -18.48200341583098449 ) ) ;
#1330 = CARTESIAN_POINT ( 'NONE',  ( 169.5152310637604103, -1.999999999999971356, -4.391296821672111328 ) ) ;
#1331 = AXIS2_PLACEMENT_3D ( 'NONE', #11597, #23666, #18635 ) ;
#1332 = CARTESIAN_POINT ( 'NONE',  ( 9.917332382238186028, 16.40320447359955125, -16.50418441153501448 ) ) ;
#1333 = VECTOR ( 'NONE', #15989, 1000.000000000000000 ) ;
#1334 = LINE ( 'NONE', #4363, #17592 ) ;
#1335 = FACE_OUTER_BOUND ( 'NONE', #23321, .T. ) ;
#1336 = CARTESIAN_POINT ( 'NONE',  ( 9.661883061612440926, 16.25482663361732705, -17.91928203681695564 ) ) ;
#1337 = DIRECTION ( 'NONE',  ( 0.000000000000000000, 0.000000000000000000, 1.000000000000000000 ) ) ;
#1338 = VERTEX_POINT ( 'NONE', #29162 ) ;
#1339 = CARTESIAN_POINT ( 'NONE',  ( -15.99999999999998224, -1.561251128379126385E-14, 0.000000000000000000 ) ) ;
#1340 = CARTESIAN_POINT ( 'NONE',  ( 9.924804006935172396, 16.36893865032855899, -16.50109463189289016 ) ) ;
#1341 = ORIENTED_EDGE ( 'NONE', *, *, #24841, .T. ) ;
#1342 = ADVANCED_FACE ( 'NONE', ( #19799 ), #12325, .T. ) ;
#1343 = EDGE_LOOP ( 'NONE', ( #9182, #27199, #3969, #12528, #1225 ) ) ;
#1344 = DIRECTION ( 'NONE',  ( 1.000000000000000000, -0.000000000000000000, -0.000000000000000000 ) ) ;
#1345 = DIRECTION ( 'NONE',  ( -0.9510565162951536422, -2.566386769018988816E-16, -0.3090169943749472292 ) ) ;
#1346 = EDGE_CURVE ( 'NONE', #13830, #17432, #3201, .T. ) ;
#1347 = LINE ( 'NONE', #5613, #2489 ) ;
#1348 = ORIENTED_EDGE ( 'NONE', *, *, #20074, .F. ) ;
#1349 = CARTESIAN_POINT ( 'NONE',  ( 8.944584683310379702, 16.95159276115599667, -23.00000000000000711 ) ) ;
#1350 = ORIENTED_EDGE ( 'NONE', *, *, #7117, .F. ) ;
#1351 = CARTESIAN_POINT ( 'NONE',  ( 27.68941694697105760, -11.75984073208553582, -11.85267853464266352 ) ) ;
#1352 = CARTESIAN_POINT ( 'NONE',  ( 25.66600519952783799, -8.909200411882650883, -19.30012332941604924 ) ) ;
#1353 = AXIS2_PLACEMENT_3D ( 'NONE', #29693, #27677, #13439 ) ;
#1354 = FACE_OUTER_BOUND ( 'NONE', #2002, .T. ) ;
#1355 = CARTESIAN_POINT ( 'NONE',  ( 101.7267641804769056, -4.999999999999989342, -73.90882041348888265 ) ) ;
#1356 = LINE ( 'NONE', #19643, #3062 ) ;
#1357 = CONICAL_SURFACE ( 'NONE', #21798, 4.000000000000003553, 1.047197551196597853 ) ;
#1358 = EDGE_LOOP ( 'NONE', ( #8368, #24068, #2089, #226 ) ) ;
#1359 = CARTESIAN_POINT ( 'NONE',  ( 143.6922820468854525, -4.999999999999978684, -15.07341522555727664 ) ) ;
#1360 = VECTOR ( 'NONE', #4468, 1000.000000000000000 ) ;
#1361 = CARTESIAN_POINT ( 'NONE',  ( 152.0152310637605808, -10.00000000000000000, -24.27857615940569502 ) ) ;
#1362 = FACE_OUTER_BOUND ( 'NONE', #5538, .T. ) ;
#1363 = LINE ( 'NONE', #8657, #3133 ) ;
#1364 = CARTESIAN_POINT ( 'NONE',  ( 13.11043623405165448, 8.565188957795726310, -15.92239833454181230 ) ) ;
#1365 = CARTESIAN_POINT ( 'NONE',  ( 32.61797162530606187, -11.69648652134232414, -16.29118568026193614 ) ) ;
#1366 = VERTEX_POINT ( 'NONE', #1668 ) ;
#1367 = CARTESIAN_POINT ( 'NONE',  ( 9.112490548836888138, 16.18155505883174783, -17.05474119751274031 ) ) ;
#1368 = ORIENTED_EDGE ( 'NONE', *, *, #19922, .T. ) ;
#1369 = VECTOR ( 'NONE', #21068, 1000.000000000000000 ) ;
#1370 = CARTESIAN_POINT ( 'NONE',  ( 21.43917814492346707, -4.799604530101110988, -17.97822123721208243 ) ) ;
#1371 = CARTESIAN_POINT ( 'NONE',  ( 13.00452062571394229, 9.576253617860157163, -16.00682707811506233 ) ) ;
#1372 = FACE_BOUND ( 'NONE', #2319, .T. ) ;
#1373 = EDGE_CURVE ( 'NONE', #26457, #18739, #13247, .T. ) ;
#1374 = ORIENTED_EDGE ( 'NONE', *, *, #5125, .F. ) ;
#1375 = DIRECTION ( 'NONE',  ( -0.9510565162951536422, -2.566386769018988323E-16, 0.3090169943749475623 ) ) ;
#1376 = EDGE_CURVE ( 'NONE', #20136, #19188, #29491, .T. ) ;
#1377 = CARTESIAN_POINT ( 'NONE',  ( 11.47276097331165623, 9.269810413962238371, -15.86095999428340697 ) ) ;
#1378 = DIRECTION ( 'NONE',  ( 1.110223024625156540E-16, 2.995891024602366092E-32, 1.000000000000000000 ) ) ;
#1379 = EDGE_CURVE ( 'NONE', #9909, #26420, #29640, .T. ) ;
#1380 = ORIENTED_EDGE ( 'NONE', *, *, #6468, .F. ) ;
#1381 = ORIENTED_EDGE ( 'NONE', *, *, #25320, .T. ) ;
#1382 = CARTESIAN_POINT ( 'NONE',  ( 139.5152310637605808, -10.00000000000000533, -21.71180489736090991 ) ) ;
#1383 = ORIENTED_EDGE ( 'NONE', *, *, #3958, .F. ) ;
#1384 = CARTESIAN_POINT ( 'NONE',  ( 9.661883061612440926, 16.25482663361732705, -17.98596209335946128 ) ) ;
#1385 = ORIENTED_EDGE ( 'NONE', *, *, #24357, .T. ) ;
#1386 = CARTESIAN_POINT ( 'NONE',  ( 22.56675539556120924, 5.189497681140571750, -18.50903523470404011 ) ) ;
#1387 = CARTESIAN_POINT ( 'NONE',  ( 19.63206833423595299, 9.033623817254925470, -16.13982763006638166 ) ) ;
#1388 = ORIENTED_EDGE ( 'NONE', *, *, #13725, .F. ) ;
#1389 = DIRECTION ( 'NONE',  ( -0.5877852522924731371, -1.586114251531760728E-16, -0.8090169943749474513 ) ) ;
#1390 = ORIENTED_EDGE ( 'NONE', *, *, #27011, .F. ) ;
#1391 = FACE_OUTER_BOUND ( 'NONE', #22443, .T. ) ;
#1392 = CARTESIAN_POINT ( 'NONE',  ( 16.53304876882650731, 8.555045913257369961, -19.77053526944897754 ) ) ;
#1393 = CIRCLE ( 'NONE', #1883, 4.756499999999999062 ) ;
#1394 = LINE ( 'NONE', #11136, #2747 ) ;
#1395 = FACE_BOUND ( 'NONE', #5957, .T. ) ;
#1396 = VECTOR ( 'NONE', #22128, 1000.000000000000000 ) ;
#1397 = VERTEX_POINT ( 'NONE', #18266 ) ;
#1398 = VECTOR ( 'NONE', #14979, 1000.000000000000000 ) ;
#1399 = PLANE ( 'NONE',  #23067 ) ;
#1400 = CARTESIAN_POINT ( 'NONE',  ( 33.57712230886461668, -13.32773824946660923, -19.76201999124979736 ) ) ;
#1401 = DIRECTION ( 'NONE',  ( 0.000000000000000000, 0.000000000000000000, 1.000000000000000000 ) ) ;
#1402 = ORIENTED_EDGE ( 'NONE', *, *, #6678, .T. ) ;
#1403 = VERTEX_POINT ( 'NONE', #27621 ) ;
#1404 = LINE ( 'NONE', #24903, #16830 ) ;
#1405 = CARTESIAN_POINT ( 'NONE',  ( 12.35402573141577598, 9.564223303342972216, -15.24651908135525957 ) ) ;
#1406 = DIRECTION ( 'NONE',  ( -0.000000000000000000, 0.000000000000000000, 1.000000000000000000 ) ) ;
#1407 = VERTEX_POINT ( 'NONE', #11252 ) ;
#1408 = CARTESIAN_POINT ( 'NONE',  ( 13.04501788334644630, 8.811555337407297017, -14.69578613943112799 ) ) ;
#1409 = VERTEX_POINT ( 'NONE', #4241 ) ;
#1410 = ADVANCED_FACE ( 'NONE', ( #20402 ), #3946, .F. ) ;
#1411 = CARTESIAN_POINT ( 'NONE',  ( 10.66667607898454939, 9.053862104998891880, -16.41203073725236905 ) ) ;
#1412 = PLANE ( 'NONE',  #7355 ) ;
#1413 = CARTESIAN_POINT ( 'NONE',  ( 20.00000000000000711, 60.00000000000000711, 29.99999999999998579 ) ) ;
#1414 = EDGE_CURVE ( 'NONE', #4557, #23709, #24844, .T. ) ;
#1415 = EDGE_CURVE ( 'NONE', #24408, #23323, #4094, .T. ) ;
#1416 = CARTESIAN_POINT ( 'NONE',  ( 13.77718166750865869, 8.859676595473324312, -15.39100258941132182 ) ) ;
#1417 = EDGE_CURVE ( 'NONE', #18587, #23159, #20697, .T. ) ;
#1418 = ORIENTED_EDGE ( 'NONE', *, *, #6948, .T. ) ;
#1419 = CARTESIAN_POINT ( 'NONE',  ( 12.86818510107347890, 9.516005823298000266, -16.11548879760486130 ) ) ;
#1420 = VECTOR ( 'NONE', #541, 1000.000000000000000 ) ;
#1421 = CARTESIAN_POINT ( 'NONE',  ( 36.25073006198487491, -19.84637134955221072, -19.45760515208133512 ) ) ;
#1422 = CARTESIAN_POINT ( 'NONE',  ( 23.66601916330066402, 2.199037240492611733, -18.57254039386976885 ) ) ;
#1423 = ORIENTED_EDGE ( 'NONE', *, *, #28318, .F. ) ;
#1424 = VERTEX_POINT ( 'NONE', #27774 ) ;
#1425 = DIRECTION ( 'NONE',  ( -0.5877852522924731371, -1.586114251531760235E-16, 0.8090169943749474513 ) ) ;
#1426 = ORIENTED_EDGE ( 'NONE', *, *, #17039, .T. ) ;
#1427 = VECTOR ( 'NONE', #29243, 999.9999999999998863 ) ;
#1428 = PLANE ( 'NONE',  #29908 ) ;
#1429 = CARTESIAN_POINT ( 'NONE',  ( 26.64416741123070054, -12.70369174447049332, -17.39020166599120643 ) ) ;
#1430 = CARTESIAN_POINT ( 'NONE',  ( 18.16797961131436523, 4.950584380424773556, -14.83967967756414730 ) ) ;
#1431 = ORIENTED_EDGE ( 'NONE', *, *, #20132, .F. ) ;
#1432 = ORIENTED_EDGE ( 'NONE', *, *, #6569, .F. ) ;
#1433 = CARTESIAN_POINT ( 'NONE',  ( 0.000000000000000000, 0.000000000000000000, -23.00000000000000000 ) ) ;
#1434 = CARTESIAN_POINT ( 'NONE',  ( 2.000000000000003553, -3.464101615137736623, 8.673617379884035472E-16 ) ) ;
#1435 = DIRECTION ( 'NONE',  ( -2.698458740408365879E-16, 1.000000000000000000, 0.000000000000000000 ) ) ;
#1436 = LINE ( 'NONE', #17593, #25213 ) ;
#1437 = VECTOR ( 'NONE', #500, 1000.000000000000000 ) ;
#1438 = CARTESIAN_POINT ( 'NONE',  ( -8.000000000000003553, -4.618802153517037823, -4.285468820183664818 ) ) ;
#1439 = DIRECTION ( 'NONE',  ( 0.5877852522924731371, 1.586114251531760728E-16, 0.8090169943749474513 ) ) ;
#1440 = CARTESIAN_POINT ( 'NONE',  ( 11.19157713609530269, 9.239454617397717229, -17.25496879848155629 ) ) ;
#1441 = CARTESIAN_POINT ( 'NONE',  ( 12.48484057295006977, 8.564241722236854315, -15.14223913367768759 ) ) ;
#1442 = AXIS2_PLACEMENT_3D ( 'NONE', #27922, #25750, #6981 ) ;
#1443 = CARTESIAN_POINT ( 'NONE',  ( 23.54468722040186890, -6.934586491718037315, -13.40271233150634878 ) ) ;
#1444 = EDGE_LOOP ( 'NONE', ( #23395, #23568, #5169, #4778 ) ) ;
#1445 = CLOSED_SHELL ( 'NONE', ( #15132, #20882, #7737, #23190, #12590, #9060, #28804, #19502, #3783, #27996, #7327, #29752, #648, #8113, #11444, #4693, #302, #29167, #4024, #17444, #21025, #26089, #10107, #19688, #21517, #24283, #29171 ) ) ;
#1446 = DIRECTION ( 'NONE',  ( -1.110223024625156540E-16, 0.000000000000000000, -1.000000000000000000 ) ) ;
#1447 = DIRECTION ( 'NONE',  ( 0.000000000000000000, 0.000000000000000000, 1.000000000000000000 ) ) ;
#1448 = EDGE_LOOP ( 'NONE', ( #28288, #1390, #21032, #9698 ) ) ;
#1449 = DIRECTION ( 'NONE',  ( -1.110223024625156540E-16, 0.000000000000000000, -1.000000000000000000 ) ) ;
#1450 = EDGE_CURVE ( 'NONE', #2343, #15349, #27174, .T. ) ;
#1451 = DIRECTION ( 'NONE',  ( 0.3090169943749475623, 8.338696094058001131E-17, 0.9510565162951536422 ) ) ;
#1452 = DIRECTION ( 'NONE',  ( -2.698458740408365879E-16, 1.000000000000000000, 0.000000000000000000 ) ) ;
#1453 = B_SPLINE_CURVE_WITH_KNOTS ( 'NONE', 3,
 ( #650, #9935, #949, #19247, #10237, #17262 ),
 .UNSPECIFIED., .F., .F.,
 ( 4, 2, 4 ),
 ( 2.380731629582120260E-07, 0.002336973833157553367, 0.004673709593152147908 ),
 .UNSPECIFIED. ) ;
#1454 = EDGE_CURVE ( 'NONE', #14318, #9080, #6531, .T. ) ;
#1455 = CARTESIAN_POINT ( 'NONE',  ( 26.84970692451943819, -5.812874930055231815, -14.04107299160273037 ) ) ;
#1456 = EDGE_LOOP ( 'NONE', ( #22399, #8781, #21563, #9519 ) ) ;
#1457 = DIRECTION ( 'NONE',  ( -0.8090169943749474513, -2.183098979609982436E-16, -0.5877852522924731371 ) ) ;
#1458 = EDGE_CURVE ( 'NONE', #28897, #29710, #30085, .T. ) ;
#1459 = CARTESIAN_POINT ( 'NONE',  ( 10.78565875124225393, 16.33370571569710705, -15.92737460872590738 ) ) ;
#1460 = FACE_OUTER_BOUND ( 'NONE', #27089, .T. ) ;
#1461 = DIRECTION ( 'NONE',  ( 1.110223024625156540E-16, 2.995891024602366092E-32, 1.000000000000000000 ) ) ;
#1462 = CARTESIAN_POINT ( 'NONE',  ( 22.09544204423535874, -4.864148257255451746, -14.35781331922719772 ) ) ;
#1463 = CARTESIAN_POINT ( 'NONE',  ( 132.0152310637605524, -4.999999999999982236, -1.465663491281971624E-14 ) ) ;
#1464 = CARTESIAN_POINT ( 'NONE',  ( 20.51677437365689372, 7.544110930723523012, -19.48516728630390915 ) ) ;
#1465 = ORIENTED_EDGE ( 'NONE', *, *, #3746, .T. ) ;
#1466 = CYLINDRICAL_SURFACE ( 'NONE', #4682, 2.000000000000000000 ) ;
#1467 = VECTOR ( 'NONE', #2467, 1000.000000000000000 ) ;
#1468 = CARTESIAN_POINT ( 'NONE',  ( 25.64694198568010819, -13.68525919019184300, -15.02544717525507778 ) ) ;
#1469 = CARTESIAN_POINT ( 'NONE',  ( 27.64540148246904749, -2.072091111371471506, -15.50399641584551702 ) ) ;
#1470 = VECTOR ( 'NONE', #4280, 1000.000000000000000 ) ;
#1471 = VECTOR ( 'NONE', #20519, 1000.000000000000000 ) ;
#1472 = EDGE_LOOP ( 'NONE', ( #27548, #7434, #25385, #2470 ) ) ;
#1473 = CARTESIAN_POINT ( 'NONE',  ( 27.20760296572909809, -8.488227175050779394, -13.35743234967312354 ) ) ;
#1474 = DIRECTION ( 'NONE',  ( 0.3090169943749475623, 8.338696094058001131E-17, 0.9510565162951536422 ) ) ;
#1475 = EDGE_LOOP ( 'NONE', ( #18969, #23899, #5441, #13330, #15759 ) ) ;
#1476 = ORIENTED_EDGE ( 'NONE', *, *, #11789, .T. ) ;
#1477 = ADVANCED_FACE ( 'NONE', ( #11100 ), #17961, .T. ) ;
#1478 = FACE_OUTER_BOUND ( 'NONE', #12827, .T. ) ;
#1479 = MANIFOLD_SOLID_BREP ( 'Sweep3', #18491 ) ;
#1480 = DIRECTION ( 'NONE',  ( 0.9510565162951536422, 0.000000000000000000, -0.3090169943749475623 ) ) ;
#1481 = DIRECTION ( 'NONE',  ( 0.5877852522924731371, 1.586114251531760728E-16, -0.8090169943749474513 ) ) ;
#1482 = CARTESIAN_POINT ( 'NONE',  ( 8.000000000000000000, -4.618802153517027165, -0.7145311798163362926 ) ) ;
#1483 = PRODUCT_DEFINITION_FORMATION_WITH_SPECIFIED_SOURCE ( 'ANY', '', #27439, .NOT_KNOWN. ) ;
#1484 = CARTESIAN_POINT ( 'NONE',  ( 23.44948677240984480, -6.246615351793893822, -14.99377964970044808 ) ) ;
#1485 = DIRECTION ( 'NONE',  ( 0.5877852522924731371, 1.586114251531760728E-16, -0.8090169943749474513 ) ) ;
#1486 = CARTESIAN_POINT ( 'NONE',  ( 32.94969931363368687, -9.746457777152386370, -18.95700739231402920 ) ) ;
#1488 = FACE_OUTER_BOUND ( 'NONE', #26207, .T. ) ;
#1487 = VECTOR ( 'NONE', #6963, 1000.000000000000000 ) ;
#1489 = CARTESIAN_POINT ( 'NONE',  ( 9.916824447075894611, 16.40553392900050156, -16.50439446175997205 ) ) ;
#1490 = VECTOR ( 'NONE', #16844, 1000.000000000000000 ) ;
#1491 = CARTESIAN_POINT ( 'NONE',  ( 149.7287565553230309, -1.999999999999975353, -25.16025403784440329 ) ) ;
#1492 = CARTESIAN_POINT ( 'NONE',  ( 7.817546131999246306, -5.000000000000015987, 24.05993303156214935 ) ) ;
#1493 = CARTESIAN_POINT ( 'NONE',  ( 9.661884236495001943, 16.25482124545614937, -17.91517755594902894 ) ) ;
#1494 = LINE ( 'NONE', #10782, #14605 ) ;
#1495 = LINE ( 'NONE', #24378, #14460 ) ;
#1496 = CARTESIAN_POINT ( 'NONE',  ( 11.49350937636955372, 9.187954247928445284, -15.85136552863131421 ) ) ;
#1497 = EDGE_LOOP ( 'NONE', ( #806, #13423, #22171, #19869 ) ) ;
#1498 = CARTESIAN_POINT ( 'NONE',  ( 169.5152310637604387, -1.999999999999971356, -2.627941064794695691 ) ) ;
#1499 = CARTESIAN_POINT ( 'NONE',  ( 156.1922820468854241, -4.999999999999975131, -30.91696583120936026 ) ) ;
#1500 = CARTESIAN_POINT ( 'NONE',  ( 17.32873655921053313, 10.26331207550778579, -16.20725374984683143 ) ) ;
#1501 = EDGE_LOOP ( 'NONE', ( #17519, #8441, #11532, #15536 ) ) ;
#1502 = EDGE_LOOP ( 'NONE', ( #15115, #4598, #15245, #10391 ) ) ;
#1503 = CARTESIAN_POINT ( 'NONE',  ( 8.944589832665828411, 16.95156914555548866, -17.90909639166975609 ) ) ;
#1505 = VECTOR ( 'NONE', #21440, 1000.000000000000000 ) ;
#1504 = CARTESIAN_POINT ( 'NONE',  ( 31.74553205326546390, -10.26435202779689604, -17.82876124730869805 ) ) ;
#1506 = CARTESIAN_POINT ( 'NONE',  ( 13.62270618888621776, 10.12723052195839024, -14.35540206260209573 ) ) ;
#1507 = AXIS2_PLACEMENT_3D ( 'NONE', #14519, #26299, #14367 ) ;
#1508 = CARTESIAN_POINT ( 'NONE',  ( 26.83671086236671144, -5.482767762337403816, -13.01846673106422436 ) ) ;
#1509 = LINE ( 'NONE', #27327, #12596 ) ;
#1510 = DIRECTION ( 'NONE',  ( 0.5877852522924731371, 0.000000000000000000, 0.8090169943749474513 ) ) ;
#1511 = DIRECTION ( 'NONE',  ( 1.000000000000000000, 0.000000000000000000, -0.000000000000000000 ) ) ;
#1512 = AXIS2_PLACEMENT_3D ( 'NONE', #12480, #12790, #7761 ) ;
#1513 = ORIENTED_EDGE ( 'NONE', *, *, #29997, .T. ) ;
#1514 = LINE ( 'NONE', #20110, #6493 ) ;
#1515 = EDGE_CURVE ( 'NONE', #16280, #12464, #8946, .T. ) ;
#1516 =( NAMED_UNIT ( * ) SI_UNIT ( $, .STERADIAN. ) SOLID_ANGLE_UNIT ( ) );
#1517 = ADVANCED_FACE ( 'NONE', ( #19026 ), #13971, .T. ) ;
#1518 = APPLICATION_CONTEXT ( 'automotive_design' ) ;
#1519 = CARTESIAN_POINT ( 'NONE',  ( -7.999999999999998224, 1.572549600175610962, -0.06894455525513019933 ) ) ;
#1520 = CARTESIAN_POINT ( 'NONE',  ( 148.6922820468854525, -4.999999999999977796, -35.24709285013155835 ) ) ;
#1521 = EDGE_LOOP ( 'NONE', ( #9352, #12123, #6100, #25034, #22361 ) ) ;
#1522 = CARTESIAN_POINT ( 'NONE',  ( 13.19188795686497429, 8.601024833420110483, -15.85749200792911573 ) ) ;
#1523 = CARTESIAN_POINT ( 'NONE',  ( 33.45149595566165601, -11.04796323883829423, -16.41509932566969354 ) ) ;
#1524 = ORIENTED_EDGE ( 'NONE', *, *, #16902, .T. ) ;
#1525 = AXIS2_PLACEMENT_3D ( 'NONE', #5532, #7380, #9941 ) ;
#1526 = CARTESIAN_POINT ( 'NONE',  ( 9.112705230111354027, 16.18057050314154210, -17.05465234812585607 ) ) ;
#1527 = ORIENTED_EDGE ( 'NONE', *, *, #18894, .T. ) ;
#1528 = CARTESIAN_POINT ( 'NONE',  ( -8.000000000000003553, -4.618802153517037823, -4.285468820183664818 ) ) ;
#1529 = CARTESIAN_POINT ( 'NONE',  ( 10.35864918915110877, 16.97212501191939538, -17.92981046679734547 ) ) ;
#1530 = FACE_BOUND ( 'NONE', #1675, .T. ) ;
#1531 = STYLED_ITEM ( 'NONE', ( #19269 ), #18930 ) ;
#1532 = ORIENTED_EDGE ( 'NONE', *, *, #22031, .F. ) ;
#1533 = FACE_OUTER_BOUND ( 'NONE', #8235, .T. ) ;
#1534 = CARTESIAN_POINT ( 'NONE',  ( 11.47652547240386944, 9.253065934422213701, -15.85936358228339316 ) ) ;
#1535 = PLANE ( 'NONE',  #25718 ) ;
#1536 = CARTESIAN_POINT ( 'NONE',  ( 129.5152310637605524, -10.00000000000000888, -21.71180489736090991 ) ) ;
#1537 = ORIENTED_EDGE ( 'NONE', *, *, #14272, .F. ) ;
#1538 = CARTESIAN_POINT ( 'NONE',  ( 9.661883061612440926, 16.25482663361732705, -17.92981046679734547 ) ) ;
#1539 = CARTESIAN_POINT ( 'NONE',  ( 13.26656245924271005, 6.725567473591735457, -17.69027979179009691 ) ) ;
#1540 = CARTESIAN_POINT ( 'NONE',  ( 14.64418905516944314, 2.941711854493593403, -16.63492386420942282 ) ) ;
#1541 = ORIENTED_EDGE ( 'NONE', *, *, #9804, .T. ) ;
#1542 = CARTESIAN_POINT ( 'NONE',  ( 137.2287565553230309, -10.00000000000000533, -3.509618943233403510 ) ) ;
#1543 = ORIENTED_EDGE ( 'NONE', *, *, #3915, .F. ) ;
#1544 = DIRECTION ( 'NONE',  ( -0.9510565162951536422, -2.566386769018988323E-16, 0.3090169943749475623 ) ) ;
#1545 = AXIS2_PLACEMENT_3D ( 'NONE', #18091, #15948, #15655 ) ;
#1546 = VECTOR ( 'NONE', #15312, 1000.000000000000000 ) ;
#1547 = CARTESIAN_POINT ( 'NONE',  ( 22.89472691350227507, 1.279074496056108901, -19.72372301458170796 ) ) ;
#1548 = DIRECTION ( 'NONE',  ( 0.3090169943749475623, 8.338696094058001131E-17, 0.9510565162951536422 ) ) ;
#1549 = EDGE_CURVE ( 'NONE', #887, #12491, #24359, .T. ) ;
#1550 = CARTESIAN_POINT ( 'NONE',  ( 133.6922820468854241, -10.00000000000000711, -32.39392330124607611 ) ) ;
#1551 = ADVANCED_FACE ( 'NONE', ( #25908 ), #267, .T. ) ;
#1552 = EDGE_CURVE ( 'NONE', #11816, #24750, #26302, .T. ) ;
#1553 = EDGE_CURVE ( 'NONE', #17394, #5801, #23609, .T. ) ;
#1554 = VERTEX_POINT ( 'NONE', #21009 ) ;
#1555 = DIRECTION ( 'NONE',  ( -2.698458740408365879E-16, 1.000000000000000000, 0.000000000000000000 ) ) ;
#1556 = CARTESIAN_POINT ( 'NONE',  ( 32.45272648307624053, -11.02157468472264412, -17.82583700188536824 ) ) ;
#1557 = DIRECTION ( 'NONE',  ( -0.9510565162951536422, -2.566386769018988323E-16, 0.3090169943749475623 ) ) ;
#1558 = VERTEX_POINT ( 'NONE', #115 ) ;
#1559 = VERTEX_POINT ( 'NONE', #11990 ) ;
#1560 = CARTESIAN_POINT ( 'NONE',  ( 142.2287565553230309, -10.00000000000000533, -20.83012701892220164 ) ) ;
#1561 = CARTESIAN_POINT ( 'NONE',  ( 11.05541531668977662, 17.68942339022145305, -17.92981046679734547 ) ) ;
#1562 = CARTESIAN_POINT ( 'NONE',  ( 35.54859661768235668, -23.18452799999607805, -18.25366188177437365 ) ) ;
#1563 = ORIENTED_EDGE ( 'NONE', *, *, #29487, .F. ) ;
#1564 = CARTESIAN_POINT ( 'NONE',  ( 9.641350810849047548, 17.66889113945805789, -23.00000000000000711 ) ) ;
#1565 = CARTESIAN_POINT ( 'NONE',  ( 10.66059746906157635, 9.081739384948186000, -16.41454445628326297 ) ) ;
#1566 = CARTESIAN_POINT ( 'NONE',  ( 147.0152310637605808, -4.999999999999977796, -1.632196944975745421E-14 ) ) ;
#1567 = CARTESIAN_POINT ( 'NONE',  ( 159.5152310637605240, -4.999999999999974243, -1.770974823053889357E-14 ) ) ;
#1568 = ORIENTED_EDGE ( 'NONE', *, *, #25832, .F. ) ;
#1569 = CARTESIAN_POINT ( 'NONE',  ( 171.1922820468853672, -9.999999999999994671, -28.06379628232387802 ) ) ;
#1570 = EDGE_LOOP ( 'NONE', ( #4552, #9961, #24216, #10666 ) ) ;
#1571 = CARTESIAN_POINT ( 'NONE',  ( 10.35864918915110877, 16.97212501191939538, -17.92454625180715766 ) ) ;
#1572 = CARTESIAN_POINT ( 'NONE',  ( 33.42826320546385688, -10.41623213582910523, -18.33855703361424361 ) ) ;
#1573 = CARTESIAN_POINT ( 'NONE',  ( 24.79644250101478065, -1.608028467720058918, -19.02763285027648976 ) ) ;
#1574 = ORIENTED_EDGE ( 'NONE', *, *, #24026, .F. ) ;
#1575 = PRODUCT ( 'pedal', 'pedal', '', ( #24431 ) ) ;
#1576 = VECTOR ( 'NONE', #20176, 1000.000000000000000 ) ;
#1577 = ORIENTED_EDGE ( 'NONE', *, *, #23516, .F. ) ;
#1578 = CARTESIAN_POINT ( 'NONE',  ( 175.7287565553229456, -4.999999999999970690, 3.500000000000003109 ) ) ;
#1579 = FACE_OUTER_BOUND ( 'NONE', #11118, .T. ) ;
#1580 = CARTESIAN_POINT ( 'NONE',  ( 157.0152310637605524, -1.999999999999973133, -34.70218595412750773 ) ) ;
#1581 = EDGE_CURVE ( 'NONE', #6067, #24792, #488, .T. ) ;
#1582 = CARTESIAN_POINT ( 'NONE',  ( 29.00434111665888182, -5.389956126880047549, -17.18324766788818181 ) ) ;
#1583 = CARTESIAN_POINT ( 'NONE',  ( 26.07721637849146390, 0.4197350235787081774, -17.11807909718082144 ) ) ;
#1584 = AXIS2_PLACEMENT_3D ( 'NONE', #13450, #6749, #9158 ) ;
#1585 = ORIENTED_EDGE ( 'NONE', *, *, #27651, .F. ) ;
#1586 = CARTESIAN_POINT ( 'NONE',  ( 0.2500000000000002220, 0.000000000000000000, 0.000000000000000000 ) ) ;
#1587 = EDGE_CURVE ( 'NONE', #4687, #30106, #5136, .T. ) ;
#1588 = CARTESIAN_POINT ( 'NONE',  ( 172.0152310637604955, -4.999999999999970690, -1.909752701132033609E-14 ) ) ;
#1589 = EDGE_CURVE ( 'NONE', #633, #15422, #14131, .T. ) ;
#1590 = EDGE_CURVE ( 'NONE', #2176, #22297, #21310, .T. ) ;
#1591 = LINE ( 'NONE', #26788, #10873 ) ;
#1592 = DIRECTION ( 'NONE',  ( 0.5877852522924731371, 0.000000000000000000, 0.8090169943749474513 ) ) ;
#1593 = LINE ( 'NONE', #17594, #22869 ) ;
#1594 = AXIS2_PLACEMENT_3D ( 'NONE', #24585, #19543, #12977 ) ;
#1595 = DIRECTION ( 'NONE',  ( -2.698458740408365879E-16, 1.000000000000000000, 0.000000000000000000 ) ) ;
#1596 = UNCERTAINTY_MEASURE_WITH_UNIT (LENGTH_MEASURE( 1.000000000000000082E-05 ), #3021, 'distance_accuracy_value', 'NONE');
#1597 = CARTESIAN_POINT ( 'NONE',  ( 12.60230244812736800, 7.534144488243946114, -16.30820540178382316 ) ) ;
#1598 = CARTESIAN_POINT ( 'NONE',  ( 12.50906579366657390, 8.574708520419219937, -15.12294941509656354 ) ) ;
#1599 = CARTESIAN_POINT ( 'NONE',  ( 30.50415327504139285, -11.36213899161910135, -13.19862950667920565 ) ) ;
#1600 = ORIENTED_EDGE ( 'NONE', *, *, #8987, .F. ) ;
#1601 = LINE ( 'NONE', #10877, #8584 ) ;
#1602 = FACE_OUTER_BOUND ( 'NONE', #25544, .T. ) ;
#1603 = VERTEX_POINT ( 'NONE', #18722 ) ;
#1604 = CARTESIAN_POINT ( 'NONE',  ( 9.641350810849047548, 17.66889113945805789, -23.00000000000000711 ) ) ;
#1606 = DIRECTION ( 'NONE',  ( 0.5877852522924731371, 0.000000000000000000, 0.8090169943749474513 ) ) ;
#1605 = VECTOR ( 'NONE', #1061, 1000.000000000000000 ) ;
#1607 = CARTESIAN_POINT ( 'NONE',  ( -4.000000000000004441, -1.549102112939102271, -2.292104661404058774 ) ) ;
#1608 = CARTESIAN_POINT ( 'NONE',  ( 172.0152310637604387, -1.999999999999970468, -6.958068083716895558 ) ) ;
#1609 = CARTESIAN_POINT ( 'NONE',  ( 25.04068920418659161, -5.475481712173364990, -18.92835678451453774 ) ) ;
#1610 = ORIENTED_EDGE ( 'NONE', *, *, #14201, .F. ) ;
#1611 = FACE_OUTER_BOUND ( 'NONE', #1958, .T. ) ;
#1612 = CARTESIAN_POINT ( 'NONE',  ( 12.24516467974477152, 9.516115653471018732, -15.33328326133307762 ) ) ;
#1613 = CARTESIAN_POINT ( 'NONE',  ( 32.74314609665832165, -11.10724048739539782, -18.62249297335446840 ) ) ;
#1614 = FACE_BOUND ( 'NONE', #16406, .T. ) ;
#1615 = CARTESIAN_POINT ( 'NONE',  ( 27.31974442496251143, -5.660127319198639206, -14.41990313654811651 ) ) ;
#1616 = CARTESIAN_POINT ( 'NONE',  ( 134.5152310637605808, -10.00000000000000533, -2.627941064794695691 ) ) ;
#1617 = CARTESIAN_POINT ( 'NONE',  ( 22.60936069168443652, -2.585520780102871896, -18.46111163327002913 ) ) ;
#1618 = ORIENTED_EDGE ( 'NONE', *, *, #23668, .T. ) ;
#1619 = DIRECTION ( 'NONE',  ( -1.000000000000000000, 0.000000000000000000, -0.000000000000000000 ) ) ;
#1620 = CARTESIAN_POINT ( 'NONE',  ( 13.93479307118181509, 9.207276677253689812, -14.11477394318545286 ) ) ;
#1621 = VECTOR ( 'NONE', #1245, 1000.000000000000000 ) ;
#1622 = CARTESIAN_POINT ( 'NONE',  ( 26.83635784119175938, -3.902057423304301942, -19.75319010936098962 ) ) ;
#1623 = VERTEX_POINT ( 'NONE', #11844 ) ;
#1624 = ORIENTED_EDGE ( 'NONE', *, *, #12930, .T. ) ;
#1625 = CARTESIAN_POINT ( 'NONE',  ( 26.87449084144840938, -11.88902188497427481, -13.49525739704605343 ) ) ;
#1626 = ADVANCED_FACE ( 'NONE', ( #28073 ), #2866, .T. ) ;
#1627 = VECTOR ( 'NONE', #13245, 1000.000000000000000 ) ;
#1628 = ADVANCED_FACE ( 'NONE', ( #7128 ), #19463, .T. ) ;
#1629 = DIRECTION ( 'NONE',  ( -0.9510565162951536422, -2.566386769018988816E-16, -0.3090169943749472292 ) ) ;
#1630 = EDGE_CURVE ( 'NONE', #27716, #17672, #28296, .T. ) ;
#1631 = CARTESIAN_POINT ( 'NONE',  ( 142.0152310637605808, -4.999999999999979572, -26.04193191628310800 ) ) ;
#1632 = LINE ( 'NONE', #10768, #26740 ) ;
#1633 = CARTESIAN_POINT ( 'NONE',  ( 161.1922820468853388, -9.999999999999998224, -10.74328820663507678 ) ) ;
#1634 = CARTESIAN_POINT ( 'NONE',  ( 5.354491962338135735, -6.146186931204433712, -0.06809871960544290614 ) ) ;
#1635 = CARTESIAN_POINT ( 'NONE',  ( 25.76376746566330311, -3.589579415956118069, -17.31313795625071350 ) ) ;
#1636 = CARTESIAN_POINT ( 'NONE',  ( 15.33641899704135980, 5.898237403637139664, -14.35162154369138676 ) ) ;
#1637 = CARTESIAN_POINT ( 'NONE',  ( 32.63927297112797277, -9.624974391992262568, -18.12286679007055312 ) ) ;
#1638 = LINE ( 'NONE', #26993, #5641 ) ;
#1639 = CARTESIAN_POINT ( 'NONE',  ( 11.48043977940431226, 9.236673419044803879, -15.85762597608872326 ) ) ;
#1640 = LINE ( 'NONE', #10920, #10784 ) ;
#1641 = PLANE ( 'NONE',  #21233 ) ;
#1642 = CARTESIAN_POINT ( 'NONE',  ( 9.661883061612440926, 16.25482663361732705, -23.00000000000000711 ) ) ;
#1643 = CARTESIAN_POINT ( 'NONE',  ( 147.0152310637605240, -1.999999999999977573, 1.702185954127501066 ) ) ;
#1644 = ORIENTED_EDGE ( 'NONE', *, *, #5603, .F. ) ;
#1645 = FACE_BOUND ( 'NONE', #6745, .T. ) ;
#1646 = CARTESIAN_POINT ( 'NONE',  ( 12.50268541164654756, 8.571888915454989544, -15.12803469218787811 ) ) ;
#1647 = VERTEX_POINT ( 'NONE', #7281 ) ;
#1648 = CARTESIAN_POINT ( 'NONE',  ( 175.7287565553229456, -4.999999999999970690, 3.500000000000003109 ) ) ;
#1649 = CARTESIAN_POINT ( 'NONE',  ( 20.00000000000017053, 27.64101615137744972, 12.00000000000000178 ) ) ;
#1650 = CARTESIAN_POINT ( 'NONE',  ( 137.0152310637606092, -1.999999999999979572, -32.93883019725009120 ) ) ;
#1651 = CONICAL_SURFACE ( 'NONE', #6535, 4.000000000000003553, 1.047197551196597853 ) ;
#1652 = ORIENTED_EDGE ( 'NONE', *, *, #2676, .T. ) ;
#1653 = ORIENTED_EDGE ( 'NONE', *, *, #21161, .T. ) ;
#1654 = CARTESIAN_POINT ( 'NONE',  ( 8.945901566930443138, 16.94555336501101550, -17.80918358208353069 ) ) ;
#1655 = CARTESIAN_POINT ( 'NONE',  ( 32.24963562184495203, -10.43994945000269148, -19.19593526939238970 ) ) ;
#1656 = EDGE_LOOP ( 'NONE', ( #22291, #16181, #17608, #21411, #15076, #18095 ) ) ;
#1657 = CARTESIAN_POINT ( 'NONE',  ( 17.78670086218314239, 4.747145650100266678, -21.23922340053293212 ) ) ;
#1658 = CARTESIAN_POINT ( 'NONE',  ( 30.68845550234816244, -8.154108532121835395, -15.50657635367809917 ) ) ;
#1659 = CARTESIAN_POINT ( 'NONE',  ( 136.1922820468854241, -10.00000000000000533, -28.06379628232387446 ) ) ;
#1660 = CARTESIAN_POINT ( 'NONE',  ( 138.6922820468854241, -10.00000000000000533, 2.247092850131519715 ) ) ;
#1661 = EDGE_CURVE ( 'NONE', #22694, #16928, #9245, .T. ) ;
#1662 = LINE ( 'NONE', #18415, #5967 ) ;
#1663 = CARTESIAN_POINT ( 'NONE',  ( 19.79992434292498515, 0.1278105412470878222, -19.37491769885296122 ) ) ;
#1664 = ORIENTED_EDGE ( 'NONE', *, *, #12629, .T. ) ;
#1665 = EDGE_CURVE ( 'NONE', #3391, #13743, #22398, .T. ) ;
#1666 = CARTESIAN_POINT ( 'NONE',  ( -24.99999999999998934, 55.00000000000000711, 29.99999999999999289 ) ) ;
#1667 = EDGE_CURVE ( 'NONE', #9897, #3706, #23152, .T. ) ;
#1668 = CARTESIAN_POINT ( 'NONE',  ( 175.7287565553229456, -9.999999999999994671, -13.44584919360591613 ) ) ;
#1669 = CARTESIAN_POINT ( 'NONE',  ( 172.0152310637604387, -1.999999999999970024, -17.38167787843871182 ) ) ;
#1670 = VECTOR ( 'NONE', #23341, 1000.000000000000000 ) ;
#1671 = CARTESIAN_POINT ( 'NONE',  ( 13.12341270237516078, 8.570764515250925086, -15.91206798513452192 ) ) ;
#1672 = CARTESIAN_POINT ( 'NONE',  ( 33.91010249890941708, -13.82364185882242147, -18.82035036639317482 ) ) ;
#1673 = ORIENTED_EDGE ( 'NONE', *, *, #15719, .T. ) ;
#1674 = CARTESIAN_POINT ( 'NONE',  ( 12.74961974476379289, 7.623002797808662301, -14.93122222525392928 ) ) ;
#1675 = EDGE_LOOP ( 'NONE', ( #4454, #5179, #6577, #7624, #5321 ) ) ;
#1676 = CARTESIAN_POINT ( 'NONE',  ( 28.06689949639850212, -8.111051215268487269, -13.49421662364394514 ) ) ;
#1677 = CARTESIAN_POINT ( 'NONE',  ( 10.35864918915110877, 16.97212501191939538, -17.91796598306941135 ) ) ;
#1678 = LINE ( 'NONE', #8960, #7786 ) ;
#1679 = VERTEX_POINT ( 'NONE', #11535 ) ;
#1680 = ORIENTED_EDGE ( 'NONE', *, *, #15410, .T. ) ;
#1681 = DIRECTION ( 'NONE',  ( 0.5877852522924731371, 1.586114251531760728E-16, -0.8090169943749474513 ) ) ;
#1682 = CARTESIAN_POINT ( 'NONE',  ( 133.7287565553229456, -4.000000000000003553, 0.5000000000000029976 ) ) ;
#1683 = DIRECTION ( 'NONE',  ( -2.908569913943826047E-16, 1.000000000000000000, 6.826925868028084813E-18 ) ) ;
#1684 = LINE ( 'NONE', #13564, #22276 ) ;
#1685 = ORIENTED_EDGE ( 'NONE', *, *, #7603, .T. ) ;
#1686 = CARTESIAN_POINT ( 'NONE',  ( 9.661883061612440926, 16.25482663361732705, -17.94384837343789130 ) ) ;
#1687 = ADVANCED_FACE ( 'NONE', ( #20851 ), #30235, .T. ) ;
#1688 = CARTESIAN_POINT ( 'NONE',  ( 24.81022290780906658, -1.767900772465358372, -17.79475844156381470 ) ) ;
#1689 = CARTESIAN_POINT ( 'NONE',  ( 14.98730560944732559, 2.974898859484017333, -15.20016081292634169 ) ) ;
#1690 = CARTESIAN_POINT ( 'NONE',  ( 2.000000000000008882, -3.464101615137750390, -2.450000000000000622 ) ) ;
#1691 = VECTOR ( 'NONE', #10005, 1000.000000000000000 ) ;
#1692 = LINE ( 'NONE', #15707, #4010 ) ;
#1693 = CARTESIAN_POINT ( 'NONE',  ( 17.55424633453837302, 0.6138019359854992585, -14.89346452969079060 ) ) ;
#1694 = VECTOR ( 'NONE', #29059, 1000.000000000000000 ) ;
#1695 = CARTESIAN_POINT ( 'NONE',  ( 74.18800000000001660, -1.387778780781445676E-16, 5.000000000000000888 ) ) ;
#1696 = FACE_OUTER_BOUND ( 'NONE', #24882, .T. ) ;
#1697 = ORIENTED_EDGE ( 'NONE', *, *, #3987, .T. ) ;
#1698 = DIRECTION ( 'NONE',  ( -2.698458740408365879E-16, 1.000000000000000000, 0.000000000000000000 ) ) ;
#1699 = CARTESIAN_POINT ( 'NONE',  ( 32.57315965809380742, -11.03986597812349935, -18.16622079659612510 ) ) ;
#1700 = FACE_OUTER_BOUND ( 'NONE', #16788, .T. ) ;
#1701 = ORIENTED_EDGE ( 'NONE', *, *, #9372, .F. ) ;
#1702 = EDGE_LOOP ( 'NONE', ( #19013, #20985, #21361, #6119 ) ) ;
#1703 = LINE ( 'NONE', #9295, #18767 ) ;
#1704 = VECTOR ( 'NONE', #23386, 999.9999999999998863 ) ;
#1705 = CARTESIAN_POINT ( 'NONE',  ( 16.75072914628186282, 8.771658487634226731, -19.67538163746542779 ) ) ;
#1706 = CARTESIAN_POINT ( 'NONE',  ( 12.24670349824113380, 9.516721811805902931, -15.33206243003379754 ) ) ;
#1707 = CARTESIAN_POINT ( 'NONE',  ( 35.16668739017224965, -20.46881214373840763, -20.22602438870426766 ) ) ;
#1708 = ORIENTED_EDGE ( 'NONE', *, *, #13482, .T. ) ;
#1709 = CARTESIAN_POINT ( 'NONE',  ( 154.5152310637605240, -10.00000000000000000, -21.71180489736091346 ) ) ;
#1710 = CARTESIAN_POINT ( 'NONE',  ( 9.641359250860388030, 17.66885243249017634, -17.90483003768722625 ) ) ;
#1711 = LINE ( 'NONE', #8408, #3955 ) ;
#1712 = CARTESIAN_POINT ( 'NONE',  ( 130.7287565553229456, -9.999999999999982236, 3.500000000000003109 ) ) ;
#1713 = EDGE_LOOP ( 'NONE', ( #18662, #11561, #14399, #9198 ) ) ;
#1714 = B_SPLINE_CURVE_WITH_KNOTS ( 'NONE', 3,
 ( #13109, #1845, #27043, #13409, #17982, #22735 ),
 .UNSPECIFIED., .F., .F.,
 ( 4, 2, 4 ),
 ( 0.008240550023493518894, 0.01057684187039405199, 0.01291313371729458682 ),
 .UNSPECIFIED. ) ;
#1715 = CARTESIAN_POINT ( 'NONE',  ( -5.000000000000000000, 0.000000000000000000, -18.00000000000000000 ) ) ;
#1716 = ORIENTED_EDGE ( 'NONE', *, *, #30020, .F. ) ;
#1717 = CARTESIAN_POINT ( 'NONE',  ( 10.35864919943752405, 16.97212496474457311, -17.91550491156534974 ) ) ;
#1718 = ADVANCED_FACE ( 'NONE', ( #17188 ), #24069, .T. ) ;
#1719 = EDGE_CURVE ( 'NONE', #30215, #14810, #16548, .T. ) ;
#1720 = CARTESIAN_POINT ( 'NONE',  ( 36.54859390953724585, -21.18451583373416014, -16.94733705004010105 ) ) ;
#1721 = CARTESIAN_POINT ( 'NONE',  ( 25.31619048431776875, -0.2099727537683927225, -15.56338435260822628 ) ) ;
#1722 = ORIENTED_EDGE ( 'NONE', *, *, #27731, .T. ) ;
#1723 = EDGE_CURVE ( 'NONE', #26303, #5191, #22214, .T. ) ;
#1724 = ORIENTED_EDGE ( 'NONE', *, *, #2251, .F. ) ;
#1725 = CARTESIAN_POINT ( 'NONE',  ( 127.7287565553229740, -1.999999999999982681, 0.5000000000000115463 ) ) ;
#1726 = CARTESIAN_POINT ( 'NONE',  ( 118.5123031260608286, -4.999999999999985789, -86.10422831294586388 ) ) ;
#1727 = CARTESIAN_POINT ( 'NONE',  ( 166.1922820468853672, -1.999999999999971356, -30.91696583120936026 ) ) ;
#1728 = ORIENTED_EDGE ( 'NONE', *, *, #12623, .T. ) ;
#1729 =( LENGTH_UNIT ( ) NAMED_UNIT ( * ) SI_UNIT ( .MILLI., .METRE. ) );
#1730 = CARTESIAN_POINT ( 'NONE',  ( 25.71810023473615203, -5.953606672203104466, -12.71518937071605038 ) ) ;
#1731 = CARTESIAN_POINT ( 'NONE',  ( 26.19520757255249066, -7.109971961106261951, -13.37903969216112898 ) ) ;
#1732 = VECTOR ( 'NONE', #11918, 1000.000000000000000 ) ;
#1733 = ORIENTED_EDGE ( 'NONE', *, *, #15202, .F. ) ;
#1734 = LINE ( 'NONE', #20322, #4017 ) ;
#1735 = FACE_OUTER_BOUND ( 'NONE', #26670, .T. ) ;
#1736 = CARTESIAN_POINT ( 'NONE',  ( 0.000000000000000000, 0.000000000000000000, 0.000000000000000000 ) ) ;
#1737 = DIRECTION ( 'NONE',  ( -2.698458740408365879E-16, 1.000000000000000000, 0.000000000000000000 ) ) ;
#1738 = LINE ( 'NONE', #20328, #16512 ) ;
#1739 = CARTESIAN_POINT ( 'NONE',  ( 84.45309523925811845, -4.999999999999994671, 61.35876531300809944 ) ) ;
#1740 = CARTESIAN_POINT ( 'NONE',  ( 13.24589568141979612, 7.574869496316740225, -15.81383618087551746 ) ) ;
#1741 = CARTESIAN_POINT ( 'NONE',  ( 12.50076791318051761, 8.571041463825640250, -15.12956297801270900 ) ) ;
#1742 = CARTESIAN_POINT ( 'NONE',  ( 26.46413748225140594, -13.10274310649288942, -15.24000415025259692 ) ) ;
#1743 = ORIENTED_EDGE ( 'NONE', *, *, #23303, .T. ) ;
#1744 = FACE_OUTER_BOUND ( 'NONE', #6476, .T. ) ;
#1745 = CARTESIAN_POINT ( 'NONE',  ( 2.698458740408370316E-15, -10.00000000000001776, 0.000000000000000000 ) ) ;
#1746 = VERTEX_POINT ( 'NONE', #19762 ) ;
#1747 = CARTESIAN_POINT ( 'NONE',  ( 9.675370519060759733, 17.51287242109451014, -17.23928541814325399 ) ) ;
#1748 = VECTOR ( 'NONE', #8922, 1000.000000000000000 ) ;
#1749 = CARTESIAN_POINT ( 'NONE',  ( 175.7287565553229456, -9.999999999999994671, -22.10610323145030520 ) ) ;
#1750 = DIRECTION ( 'NONE',  ( -2.698458740408365879E-16, 1.000000000000000000, 0.000000000000000000 ) ) ;
#1751 = CARTESIAN_POINT ( 'NONE',  ( 172.0152310637603819, -1.999999999999970912, -0.06116980274991495881 ) ) ;
#1753 = VERTEX_POINT ( 'NONE', #28677 ) ;
#1752 = CARTESIAN_POINT ( 'NONE',  ( 21.42923412144385509, -1.598955984811285536, -13.33006947543598741 ) ) ;
#1754 = VERTEX_POINT ( 'NONE', #26673 ) ;
#1755 = CARTESIAN_POINT ( 'NONE',  ( 174.7287565553228887, -1.999999999999969358, -16.50000000000000355 ) ) ;
#1756 = CARTESIAN_POINT ( 'NONE',  ( 11.05541531668977662, 17.68942339022145305, -17.92279151347708677 ) ) ;
#1757 = EDGE_CURVE ( 'NONE', #24463, #26115, #12750, .T. ) ;
#1758 = CARTESIAN_POINT ( 'NONE',  ( 33.38708106686501509, -12.47399286361455850, -19.70456970583452616 ) ) ;
#1759 = CARTESIAN_POINT ( 'NONE',  ( 132.2287565553230024, -4.999999999999982236, -12.16987298107780013 ) ) ;
#1760 = ORIENTED_EDGE ( 'NONE', *, *, #27900, .F. ) ;
#1761 = EDGE_CURVE ( 'NONE', #1908, #20048, #5901, .T. ) ;
#1762 = EDGE_CURVE ( 'NONE', #930, #1338, #12665, .T. ) ;
#1763 = CARTESIAN_POINT ( 'NONE',  ( 25.67262840375075328, -3.322766148301121714, -14.04542551033457798 ) ) ;
#1764 = CARTESIAN_POINT ( 'NONE',  ( 420.0000000000002274, 34.64101615137744972, 10.00000000000000178 ) ) ;
#1765 = ADVANCED_FACE ( 'NONE', ( #26366 ), #18502, .T. ) ;
#1766 = CARTESIAN_POINT ( 'NONE',  ( 24.12901349891383163, -0.6887463444711696692, -16.28517635256633156 ) ) ;
#1767 = ORIENTED_EDGE ( 'NONE', *, *, #11879, .T. ) ;
#1768 = CARTESIAN_POINT ( 'NONE',  ( 162.0152310637604387, -1.999999999999973577, 1.702185954127501066 ) ) ;
#1769 = VECTOR ( 'NONE', #19625, 1000.000000000000000 ) ;
#1770 = CARTESIAN_POINT ( 'NONE',  ( 26.55441479597953247, -12.51626325376082249, -18.99724541349076645 ) ) ;
#1771 = CARTESIAN_POINT ( 'NONE',  ( 29.20193236150002392, -6.731655735042891386, -17.98962132073140552 ) ) ;
#1772 = AXIS2_PLACEMENT_3D ( 'NONE', #8490, #29625, #19942 ) ;
#1773 = ORIENTED_EDGE ( 'NONE', *, *, #21581, .T. ) ;
#1774 = FACE_OUTER_BOUND ( 'NONE', #29876, .T. ) ;
#1775 = VECTOR ( 'NONE', #13954, 1000.000000000000000 ) ;
#1776 = VECTOR ( 'NONE', #11033, 1000.000000000000000 ) ;
#1777 = CARTESIAN_POINT ( 'NONE',  ( 168.6922820468853956, -4.999999999999971578, -35.24709285013155835 ) ) ;
#1778 = LINE ( 'NONE', #1932, #23891 ) ;
#1779 = VECTOR ( 'NONE', #26176, 1000.000000000000000 ) ;
#1780 = DIRECTION ( 'NONE',  ( 1.110223024625156540E-16, 2.995891024602366092E-32, 1.000000000000000000 ) ) ;
#1781 = CARTESIAN_POINT ( 'NONE',  ( 102.9952437281683757, -4.999999999999989342, -74.83042475079173528 ) ) ;
#1782 = CARTESIAN_POINT ( 'NONE',  ( 9.641350810849047548, 17.66889113945805789, -19.66666666666842644 ) ) ;
#1783 = CARTESIAN_POINT ( 'NONE',  ( 23.18962843369624949, -6.128656054388458507, -17.19981796389819095 ) ) ;
#1784 = CARTESIAN_POINT ( 'NONE',  ( 18.54205238286641588, 5.219565156008159512, -20.23764637224795848 ) ) ;
#1785 = CARTESIAN_POINT ( 'NONE',  ( 35.88008189734257769, -20.18124548360443882, -21.42481968387543390 ) ) ;
#1786 = DIRECTION ( 'NONE',  ( 0.5877852522924731371, 1.586114251531760728E-16, -0.8090169943749474513 ) ) ;
#1787 = CARTESIAN_POINT ( 'NONE',  ( 11.46471852075427478, 9.306694396509932687, -15.86428581073749378 ) ) ;
#1788 = CARTESIAN_POINT ( 'NONE',  ( 149.7287565553230024, -4.999999999999976907, -16.50000000000000000 ) ) ;
#1789 = CARTESIAN_POINT ( 'NONE',  ( 138.6922820468854525, -1.999999999999979572, -35.24709285013155835 ) ) ;
#1790 = CARTESIAN_POINT ( 'NONE',  ( 9.667746079407143256, 16.22793808664985704, -17.88513208046981617 ) ) ;
#1791 = DIRECTION ( 'NONE',  ( -0.000000000000000000, 1.000000000000000000, -0.000000000000000000 ) ) ;
#1792 = ORIENTED_EDGE ( 'NONE', *, *, #30164, .T. ) ;
#1793 = CARTESIAN_POINT ( 'NONE',  ( 102.3970440912936795, -4.999999999999989342, 74.39580727436489838 ) ) ;
#1794 = CARTESIAN_POINT ( 'NONE',  ( 12.50162201464318557, 8.571418981294288031, -15.12888223836978341 ) ) ;
#1795 = EDGE_LOOP ( 'NONE', ( #21831, #6319, #22373, #27502 ) ) ;
#1796 = VECTOR ( 'NONE', #6285, 1000.000000000000000 ) ;
#1797 = CARTESIAN_POINT ( 'NONE',  ( 99.72270124223099685, -4.999999999999990230, -72.45278346005385117 ) ) ;
#1798 = DIRECTION ( 'NONE',  ( -2.698458740408365879E-16, 1.000000000000000000, 0.000000000000000000 ) ) ;
#1799 = ORIENTED_EDGE ( 'NONE', *, *, #17707, .F. ) ;
#1800 = ADVANCED_FACE ( 'NONE', ( #12441 ), #1322, .T. ) ;
#1801 = VECTOR ( 'NONE', #14004, 1000.000000000000000 ) ;
#1802 = PLANE ( 'NONE',  #16117 ) ;
#1803 = EDGE_CURVE ( 'NONE', #24538, #8805, #5361, .T. ) ;
#1804 = EDGE_CURVE ( 'NONE', #8129, #28570, #17479, .T. ) ;
#1805 = ORIENTED_EDGE ( 'NONE', *, *, #411, .T. ) ;
#1806 = EDGE_CURVE ( 'NONE', #14013, #17474, #10613, .T. ) ;
#1807 = CARTESIAN_POINT ( 'NONE',  ( 13.38138208201938895, 7.626735917299793499, -15.70646184538344770 ) ) ;
#1808 = CARTESIAN_POINT ( 'NONE',  ( 35.47777500975636400, -18.37389374556380517, -21.30860247919107664 ) ) ;
#1809 = B_SPLINE_CURVE_WITH_KNOTS ( 'NONE', 3,
 ( #27957, #21045, #149, #11329 ),
 .UNSPECIFIED., .F., .F.,
 ( 4, 4 ),
 ( 2.380737581964344716E-07, 0.002336974151641508721 ),
 .UNSPECIFIED. ) ;
#1810 = CARTESIAN_POINT ( 'NONE',  ( 22.56790106455553868, 4.272635385308135803, -18.10442882813315535 ) ) ;
#1811 = CARTESIAN_POINT ( 'NONE',  ( 17.46640274557904959, 4.060524459741898795, -18.82505950134852313 ) ) ;
#1812 = CARTESIAN_POINT ( 'NONE',  ( -24.99999999999998934, 55.00000000000000711, 24.99999999999998934 ) ) ;
#1813 = CARTESIAN_POINT ( 'NONE',  ( 416.0000000000002274, 34.64101615137744972, 10.00000000000000178 ) ) ;
#1814 = CARTESIAN_POINT ( 'NONE',  ( 27.77130384954419995, -2.130748013457071099, -15.99611347415175366 ) ) ;
#1815 = VECTOR ( 'NONE', #20958, 1000.000000000000000 ) ;
#1816 = ORIENTED_EDGE ( 'NONE', *, *, #26363, .T. ) ;
#1817 = CARTESIAN_POINT ( 'NONE',  ( 20.06118759710066968, -5.000000000000012434, -61.74198680378115967 ) ) ;
#1819 = ORIENTED_EDGE ( 'NONE', *, *, #20781, .T. ) ;
#1818 = CARTESIAN_POINT ( 'NONE',  ( 172.0152310637604387, -9.999999999999994671, -17.38167787843871182 ) ) ;
#1820 = VECTOR ( 'NONE', #18891, 1000.000000000000000 ) ;
#1821 = CARTESIAN_POINT ( 'NONE',  ( 157.0152310637605524, -9.999999999999998224, -24.27857615940569502 ) ) ;
#1823 = CARTESIAN_POINT ( 'NONE',  ( 138.6922820468854525, -1.999999999999979572, -6.413161187712876909 ) ) ;
#1822 = AXIS2_PLACEMENT_3D ( 'NONE', #4692, #24755, #24596 ) ;
#1824 = DIRECTION ( 'NONE',  ( -2.698458740408365879E-16, 1.000000000000000000, 0.000000000000000000 ) ) ;
#1825 = CARTESIAN_POINT ( 'NONE',  ( 33.92041909680281719, -11.11917911243856238, -17.74043268107170235 ) ) ;
#1826 = VECTOR ( 'NONE', #28497, 1000.000000000000000 ) ;
#1827 = ORIENTED_EDGE ( 'NONE', *, *, #10230, .F. ) ;
#1828 = CARTESIAN_POINT ( 'NONE',  ( 10.67240773364005868, 9.027839897374207112, -16.40964036978800777 ) ) ;
#1829 = VERTEX_POINT ( 'NONE', #5594 ) ;
#1830 = CARTESIAN_POINT ( 'NONE',  ( 31.59793210864275537, -10.01186915388335485, -14.42687813506083039 ) ) ;
#1831 = CARTESIAN_POINT ( 'NONE',  ( 172.7287565553229456, -1.999999999999970468, -39.49999999999997158 ) ) ;
#1832 = CARTESIAN_POINT ( 'NONE',  ( 10.35864940629342890, 16.97212401607702148, -17.91464645457531191 ) ) ;
#1833 = FACE_BOUND ( 'NONE', #13395, .T. ) ;
#1834 = ORIENTED_EDGE ( 'NONE', *, *, #1278, .F. ) ;
#1835 = MANIFOLD_SOLID_BREP ( 'EndChamfer', #26307 ) ;
#1836 = CARTESIAN_POINT ( 'NONE',  ( 167.0152310637604955, -1.999999999999971356, -15.61832212156129707 ) ) ;
#1837 = EDGE_CURVE ( 'NONE', #23534, #6999, #8618, .T. ) ;
#1838 = AXIS2_PLACEMENT_3D ( 'NONE', #8257, #5982, #8108 ) ;
#1839 = DIRECTION ( 'NONE',  ( -1.000000000000000000, -4.440892098500622217E-16, 0.000000000000000000 ) ) ;
#1841 = ORIENTED_EDGE ( 'NONE', *, *, #2900, .T. ) ;
#1840 = CARTESIAN_POINT ( 'NONE',  ( 163.6922820468853672, -9.999999999999998224, -23.73366926340167637 ) ) ;
#1842 = ORIENTED_EDGE ( 'NONE', *, *, #27520, .T. ) ;
#1843 = VERTEX_POINT ( 'NONE', #5292 ) ;
#1844 = ADVANCED_FACE ( 'NONE', ( #18082 ), #13209, .T. ) ;
#1845 = CARTESIAN_POINT ( 'NONE',  ( -7.999999999999996447, -3.867591403079199353, -0.4976753153245889738 ) ) ;
#1846 = ORIENTED_EDGE ( 'NONE', *, *, #20071, .F. ) ;
#1847 = EDGE_CURVE ( 'NONE', #1403, #28891, #27443, .T. ) ;
#1848 = CARTESIAN_POINT ( 'NONE',  ( 13.12048998592846871, 8.569482736746577345, -15.91439669260688561 ) ) ;
#1849 = EDGE_LOOP ( 'NONE', ( #23058, #3665, #6405, #3848 ) ) ;
#1850 = VECTOR ( 'NONE', #8309, 1000.000000000000000 ) ;
#1851 = CARTESIAN_POINT ( 'NONE',  ( 24.88259999727891625, -1.109419405293186944, -15.69091174474707451 ) ) ;
#1852 = CARTESIAN_POINT ( 'NONE',  ( 16.98604603105943767, -0.4850832133139416080, -17.48051239862526884 ) ) ;
#1853 = CARTESIAN_POINT ( 'NONE',  ( 13.86827785273622737, 5.312354197023893221, -16.63408457058017120 ) ) ;
#1854 = DIRECTION ( 'NONE',  ( 0.000000000000000000, -2.775557561562890735E-17, 1.000000000000000000 ) ) ;
#1855 = DIRECTION ( 'NONE',  ( -2.698458740408365879E-16, 1.000000000000000000, 0.000000000000000000 ) ) ;
#1856 = VECTOR ( 'NONE', #11459, 1000.000000000000000 ) ;
#1857 = CARTESIAN_POINT ( 'NONE',  ( 21.10023079691774228, -0.4353598523292347422, -20.14113737667230097 ) ) ;
#1858 = CARTESIAN_POINT ( 'NONE',  ( 0.000000000000000000, 0.000000000000000000, 4.999999999999997335 ) ) ;
#1859 = DIRECTION ( 'NONE',  ( 1.000000000000000000, 0.000000000000000000, 0.000000000000000000 ) ) ;
#1860 = AXIS2_PLACEMENT_3D ( 'NONE', #26887, #14779, #26725 ) ;
#1861 = ORIENTED_EDGE ( 'NONE', *, *, #15291, .T. ) ;
#1862 = ADVANCED_FACE ( 'NONE', ( #6043 ), #11358, .T. ) ;
#1863 = CARTESIAN_POINT ( 'NONE',  ( 10.35864918915111055, 16.97212501191939182, -23.00000000000000711 ) ) ;
#1864 = CARTESIAN_POINT ( 'NONE',  ( 32.30218501430429967, -10.99871056796995816, -17.40035725849610060 ) ) ;
#1865 = DIRECTION ( 'NONE',  ( 0.5877852522924731371, 0.000000000000000000, 0.8090169943749474513 ) ) ;
#1866 = VECTOR ( 'NONE', #5960, 1000.000000000000000 ) ;
#1867 = EDGE_LOOP ( 'NONE', ( #10814, #20642 ) ) ;
#1868 = FACE_OUTER_BOUND ( 'NONE', #6254, .T. ) ;
#1869 = CARTESIAN_POINT ( 'NONE',  ( 14.57776618122778700, 6.338444840345393239, -15.85465340776532095 ) ) ;
#1870 = CARTESIAN_POINT ( 'NONE',  ( 12.25874535991881764, 9.522117202545773651, -15.32245921924925902 ) ) ;
#1871 = CARTESIAN_POINT ( 'NONE',  ( 35.12509383387676820, -20.28195432802065312, -20.22992657050740917 ) ) ;
#1872 = ORIENTED_EDGE ( 'NONE', *, *, #19852, .F. ) ;
#1873 = DIRECTION ( 'NONE',  ( -1.110223024625156540E-16, 0.000000000000000000, -1.000000000000000000 ) ) ;
#1874 = CARTESIAN_POINT ( 'NONE',  ( 12.75639466810640776, 7.625977817552541005, -14.92582393630036108 ) ) ;
#1875 = LINE ( 'NONE', #13882, #16600 ) ;
#1876 = SURFACE_SIDE_STYLE ('',( #27386 ) ) ;
#1877 = DIRECTION ( 'NONE',  ( -0.8090169943749474513, -2.183098979609982436E-16, 0.5877852522924731371 ) ) ;
#1878 = VERTEX_POINT ( 'NONE', #10910 ) ;
#1879 = CARTESIAN_POINT ( 'NONE',  ( 12.86836073382838563, 9.516082146233362238, -16.11534891376273748 ) ) ;
#1880 = CARTESIAN_POINT ( 'NONE',  ( 36.54859390953724585, -21.18451583373416014, -18.19919658220850422 ) ) ;
#1881 = CARTESIAN_POINT ( 'NONE',  ( 24.52797215547132836, -1.897736678990579184, -19.26084780660264073 ) ) ;
#1882 = ORIENTED_EDGE ( 'NONE', *, *, #18338, .T. ) ;
#1883 = AXIS2_PLACEMENT_3D ( 'NONE', #9929, #16804, #25983 ) ;
#1884 = LINE ( 'NONE', #30151, #4283 ) ;
#1885 = DIRECTION ( 'NONE',  ( -0.9510565162951536422, -2.566386769018988816E-16, -0.3090169943749472292 ) ) ;
#1886 = SHAPE_REPRESENTATION_RELATIONSHIP ( 'NONE' , 'NONE' ,  #6235, #6562 ) ;
#1887 = CARTESIAN_POINT ( 'NONE',  ( 23.43951749033787735, -6.062008688038916127, -19.28752554440484701 ) ) ;
#1888 = AXIS2_PLACEMENT_3D ( 'NONE', #23992, #18290, #13572 ) ;
#1889 = CARTESIAN_POINT ( 'NONE',  ( 21.35588827150667512, -4.635113535248831518, -19.58358080364444476 ) ) ;
#1890 = VERTEX_POINT ( 'NONE', #24976 ) ;
#1891 = DIRECTION ( 'NONE',  ( -0.9510565162951536422, -2.566386769018988816E-16, -0.3090169943749472292 ) ) ;
#1892 = EDGE_CURVE ( 'NONE', #2137, #10985, #13501, .T. ) ;
#1893 = LINE ( 'NONE', #13314, #9588 ) ;
#1894 = CYLINDRICAL_SURFACE ( 'NONE', #2902, 2.500000000000000888 ) ;
#1895 = EDGE_CURVE ( 'NONE', #5625, #4687, #13652, .T. ) ;
#1896 = DIRECTION ( 'NONE',  ( -2.698458740408365879E-16, 1.000000000000000000, 0.000000000000000000 ) ) ;
#1897 = UNCERTAINTY_MEASURE_WITH_UNIT (LENGTH_MEASURE( 1.000000000000000082E-05 ), #9281, 'distance_accuracy_value', 'NONE');
#1898 = CARTESIAN_POINT ( 'NONE',  ( 12.44984726620633353, 8.550925603015029353, -15.16996558791898231 ) ) ;
#1899 = LINE ( 'NONE', #3878, #27335 ) ;
#1900 = EDGE_LOOP ( 'NONE', ( #16044, #14481, #10590, #25713, #21287 ) ) ;
#1901 = VECTOR ( 'NONE', #29105, 1000.000000000000000 ) ;
#1902 = CARTESIAN_POINT ( 'NONE',  ( 161.1922820468853672, -9.999999999999998224, -22.25671179336496053 ) ) ;
#1903 = ORIENTED_EDGE ( 'NONE', *, *, #17786, .F. ) ;
#1904 = CARTESIAN_POINT ( 'NONE',  ( 9.641350810849047548, 17.66889113945805789, -17.94384837343789485 ) ) ;
#1905 = CARTESIAN_POINT ( 'NONE',  ( 29.62334656761623819, -11.49549692320935890, -13.92735753183835712 ) ) ;
#1906 = DIRECTION ( 'NONE',  ( -1.110223024625156540E-16, 0.000000000000000000, -1.000000000000000000 ) ) ;
#1907 = CARTESIAN_POINT ( 'NONE',  ( 177.2287565553228603, -1.999999999999968914, -12.16987298107780369 ) ) ;
#1908 = VERTEX_POINT ( 'NONE', #1631 ) ;
#1910 = ORIENTED_EDGE ( 'NONE', *, *, #374, .F. ) ;
#1909 = CARTESIAN_POINT ( 'NONE',  ( 22.86252235622482587, -0.9498377794471745128, -13.29674124224850118 ) ) ;
#1911 = AXIS2_PLACEMENT_3D ( 'NONE', #5698, #17283, #13004 ) ;
#1912 = ORIENTED_EDGE ( 'NONE', *, *, #7771, .F. ) ;
#1913 = LINE ( 'NONE', #18061, #14911 ) ;
#1914 = CARTESIAN_POINT ( 'NONE',  ( 11.05541531668977662, 17.68942339022145305, -17.91796598306941135 ) ) ;
#1915 = CARTESIAN_POINT ( 'NONE',  ( 35.54859390953724585, -22.18451583373416014, -17.78191007148576475 ) ) ;
#1916 = CARTESIAN_POINT ( 'NONE',  ( -4.000000000000004441, -0.3902508023145583871, -2.693564772268675078E-15 ) ) ;
#1917 = CARTESIAN_POINT ( 'NONE',  ( 21.54098841764929873, -5.100688324319140321, -15.19385678519978633 ) ) ;
#1918 = DIRECTION ( 'NONE',  ( -0.8090169943749474513, -2.183098979609982436E-16, 0.5877852522924731371 ) ) ;
#1919 = CARTESIAN_POINT ( 'NONE',  ( 20.43449928165676965, -1.849542096390112356, -17.64764676960594869 ) ) ;
#1920 = ORIENTED_EDGE ( 'NONE', *, *, #3574, .F. ) ;
#1921 = CARTESIAN_POINT ( 'NONE',  ( -19.99999999999998934, 60.00000000000000711, 29.99999999999999289 ) ) ;
#1922 = PRESENTATION_STYLE_ASSIGNMENT (( #22522 ) ) ;
#1923 = CARTESIAN_POINT ( 'NONE',  ( 16.22940209442605308, 10.22534693890197133, -14.12725775589269084 ) ) ;
#1924 = CARTESIAN_POINT ( 'NONE',  ( 28.05683000375443825, -12.20169833507544865, -14.26034257730772126 ) ) ;
#1925 = EDGE_LOOP ( 'NONE', ( #19693, #19949, #3167, #6636 ) ) ;
#1926 = LINE ( 'NONE', #25107, #26864 ) ;
#1927 = VECTOR ( 'NONE', #25831, 1000.000000000000000 ) ;
#1928 = LINE ( 'NONE', #13648, #29476 ) ;
#1929 = VECTOR ( 'NONE', #5267, 1000.000000000000000 ) ;
#1930 = ADVANCED_FACE ( 'NONE', ( #1478 ), #15938, .T. ) ;
#1931 = EDGE_CURVE ( 'NONE', #16946, #18592, #17773, .T. ) ;
#1932 = CARTESIAN_POINT ( 'NONE',  ( 154.7287565553230309, -10.00000000000000000, -33.82050807568879947 ) ) ;
#1933 = DIRECTION ( 'NONE',  ( 0.000000000000000000, 0.000000000000000000, 1.000000000000000000 ) ) ;
#1934 = ADVANCED_FACE ( 'NONE', ( #13353 ), #25265, .T. ) ;
#1935 = DIRECTION ( 'NONE',  ( -2.698458740408365879E-16, 1.000000000000000000, 0.000000000000000000 ) ) ;
#1936 = EDGE_CURVE ( 'NONE', #13441, #25891, #3908, .T. ) ;
#1937 = CARTESIAN_POINT ( 'NONE',  ( 15.00000000000000000, 0.000000000000000000, 0.000000000000000000 ) ) ;
#1938 = CARTESIAN_POINT ( 'NONE',  ( 24.36960067559809318, -5.041758482997499513, -18.26785210147486538 ) ) ;
#1939 = CARTESIAN_POINT ( 'NONE',  ( 18.51594006248351931, 7.284897756227690202, -14.24483590514913089 ) ) ;
#1940 = CARTESIAN_POINT ( 'NONE',  ( 32.09732368354767118, -9.542663571685382706, -16.59113971387166941 ) ) ;
#1941 = FACE_OUTER_BOUND ( 'NONE', #14215, .T. ) ;
#1942 = CARTESIAN_POINT ( 'NONE',  ( 12.13006862794127017, 8.527244997094612700, -15.41586291625151972 ) ) ;
#1943 = CARTESIAN_POINT ( 'NONE',  ( 5.200000000000002842, 0.000000000000000000, -2.700000000000001066 ) ) ;
#1944 = CARTESIAN_POINT ( 'NONE',  ( 147.0152310637606092, -4.999999999999978684, -32.93883019725009120 ) ) ;
#1945 = CARTESIAN_POINT ( 'NONE',  ( 9.667069921042207525, 16.23103903510144619, -17.88562738470040969 ) ) ;
#1946 = DIRECTION ( 'NONE',  ( -2.698458740408365879E-16, 1.000000000000000000, 0.000000000000000000 ) ) ;
#1947 = ORIENTED_EDGE ( 'NONE', *, *, #27396, .T. ) ;
#1948 = LINE ( 'NONE', #22847, #301 ) ;
#1949 = CARTESIAN_POINT ( 'NONE',  ( 12.44984726620633353, 8.550925603015029353, -15.16996558791898231 ) ) ;
#1950 = ORIENTED_EDGE ( 'NONE', *, *, #16125, .T. ) ;
#1951 = CONICAL_SURFACE ( 'NONE', #13612, 2.041999999999999815, 1.047197551196591858 ) ;
#1952 = LINE ( 'NONE', #1797, #4214 ) ;
#1953 = DIRECTION ( 'NONE',  ( -0.9510565162951536422, -2.566386769018988816E-16, -0.3090169943749472292 ) ) ;
#1954 = DIRECTION ( 'NONE',  ( -0.5877852522924731371, 0.000000000000000000, 0.8090169943749474513 ) ) ;
#1955 = VERTEX_POINT ( 'NONE', #8765 ) ;
#1956 = CARTESIAN_POINT ( 'NONE',  ( 9.112356771736518368, 16.18216857766665484, -17.05479705382001399 ) ) ;
#1957 = CARTESIAN_POINT ( 'NONE',  ( 34.79556486487921774, -19.80155522666461465, -21.17264749384332134 ) ) ;
#1958 = EDGE_LOOP ( 'NONE', ( #9691, #6511, #3022, #19742 ) ) ;
#1959 = CARTESIAN_POINT ( 'NONE',  ( 17.27385296224481337, 7.553222137591894203, -13.16260341916398069 ) ) ;
#1960 = CARTESIAN_POINT ( 'NONE',  ( 27.03191753302054323, -12.88672130028117735, -14.08881772908025454 ) ) ;
#1961 = LINE ( 'NONE', #11243, #13754 ) ;
#1962 = CARTESIAN_POINT ( 'NONE',  ( 23.51547714073238282, 0.8170344765809651744, -13.87895193235286051 ) ) ;
#1963 = VERTEX_POINT ( 'NONE', #15329 ) ;
#1964 = LINE ( 'NONE', #4538, #25018 ) ;
#1965 =( GEOMETRIC_REPRESENTATION_CONTEXT ( 3 ) GLOBAL_UNCERTAINTY_ASSIGNED_CONTEXT ( ( #18347 ) ) GLOBAL_UNIT_ASSIGNED_CONTEXT ( ( #28940, #29705, #22935 ) ) REPRESENTATION_CONTEXT ( 'NONE', 'WORKASPACE' ) );
#1966 = AXIS2_PLACEMENT_3D ( 'NONE', #3469, #17641, #10319 ) ;
#1968 = EDGE_LOOP ( 'NONE', ( #25207, #6076, #3223, #29181, #3649 ) ) ;
#1967 = DIRECTION ( 'NONE',  ( -2.698458740408365879E-16, 1.000000000000000000, 0.000000000000000000 ) ) ;
#1969 = EDGE_CURVE ( 'NONE', #2119, #17207, #1778, .T. ) ;
#1970 = DIRECTION ( 'NONE',  ( -0.9510565162951536422, 0.000000000000000000, -0.3090169943749472292 ) ) ;
#1971 = EDGE_CURVE ( 'NONE', #1843, #11751, #20218, .T. ) ;
#1972 = ADVANCED_FACE ( 'NONE', ( #2081 ), #11215, .T. ) ;
#1973 = AXIS2_PLACEMENT_3D ( 'NONE', #5298, #14430, #4989 ) ;
#1974 = VECTOR ( 'NONE', #15489, 1000.000000000000000 ) ;
#1975 = EDGE_CURVE ( 'NONE', #22500, #6950, #4205, .T. ) ;
#1976 = LINE ( 'NONE', #8950, #16082 ) ;
#1977 = CARTESIAN_POINT ( 'NONE',  ( 34.22536682013040377, -11.37642754387024979, -18.47965768629886085 ) ) ;
#1978 = ORIENTED_EDGE ( 'NONE', *, *, #5256, .T. ) ;
#1979 = CARTESIAN_POINT ( 'NONE',  ( 12.33231149932895221, 7.515762311178675326, -15.25793818847554562 ) ) ;
#1980 = ORIENTED_EDGE ( 'NONE', *, *, #3782, .F. ) ;
#1981 = CARTESIAN_POINT ( 'NONE',  ( 24.60501232743784783, -9.531698448777172317, -16.22453333552994792 ) ) ;
#1982 = CARTESIAN_POINT ( 'NONE',  ( -17.25000000000017053, 34.64101615137744972, 0.000000000000000000 ) ) ;
#1983 = CARTESIAN_POINT ( 'NONE',  ( 10.46247360472336041, 16.49597300757040230, -17.34042816522791952 ) ) ;
#1984 = LINE ( 'NONE', #11265, #20453 ) ;
#1985 = DIRECTION ( 'NONE',  ( 0.000000000000000000, -1.000000000000000000, 0.000000000000000000 ) ) ;
#1986 = VECTOR ( 'NONE', #25170, 1000.000000000000000 ) ;
#1987 = VERTEX_POINT ( 'NONE', #29604 ) ;
#1988 = CARTESIAN_POINT ( 'NONE',  ( 8.469702402841419307E-15, 55.00000000000000711, 12.49999999999999112 ) ) ;
#1989 = CARTESIAN_POINT ( 'NONE',  ( 12.50098444160134470, 8.571137227758441668, -15.12939039523150520 ) ) ;
#1991 = ORIENTED_EDGE ( 'NONE', *, *, #23209, .F. ) ;
#1990 = FACE_OUTER_BOUND ( 'NONE', #824, .T. ) ;
#1992 = CARTESIAN_POINT ( 'NONE',  ( 131.1922820468854241, -1.999999999999982236, -22.25671179336495697 ) ) ;
#1993 = ORIENTED_EDGE ( 'NONE', *, *, #1723, .F. ) ;
#1994 = CARTESIAN_POINT ( 'NONE',  ( 9.661883061612440926, 16.25482663361732705, -17.93331994345748726 ) ) ;
#1995 = VECTOR ( 'NONE', #18610, 999.9999999999998863 ) ;
#1996 = CARTESIAN_POINT ( 'NONE',  ( 20.60316120045176902, -2.756227665500133206, -14.85995437523845553 ) ) ;
#1997 = CARTESIAN_POINT ( 'NONE',  ( 24.59799960276797393, -1.134526835705675918, -15.12159415400816975 ) ) ;
#1998 = CARTESIAN_POINT ( 'NONE',  ( 21.58357356133149807, 4.347441036859617469, -17.91576365920758107 ) ) ;
#1999 = CARTESIAN_POINT ( 'NONE',  ( 20.69654234312579533, -5.000000000000012434, -63.69740764588885185 ) ) ;
#2000 = LINE ( 'NONE', #27804, #20081 ) ;
#2001 = CARTESIAN_POINT ( 'NONE',  ( 19.02541433733466647, 1.263421280649871248, -13.57496312174407826 ) ) ;
#2002 = EDGE_LOOP ( 'NONE', ( #27202, #19220, #18719, #5417 ) ) ;
#2003 = DIRECTION ( 'NONE',  ( -1.000000000000000000, -4.440892098500622217E-16, 0.000000000000000000 ) ) ;
#2004 = VECTOR ( 'NONE', #19632, 1000.000000000000000 ) ;
#2005 = DIRECTION ( 'NONE',  ( -0.000000000000000000, -0.000000000000000000, -1.000000000000000000 ) ) ;
#2006 = AXIS2_PLACEMENT_3D ( 'NONE', #8999, #16029, #4889 ) ;
#2007 = EDGE_CURVE ( 'NONE', #26011, #21590, #27297, .T. ) ;
#2008 = EDGE_CURVE ( 'NONE', #20426, #28522, #15644, .T. ) ;
#2009 = EDGE_CURVE ( 'NONE', #17052, #16407, #4953, .T. ) ;
#2010 = CARTESIAN_POINT ( 'NONE',  ( 10.35864953657871190, 16.97212341857210660, -17.91436492910080247 ) ) ;
#2011 = DIRECTION ( 'NONE',  ( 0.000000000000000000, -2.775557561562890735E-17, 1.000000000000000000 ) ) ;
#2012 = LINE ( 'NONE', #16170, #2927 ) ;
#2013 = ORIENTED_EDGE ( 'NONE', *, *, #28246, .T. ) ;
#2014 = ORIENTED_EDGE ( 'NONE', *, *, #6086, .T. ) ;
#2015 = LINE ( 'NONE', #6578, #23655 ) ;
#2016 = CARTESIAN_POINT ( 'NONE',  ( 14.29829396236512729, 6.476847147513518088, -18.28004444394726491 ) ) ;
#2017 = CARTESIAN_POINT ( 'NONE',  ( 11.05610776857519184, 17.68624771760786274, -17.82814161748832760 ) ) ;
#2018 = CARTESIAN_POINT ( 'NONE',  ( 35.22227017426903473, -20.71851614966110233, -20.19360243392694088 ) ) ;
#2019 = ORIENTED_EDGE ( 'NONE', *, *, #9336, .F. ) ;
#2020 = DIRECTION ( 'NONE',  ( 1.000000000000000000, 0.000000000000000000, 0.000000000000000000 ) ) ;
#2021 = CARTESIAN_POINT ( 'NONE',  ( 12.75768479220908169, 7.626547943635540783, -14.92479568483475028 ) ) ;
#2022 = CARTESIAN_POINT ( 'NONE',  ( 37.54859390953724585, -22.18451583373416014, -18.00000000000000000 ) ) ;
#2023 = LINE ( 'NONE', #1567, #14475 ) ;
#2024 = ORIENTED_EDGE ( 'NONE', *, *, #20166, .T. ) ;
#2025 = VERTEX_POINT ( 'NONE', #2227 ) ;
#2026 = LINE ( 'NONE', #18321, #3254 ) ;
#2027 = EDGE_LOOP ( 'NONE', ( #13919, #4831, #22546, #26614 ) ) ;
#2028 = CARTESIAN_POINT ( 'NONE',  ( 15.98547205987755149, 10.89358938796158149, -13.63095616771664709 ) ) ;
#2029 = AXIS2_PLACEMENT_3D ( 'NONE', #4808, #7102, #6807 ) ;
#2031 = VECTOR ( 'NONE', #25433, 1000.000000000000000 ) ;
#2030 = CARTESIAN_POINT ( 'NONE',  ( 32.83462640711407232, -10.30445905196369516, -16.67331141712644538 ) ) ;
#2032 = CARTESIAN_POINT ( 'NONE',  ( 24.68825858685077179, -9.385095155728059524, -16.92495907518576104 ) ) ;
#2033 = B_SPLINE_CURVE_WITH_KNOTS ( 'NONE', 3,
 ( #24314, #22164, #29550, #17867, #29234, #27083 ),
 .UNSPECIFIED., .F., .F.,
 ( 4, 2, 4 ),
 ( 0.006456566858647387087, 0.007625406818786638688, 0.008794246778925891156 ),
 .UNSPECIFIED. ) ;
#2034 = FACE_OUTER_BOUND ( 'NONE', #1925, .T. ) ;
#2035 = DIRECTION ( 'NONE',  ( 2.698458740408365879E-16, -1.000000000000000000, 0.000000000000000000 ) ) ;
#2036 = ORIENTED_EDGE ( 'NONE', *, *, #28323, .T. ) ;
#2037 = FILL_AREA_STYLE ('',( #10716 ) ) ;
#2038 = CARTESIAN_POINT ( 'NONE',  ( 27.15223745481332784, -12.21752729395051063, -18.24437427626675046 ) ) ;
#2039 = CARTESIAN_POINT ( 'NONE',  ( 24.41106252871404436, -7.915231898853421377, -13.94454578273958667 ) ) ;
#2040 = VERTEX_POINT ( 'NONE', #16241 ) ;
#2041 = DIRECTION ( 'NONE',  ( -0.8090169943749474513, -2.183098979609982436E-16, 0.5877852522924731371 ) ) ;
#2042 = EDGE_CURVE ( 'NONE', #26513, #16825, #11500, .T. ) ;
#2043 = CARTESIAN_POINT ( 'NONE',  ( -13.00000000000000178, 1.592040838891559293E-15, 15.00000000000000000 ) ) ;
#2044 = LINE ( 'NONE', #30010, #16034 ) ;
#2045 = VECTOR ( 'NONE', #18843, 1000.000000000000000 ) ;
#2046 = DIRECTION ( 'NONE',  ( -0.8090169943749474513, -2.183098979609982436E-16, 0.5877852522924731371 ) ) ;
#2047 = CARTESIAN_POINT ( 'NONE',  ( 12.48799528366842360, 8.565546312597838607, -15.13973160209665991 ) ) ;
#2048 = CARTESIAN_POINT ( 'NONE',  ( 27.61484239614359737, -11.78684095324212855, -18.66559939683001446 ) ) ;
#2049 = ORIENTED_EDGE ( 'NONE', *, *, #7802, .T. ) ;
#2050 = DIRECTION ( 'NONE',  ( 0.5877852522924731371, 1.586114251531760728E-16, 0.8090169943749474513 ) ) ;
#2051 = ORIENTED_EDGE ( 'NONE', *, *, #1762, .F. ) ;
#2052 = CARTESIAN_POINT ( 'NONE',  ( 9.641350810849047548, 17.66889113945805789, -17.93331994345748370 ) ) ;
#2053 = CARTESIAN_POINT ( 'NONE',  ( 27.56197131007709444, -12.41890123633259435, -14.84244373703855935 ) ) ;
#2054 = DIRECTION ( 'NONE',  ( 0.000000000000000000, 0.000000000000000000, -1.000000000000000000 ) ) ;
#2055 = CARTESIAN_POINT ( 'NONE',  ( 2.500000000000000444, 2.357898499370430834, -3.469446951953614189E-15 ) ) ;
#2056 = ORIENTED_EDGE ( 'NONE', *, *, #7085, .T. ) ;
#2058 = ORIENTED_EDGE ( 'NONE', *, *, #23632, .T. ) ;
#2057 = CARTESIAN_POINT ( 'NONE',  ( 23.56138260001205964, -6.829566487537672259, -18.05074380722902916 ) ) ;
#2059 = ORIENTED_EDGE ( 'NONE', *, *, #8323, .T. ) ;
#2060 = LINE ( 'NONE', #30028, #23231 ) ;
#2061 = CARTESIAN_POINT ( 'NONE',  ( 11.05541531668977662, 17.68942339022145305, -17.92981046679734547 ) ) ;
#2062 = CARTESIAN_POINT ( 'NONE',  ( 35.54859215833182873, -22.18450796649496226, -18.40462262104107083 ) ) ;
#2063 = PLANE ( 'NONE',  #16133 ) ;
#2064 = ORIENTED_EDGE ( 'NONE', *, *, #21308, .F. ) ;
#2065 = CARTESIAN_POINT ( 'NONE',  ( 24.14158683625483803, -3.940216521628096658, -13.50644477367014673 ) ) ;
#2066 = CARTESIAN_POINT ( 'NONE',  ( 130.7287565553229172, -10.00000000000000888, -30.76635726929466585 ) ) ;
#2067 = VECTOR ( 'NONE', #18751, 1000.000000000000000 ) ;
#2068 = CARTESIAN_POINT ( 'NONE',  ( 21.79248024726475563, -3.676524810334697246, -15.28166220873658077 ) ) ;
#2069 = ORIENTED_EDGE ( 'NONE', *, *, #4771, .F. ) ;
#2070 = DIRECTION ( 'NONE',  ( 0.5877852522924731371, 0.000000000000000000, 0.8090169943749474513 ) ) ;
#2071 = EDGE_CURVE ( 'NONE', #23292, #10473, #9039, .T. ) ;
#2072 = VECTOR ( 'NONE', #6617, 1000.000000000000000 ) ;
#2073 = CARTESIAN_POINT ( 'NONE',  ( 16.38240814442996651, 6.370603895193741373, -13.89573738210111919 ) ) ;
#2074 = PRODUCT_RELATED_PRODUCT_CATEGORY ( 'part', '', ( #29395 ) ) ;
#2075 = CARTESIAN_POINT ( 'NONE',  ( 30.15014520769674533, -9.019674524353797906, -15.19912247041013842 ) ) ;
#2076 = ORIENTED_EDGE ( 'NONE', *, *, #7497, .T. ) ;
#2077 = DIRECTION ( 'NONE',  ( 1.110223024625156540E-16, 2.995891024602366092E-32, 1.000000000000000000 ) ) ;
#2078 = AXIS2_PLACEMENT_3D ( 'NONE', #825, #9667, #12260 ) ;
#2079 = CARTESIAN_POINT ( 'NONE',  ( 168.6922820468853388, -9.999999999999996447, -17.92658477444275889 ) ) ;
#2080 = VERTEX_POINT ( 'NONE', #23574 ) ;
#2081 = FACE_OUTER_BOUND ( 'NONE', #21700, .T. ) ;
#2082 = CARTESIAN_POINT ( 'NONE',  ( 174.5152310637604671, -9.999999999999994671, -19.94844914048349693 ) ) ;
#2083 = CARTESIAN_POINT ( 'NONE',  ( 136.1922820468854241, -4.999999999999980460, -10.74328820663507322 ) ) ;
#2084 = AXIS2_PLACEMENT_3D ( 'NONE', #2149, #27649, #13273 ) ;
#2085 = DIRECTION ( 'NONE',  ( -0.9510565162951536422, -2.566386769018988323E-16, 0.3090169943749475623 ) ) ;
#2086 = CARTESIAN_POINT ( 'NONE',  ( 23.39714218815755231, -8.028440028060597200, -17.83143846932372512 ) ) ;
#2087 = CARTESIAN_POINT ( 'NONE',  ( 21.65198393244800812, 4.573788442230395823, -17.29480057625502454 ) ) ;
#2089 = ORIENTED_EDGE ( 'NONE', *, *, #28976, .F. ) ;
#2088 = CARTESIAN_POINT ( 'NONE',  ( 33.72790161547175103, -10.96501189107364738, -20.51660325596433765 ) ) ;
#2090 = CYLINDRICAL_SURFACE ( 'NONE', #3703, 8.000000000000000000 ) ;
#2091 = CARTESIAN_POINT ( 'NONE',  ( 12.44984726620633353, 8.550925603015029353, -15.16996558791898231 ) ) ;
#2092 = DIRECTION ( 'NONE',  ( -2.698458740408365879E-16, 1.000000000000000000, 0.000000000000000000 ) ) ;
#2093 = LINE ( 'NONE', #22688, #27122 ) ;
#2094 = CARTESIAN_POINT ( 'NONE',  ( 9.667840685194843076, 16.22750421244806063, -17.88508776754438401 ) ) ;
#2095 = CARTESIAN_POINT ( 'NONE',  ( -12.69484042717385464, 39.89788248176327556, 4.999999999999998224 ) ) ;
#2096 = ORIENTED_EDGE ( 'NONE', *, *, #6742, .T. ) ;
#2097 = DIRECTION ( 'NONE',  ( -0.000000000000000000, 0.000000000000000000, 1.000000000000000000 ) ) ;
#2098 = CARTESIAN_POINT ( 'NONE',  ( 12.23783994716398560, 8.515526397163364791, -15.33449341356891615 ) ) ;
#2099 = ORIENTED_EDGE ( 'NONE', *, *, #6954, .T. ) ;
#2100 = DIRECTION ( 'NONE',  ( -0.9510565162951536422, -2.566386769018988816E-16, -0.3090169943749472292 ) ) ;
#2101 = DIRECTION ( 'NONE',  ( -0.5877852522924731371, -1.586114251531760235E-16, 0.8090169943749474513 ) ) ;
#2102 = AXIS2_PLACEMENT_3D ( 'NONE', #21046, #150, #16913 ) ;
#2103 = APPLICATION_CONTEXT ( 'automotive_design' ) ;
#2104 = PLANE ( 'NONE',  #4427 ) ;
#2105 = ORIENTED_EDGE ( 'NONE', *, *, #1590, .F. ) ;
#2106 = CARTESIAN_POINT ( 'NONE',  ( 10.34450975306715570, 10.53135794231081057, -16.54525784588868120 ) ) ;
#2107 = CARTESIAN_POINT ( 'NONE',  ( 31.15806985163746390, -10.82494328065958911, -14.16671120874331358 ) ) ;
#2108 = EDGE_CURVE ( 'NONE', #28209, #22503, #9210, .T. ) ;
#2109 = ADVANCED_FACE ( 'NONE', ( #9360 ), #9509, .F. ) ;
#2110 = CARTESIAN_POINT ( 'NONE',  ( 18.14419664895403272, 7.915595134365798202, -13.41836860846829538 ) ) ;
#2111 = EDGE_CURVE ( 'NONE', #18112, #26865, #786, .T. ) ;
#2112 = CARTESIAN_POINT ( 'NONE',  ( 14.70507544977879100, 5.024503852999842479, -17.88552553980999704 ) ) ;
#2113 = VECTOR ( 'NONE', #12320, 1000.000000000000000 ) ;
#2114 = EDGE_CURVE ( 'NONE', #21937, #14836, #2670, .T. ) ;
#2115 = CARTESIAN_POINT ( 'NONE',  ( -4.000000000000008882, 6.928203230275508773, -5.000000000000000888 ) ) ;
#2116 = CARTESIAN_POINT ( 'NONE',  ( 22.15378238435969394, -4.028439702987021143, -12.64872919198682943 ) ) ;
#2117 = ORIENTED_EDGE ( 'NONE', *, *, #11471, .F. ) ;
#2118 = PLANE ( 'NONE',  #24039 ) ;
#2119 = VERTEX_POINT ( 'NONE', #16393 ) ;
#2121 = VERTEX_POINT ( 'NONE', #13940 ) ;
#2120 = CARTESIAN_POINT ( 'NONE',  ( 154.5152310637605524, -1.999999999999974465, -19.94844914048349693 ) ) ;
#2122 = ORIENTED_EDGE ( 'NONE', *, *, #3314, .T. ) ;
#2123 = CARTESIAN_POINT ( 'NONE',  ( 1.214306433183764966E-14, 4.618802153517016507, -2.450000000000000178 ) ) ;
#2124 = CARTESIAN_POINT ( 'NONE',  ( 13.66828981435543788, 8.811555337407297017, -15.47779131845254952 ) ) ;
#2125 = CARTESIAN_POINT ( 'NONE',  ( 35.05137900175546406, -18.95079263513605028, -19.16533087415493952 ) ) ;
#2126 = CARTESIAN_POINT ( 'NONE',  ( 10.70135522441200671, 8.911701773272509897, -16.39640207298747754 ) ) ;
#2127 = ORIENTED_EDGE ( 'NONE', *, *, #24104, .T. ) ;
#2128 = AXIS2_PLACEMENT_3D ( 'NONE', #6346, #1174, #15641 ) ;
#2129 = CARTESIAN_POINT ( 'NONE',  ( 28.15048769591263067, -5.842385520647848551, -16.89978903947823241 ) ) ;
#2130 = DIRECTION ( 'NONE',  ( 0.5000000000000014433, -0.8660254037844378194, 0.000000000000000000 ) ) ;
#2131 = CARTESIAN_POINT ( 'NONE',  ( 10.47300640208398370, 16.44766825625507778, -17.33439677017039671 ) ) ;
#2132 = DIRECTION ( 'NONE',  ( 0.000000000000000000, 0.000000000000000000, -1.000000000000000000 ) ) ;
#2133 = DIRECTION ( 'NONE',  ( -2.698458740408365879E-16, 1.000000000000000000, 0.000000000000000000 ) ) ;
#2134 = ORIENTED_EDGE ( 'NONE', *, *, #23845, .F. ) ;
#2135 = CARTESIAN_POINT ( 'NONE',  ( 164.7287565553229740, -1.999999999999970912, -33.82050807568879947 ) ) ;
#2136 = CARTESIAN_POINT ( 'NONE',  ( 12.55500454421123457, 8.595009676161804890, -15.08633542003848049 ) ) ;
#2137 = VERTEX_POINT ( 'NONE', #9056 ) ;
#2138 = CARTESIAN_POINT ( 'NONE',  ( 0.000000000000000000, 0.000000000000000000, 0.000000000000000000 ) ) ;
#2139 = ORIENTED_EDGE ( 'NONE', *, *, #18688, .T. ) ;
#2140 = CARTESIAN_POINT ( 'NONE',  ( 9.667821753224751902, 16.22759103687616999, -17.88509611560606061 ) ) ;
#2141 = ADVANCED_FACE ( 'NONE', ( #16705 ), #28194, .T. ) ;
#2142 = CARTESIAN_POINT ( 'NONE',  ( 24.26229878782818261, 2.002655289519151172, -16.31248287692968546 ) ) ;
#2143 = CARTESIAN_POINT ( 'NONE',  ( 23.66883837772530441, 2.046813550970532969, -14.77838854720118000 ) ) ;
#2144 = ADVANCED_FACE ( 'NONE', ( #16550 ), #18690, .F. ) ;
#2145 = ADVANCED_FACE ( 'NONE', ( #4797 ), #25167, .T. ) ;
#2146 = CARTESIAN_POINT ( 'NONE',  ( 17.20140313730510684, 4.016069822000726042, -19.84498366692964666 ) ) ;
#2147 = DIRECTION ( 'NONE',  ( 0.000000000000000000, 0.000000000000000000, -1.000000000000000000 ) ) ;
#2148 = ADVANCED_FACE ( 'NONE', ( #4647 ), #14089, .T. ) ;
#2149 = CARTESIAN_POINT ( 'NONE',  ( 162.2287565553229172, -9.999999999999998224, -12.16987298107780369 ) ) ;
#2150 = CARTESIAN_POINT ( 'NONE',  ( 17.72480397827495224, 1.356124466512965476, -19.40231245121514903 ) ) ;
#2151 = AXIS2_PLACEMENT_3D ( 'NONE', #28036, #4349, #7090 ) ;
#2152 = CARTESIAN_POINT ( 'NONE',  ( 144.7287565553230024, -4.999999999999978684, -7.839745962155614478 ) ) ;
#2153 = DIRECTION ( 'NONE',  ( 2.908569913943825554E-16, -1.000000000000000000, 0.000000000000000000 ) ) ;
#2154 = CARTESIAN_POINT ( 'NONE',  ( 10.35865005771744762, 16.97212102856341787, -17.91352035578586310 ) ) ;
#2155 = CARTESIAN_POINT ( 'NONE',  ( 147.0152310637605240, -4.999999999999977796, 1.702185954127501066 ) ) ;
#2156 = DIRECTION ( 'NONE',  ( -1.000000000000000000, 0.000000000000000000, 0.000000000000000000 ) ) ;
#2157 = ORIENTED_EDGE ( 'NONE', *, *, #18939, .F. ) ;
#2158 = ORIENTED_EDGE ( 'NONE', *, *, #5327, .F. ) ;
#2159 = DIRECTION ( 'NONE',  ( 1.000000000000000000, 2.891205793294675861E-16, 0.000000000000000000 ) ) ;
#2160 = CARTESIAN_POINT ( 'NONE',  ( 17.29421355564066332, 9.360779442694735053, -19.18964209290773937 ) ) ;
#2161 = CARTESIAN_POINT ( 'NONE',  ( 11.25757798850943381, 16.76227960750979307, -16.79548539596511247 ) ) ;
#2162 = FACE_OUTER_BOUND ( 'NONE', #11468, .T. ) ;
#2163 = ORIENTED_EDGE ( 'NONE', *, *, #14056, .F. ) ;
#2164 = ORIENTED_EDGE ( 'NONE', *, *, #27058, .T. ) ;
#2165 = CARTESIAN_POINT ( 'NONE',  ( 9.893572868141015775, 16.51216863388285461, -16.51808063826580408 ) ) ;
#2166 = VECTOR ( 'NONE', #19653, 1000.000000000000000 ) ;
#2167 = CARTESIAN_POINT ( 'NONE',  ( 9.641350810849047548, 17.66889113945805789, -21.33333333332589277 ) ) ;
#2168 = DIRECTION ( 'NONE',  ( -0.9510565162951536422, -2.566386769018988816E-16, -0.3090169943749472292 ) ) ;
#2169 = DIRECTION ( 'NONE',  ( 0.000000000000000000, 0.000000000000000000, 1.000000000000000000 ) ) ;
#2170 = ORIENTED_EDGE ( 'NONE', *, *, #5331, .F. ) ;
#2171 = DIRECTION ( 'NONE',  ( -0.9510565162951536422, -2.566386769018988816E-16, -0.3090169943749472292 ) ) ;
#2172 = VERTEX_POINT ( 'NONE', #7092 ) ;
#2173 = CARTESIAN_POINT ( 'NONE',  ( 10.46817501828509123, 16.46982559821503145, -17.33665662920367723 ) ) ;
#2174 = CARTESIAN_POINT ( 'NONE',  ( 33.97319001242765779, -11.13623552147873141, -19.50814438409551954 ) ) ;
#2175 = CARTESIAN_POINT ( 'NONE',  ( 27.31974442496251143, -5.660127319198639206, -14.41990313654811651 ) ) ;
#2176 = VERTEX_POINT ( 'NONE', #11951 ) ;
#2177 = EDGE_CURVE ( 'NONE', #29408, #24657, #2538, .T. ) ;
#2178 = EDGE_LOOP ( 'NONE', ( #378, #21895, #3651, #22795, #9995 ) ) ;
#2179 = EDGE_CURVE ( 'NONE', #29391, #30115, #11806, .T. ) ;
#2180 = DIRECTION ( 'NONE',  ( 1.000000000000000000, 4.440892098500621724E-16, 0.000000000000000000 ) ) ;
#2181 = ORIENTED_EDGE ( 'NONE', *, *, #3371, .T. ) ;
#2182 = EDGE_CURVE ( 'NONE', #461, #12786, #3042, .T. ) ;
#2183 = ADVANCED_FACE ( 'NONE', ( #18383 ), #27737, .T. ) ;
#2184 = CARTESIAN_POINT ( 'NONE',  ( 106.5152396090253148, -4.999999999999988454, 77.38785145663800336 ) ) ;
#2185 = DIRECTION ( 'NONE',  ( 0.9237280213470682178, 0.3830490080632377725, 0.000000000000000000 ) ) ;
#2186 = CARTESIAN_POINT ( 'NONE',  ( 15.30293317557315902, 5.113330479851449617, -15.60941525921096051 ) ) ;
#2187 = CARTESIAN_POINT ( 'NONE',  ( 25.07632161252335123, -1.101686516974712315, -19.85338880782979132 ) ) ;
#2188 = ORIENTED_EDGE ( 'NONE', *, *, #2274, .T. ) ;
#2189 = PLANE ( 'NONE',  #18642 ) ;
#2190 = VECTOR ( 'NONE', #14427, 1000.000000000000000 ) ;
#2191 = CARTESIAN_POINT ( 'NONE',  ( 176.1922820468852819, -9.999999999999994671, -13.59645775552055902 ) ) ;
#2192 = LINE ( 'NONE', #20772, #16546 ) ;
#2193 = CARTESIAN_POINT ( 'NONE',  ( 146.4575131106458912, -9.999999999999976907, -15.00000000000000000 ) ) ;
#2194 = PRODUCT_DEFINITION_CONTEXT ( 'detailed design', #26069, 'design' ) ;
#2195 = CARTESIAN_POINT ( 'NONE',  ( 10.72335299953182286, 16.61944783517715862, -15.95314022879208693 ) ) ;
#2196 = CARTESIAN_POINT ( 'NONE',  ( 2.500000000000000444, 2.357898499370430834, -3.469446951953614189E-15 ) ) ;
#2197 = ORIENTED_EDGE ( 'NONE', *, *, #18377, .T. ) ;
#2198 = DIRECTION ( 'NONE',  ( -1.110223024625156540E-16, 0.000000000000000000, -1.000000000000000000 ) ) ;
#2199 = ORIENTED_EDGE ( 'NONE', *, *, #26218, .F. ) ;
#2200 = CARTESIAN_POINT ( 'NONE',  ( 9.919231947839115549, 16.39449282361540483, -16.50339887433786501 ) ) ;
#2201 = CARTESIAN_POINT ( 'NONE',  ( 17.86202776125589153, 5.750484210099715554, -19.07881598002096268 ) ) ;
#2202 = DIRECTION ( 'NONE',  ( -0.9510565162951536422, -2.566386769018988323E-16, 0.3090169943749475623 ) ) ;
#2203 = DIRECTION ( 'NONE',  ( -2.698458740408365879E-16, 1.000000000000000000, 0.000000000000000000 ) ) ;
#2205 = EDGE_LOOP ( 'NONE', ( #16150, #2209, #7218, #11627 ) ) ;
#2204 = CARTESIAN_POINT ( 'NONE',  ( 25.07290406138036687, -9.006318079059196791, -17.79994936451110732 ) ) ;
#2206 = VERTEX_POINT ( 'NONE', #14993 ) ;
#2207 = DIRECTION ( 'NONE',  ( 6.938893903907227392E-16, -0.000000000000000000, 1.000000000000000000 ) ) ;
#2208 = CARTESIAN_POINT ( 'NONE',  ( 12.38124869470495781, 9.576253617860157163, -15.22482189909362660 ) ) ;
#2209 = ORIENTED_EDGE ( 'NONE', *, *, #3675, .F. ) ;
#2210 = CARTESIAN_POINT ( 'NONE',  ( 32.25667210025905263, -11.64161264113965011, -15.27003429613047025 ) ) ;
#2211 = CARTESIAN_POINT ( 'NONE',  ( 132.2287565553230024, -10.00000000000000888, -3.509618943233403510 ) ) ;
#2212 = VERTEX_POINT ( 'NONE', #21875 ) ;
#2213 = ADVANCED_FACE ( 'NONE', ( #7841 ), #23892, .T. ) ;
#2214 = CIRCLE ( 'NONE', #10944, 4.000000000000000000 ) ;
#2215 = LINE ( 'NONE', #4189, #12522 ) ;
#2216 = CARTESIAN_POINT ( 'NONE',  ( 24.19805618307960060, -0.7920880973371497991, -16.79971198345035432 ) ) ;
#2217 = ORIENTED_EDGE ( 'NONE', *, *, #9890, .T. ) ;
#2218 = EDGE_CURVE ( 'NONE', #19798, #4416, #26479, .T. ) ;
#2219 = DIRECTION ( 'NONE',  ( 0.000000000000000000, -1.000000000000000000, 0.000000000000000000 ) ) ;
#2220 = ORIENTED_EDGE ( 'NONE', *, *, #2042, .T. ) ;
#2221 = FILL_AREA_STYLE ('',( #18679 ) ) ;
#2222 = CARTESIAN_POINT ( 'NONE',  ( 20.55949567978923298, 1.660703385868308235, -14.27713627412184039 ) ) ;
#2223 = CARTESIAN_POINT ( 'NONE',  ( 27.32970014129078962, -12.32490512882196754, -16.69500413328365696 ) ) ;
#2224 = EDGE_LOOP ( 'NONE', ( #22672, #8764, #8225, #13266 ) ) ;
#2225 = CARTESIAN_POINT ( 'NONE',  ( 151.1922820468853672, -1.999999999999976685, -4.936203717676158398 ) ) ;
#2226 = DIRECTION ( 'NONE',  ( 0.9510565162951536422, 0.000000000000000000, -0.3090169943749475623 ) ) ;
#2227 = CARTESIAN_POINT ( 'NONE',  ( 141.1922820468854525, -1.999999999999979128, -19.40354224447947473 ) ) ;
#2228 = DIRECTION ( 'NONE',  ( -0.9510565162951536422, -2.566386769018988323E-16, 0.3090169943749475623 ) ) ;
#2229 = DIRECTION ( 'NONE',  ( -0.9510565162951536422, 0.000000000000000000, -0.3090169943749472292 ) ) ;
#2230 = VECTOR ( 'NONE', #14958, 1000.000000000000000 ) ;
#2231 = CARTESIAN_POINT ( 'NONE',  ( 9.917205744531459644, 16.40378525026516243, -16.50423678068149869 ) ) ;
#2232 = CARTESIAN_POINT ( 'NONE',  ( 20.87485249991972580, -5.094386175754089585, -18.86169636093909219 ) ) ;
#2233 = CARTESIAN_POINT ( 'NONE',  ( 18.32179412900206827, 3.681508181950223335, -14.15692665485406643 ) ) ;
#2234 = EDGE_CURVE ( 'NONE', #26570, #10404, #12407, .T. ) ;
#2235 = EDGE_CURVE ( 'NONE', #7797, #18644, #10269, .T. ) ;
#2236 = CARTESIAN_POINT ( 'NONE',  ( 33.45813146310553066, -13.79317541067231723, -20.76837346131055639 ) ) ;
#2237 =( LENGTH_UNIT ( ) NAMED_UNIT ( * ) SI_UNIT ( .MILLI., .METRE. ) );
#2238 = CARTESIAN_POINT ( 'NONE',  ( 12.39803340617553928, 8.535179507765855433, -15.21071672276548625 ) ) ;
#2239 = DIRECTION ( 'NONE',  ( 0.9510565162951536422, 0.000000000000000000, -0.3090169943749475623 ) ) ;
#2240 = CARTESIAN_POINT ( 'NONE',  ( 141.1922820468854525, -1.999999999999978684, -28.06379628232387446 ) ) ;
#2241 = CARTESIAN_POINT ( 'NONE',  ( 14.34656430690936624, 9.113120221615268690, -15.03016663717492563 ) ) ;
#2242 = ORIENTED_EDGE ( 'NONE', *, *, #20926, .F. ) ;
#2243 = DIRECTION ( 'NONE',  ( -1.000000000000000000, -2.698458740408365879E-16, -0.000000000000000000 ) ) ;
#2244 = CARTESIAN_POINT ( 'NONE',  ( 14.38576730248667701, 9.404056492746565965, -13.62718518646353161 ) ) ;
#2245 = VECTOR ( 'NONE', #13063, 1000.000000000000000 ) ;
#2246 = EDGE_LOOP ( 'NONE', ( #6110, #5836, #1827, #7710 ) ) ;
#2247 = CARTESIAN_POINT ( 'NONE',  ( 134.5152310637605808, -4.999999999999981348, -11.28819510263909187 ) ) ;
#2248 = CARTESIAN_POINT ( 'NONE',  ( 152.2287565553230309, -1.999999999999974465, -29.49038105676660493 ) ) ;
#2249 = AXIS2_PLACEMENT_3D ( 'NONE', #24723, #22430, #8220 ) ;
#2250 = CARTESIAN_POINT ( 'NONE',  ( 16.75072914628186282, 8.771658487634226731, -19.67538163746542779 ) ) ;
#2251 = EDGE_CURVE ( 'NONE', #17576, #26769, #12711, .T. ) ;
#2252 = ORIENTED_EDGE ( 'NONE', *, *, #18555, .T. ) ;
#2253 = CARTESIAN_POINT ( 'NONE',  ( 9.109746387114286748, 16.19414013429083710, -17.05597298747021640 ) ) ;
#2254 = CARTESIAN_POINT ( 'NONE',  ( 33.35113679096266992, -13.31250502539155534, -20.73603153870848104 ) ) ;
#2255 = CARTESIAN_POINT ( 'NONE',  ( 16.82931527361030533, 7.354042003703605168, -13.11858969620360504 ) ) ;
#2256 = CIRCLE ( 'NONE', #6137, 1.500000000000001332 ) ;
#2257 = CARTESIAN_POINT ( 'NONE',  ( 27.62103240953636174, -12.62788667074165794, -13.46147607715242245 ) ) ;
#2258 = CIRCLE ( 'NONE', #19286, 4.000000000000003553 ) ;
#2259 = CARTESIAN_POINT ( 'NONE',  ( 149.5152310637605808, -10.00000000000000178, -30.37205893520531319 ) ) ;
#2260 = CARTESIAN_POINT ( 'NONE',  ( 20.29686952095399377, -4.285349973794369660, -18.75376381207850329 ) ) ;
#2261 = VECTOR ( 'NONE', #232, 1000.000000000000000 ) ;
#2262 = ORIENTED_EDGE ( 'NONE', *, *, #20668, .T. ) ;
#2263 = PLANE ( 'NONE',  #1141 ) ;
#2265 = ORIENTED_EDGE ( 'NONE', *, *, #24913, .F. ) ;
#2264 = DIRECTION ( 'NONE',  ( 0.5877852522924731371, 1.586114251531760728E-16, 0.8090169943749474513 ) ) ;
#2266 = VERTEX_POINT ( 'NONE', #26327 ) ;
#2267 = CARTESIAN_POINT ( 'NONE',  ( 151.1922820468854525, -10.00000000000000178, -28.06379628232387802 ) ) ;
#2268 = AXIS2_PLACEMENT_3D ( 'NONE', #28367, #7860, #2691 ) ;
#2269 = CARTESIAN_POINT ( 'NONE',  ( 149.7287565553229456, -10.00000000000000355, 0.8205080756887930260 ) ) ;
#2270 = EDGE_CURVE ( 'NONE', #15678, #12642, #26790, .T. ) ;
#2271 = CARTESIAN_POINT ( 'NONE',  ( 36.44623027834506956, -20.72465026231317253, -19.27049969669971929 ) ) ;
#2272 = VECTOR ( 'NONE', #6813, 1000.000000000000000 ) ;
#2273 = CARTESIAN_POINT ( 'NONE',  ( 10.63628302936969483, 9.193248504745362482, -16.42459933240677827 ) ) ;
#2274 = EDGE_CURVE ( 'NONE', #16222, #18174, #5710, .T. ) ;
#2275 = EDGE_LOOP ( 'NONE', ( #4680, #12647, #21018, #23137 ) ) ;
#2276 = AXIS2_PLACEMENT_3D ( 'NONE', #10583, #20335, #6166 ) ;
#2277 = PLANE ( 'NONE',  #3934 ) ;
#2278 = FACE_OUTER_BOUND ( 'NONE', #25468, .T. ) ;
#2279 = CARTESIAN_POINT ( 'NONE',  ( 10.63408956504272140, 15.70892033759881734, -17.26778321585235787 ) ) ;
#2280 = CARTESIAN_POINT ( 'NONE',  ( 149.7287565553230309, -10.00000000000000178, -25.16025403784440329 ) ) ;
#2281 = DIRECTION ( 'NONE',  ( -0.9510565162951536422, -2.566386769018988816E-16, -0.3090169943749472292 ) ) ;
#2282 = EDGE_LOOP ( 'NONE', ( #11648, #19219, #5264, #14423 ) ) ;
#2283 = CARTESIAN_POINT ( 'NONE',  ( 156.1922820468853956, -1.999999999999975353, -19.40354224447947828 ) ) ;
#2284 = DIRECTION ( 'NONE',  ( -1.110223024625156540E-16, 0.000000000000000000, -1.000000000000000000 ) ) ;
#2285 = DIRECTION ( 'NONE',  ( -2.908569913943826047E-16, 1.000000000000000000, 6.826925868028084813E-18 ) ) ;
#2286 = VERTEX_POINT ( 'NONE', #22033 ) ;
#2287 = CARTESIAN_POINT ( 'NONE',  ( 9.732710754582456048, 15.93000180522596665, -17.85826136589200175 ) ) ;
#2288 = CARTESIAN_POINT ( 'NONE',  ( 22.68697051328012293, -3.855329871767240402, -18.23939831819710733 ) ) ;
#2289 = CARTESIAN_POINT ( 'NONE',  ( 23.24226111988221888, -3.343277867803439829, -18.62279721135557509 ) ) ;
#2290 = CARTESIAN_POINT ( 'NONE',  ( 21.63689124574611711, 4.661388338709377521, -16.95871344450652174 ) ) ;
#2291 = VECTOR ( 'NONE', #13931, 999.9999999999998863 ) ;
#2292 = DIRECTION ( 'NONE',  ( 0.9510565162951536422, 2.566386769018988816E-16, 0.3090169943749472292 ) ) ;
#2293 = FACE_OUTER_BOUND ( 'NONE', #25182, .T. ) ;
#2294 = PLANE ( 'NONE',  #2084 ) ;
#2295 = VECTOR ( 'NONE', #18970, 1000.000000000000000 ) ;
#2296 = CARTESIAN_POINT ( 'NONE',  ( 27.78884322698630882, -6.380937659459246625, -17.89340433249687834 ) ) ;
#2297 = AXIS2_PLACEMENT_3D ( 'NONE', #25842, #21241, #11775 ) ;
#2298 = VERTEX_POINT ( 'NONE', #5254 ) ;
#2299 = PRESENTATION_STYLE_ASSIGNMENT (( #2742 ) ) ;
#2300 = DIRECTION ( 'NONE',  ( 0.000000000000000000, 0.000000000000000000, 1.000000000000000000 ) ) ;
#2301 = CARTESIAN_POINT ( 'NONE',  ( 148.6922820468854241, -10.00000000000000178, -17.92658477444275889 ) ) ;
#2302 = CARTESIAN_POINT ( 'NONE',  ( -2.681483223904239210, 3.070647092368423259, 4.157051104216616720E-15 ) ) ;
#2303 = DIRECTION ( 'NONE',  ( 0.000000000000000000, -0.7071067811865455743, 0.7071067811865495711 ) ) ;
#2304 = CARTESIAN_POINT ( 'NONE',  ( 10.46247360472336041, 16.49597300757040230, -17.34042816522791952 ) ) ;
#2305 = ADVANCED_FACE ( 'NONE', ( #10419 ), #19581, .F. ) ;
#2306 = PLANE ( 'NONE',  #25775 ) ;
#2307 = CARTESIAN_POINT ( 'NONE',  ( 154.5152310637604955, -4.999999999999976019, -1.715463671822631215E-14 ) ) ;
#2308 = ORIENTED_EDGE ( 'NONE', *, *, #19397, .F. ) ;
#2309 = CARTESIAN_POINT ( 'NONE',  ( 10.96464236563772943, 10.28020640217055259, -17.34881430896752619 ) ) ;
#2310 = EDGE_CURVE ( 'NONE', #887, #16400, #19794, .T. ) ;
#2311 = ORIENTED_EDGE ( 'NONE', *, *, #20926, .T. ) ;
#2312 = CARTESIAN_POINT ( 'NONE',  ( 8.000000000000000000, 9.797174393178825657E-16, -15.00000000000000355 ) ) ;
#2313 = VECTOR ( 'NONE', #10243, 1000.000000000000000 ) ;
#2314 = EDGE_CURVE ( 'NONE', #15020, #15488, #14298, .T. ) ;
#2315 = CARTESIAN_POINT ( 'NONE',  ( 20.39549844898813191, -2.061726703908969505, -13.85117726305786512 ) ) ;
#2316 = CARTESIAN_POINT ( 'NONE',  ( 11.08268301555968094, 17.56437024738003316, -17.37355016474266733 ) ) ;
#2317 = CARTESIAN_POINT ( 'NONE',  ( 33.47012763672258728, -12.84706786418751534, -19.72967806864707541 ) ) ;
#2318 = VERTEX_POINT ( 'NONE', #17438 ) ;
#2319 = EDGE_LOOP ( 'NONE', ( #16188, #11098, #11207, #23126, #15990 ) ) ;
#2320 = AXIS2_PLACEMENT_3D ( 'NONE', #7927, #26569, #26727 ) ;
#2321 = CARTESIAN_POINT ( 'NONE',  ( 9.641350810849047548, 17.66889113945805789, -17.92015940598198753 ) ) ;
#2322 = DIRECTION ( 'NONE',  ( -0.5877852522924731371, 0.000000000000000000, 0.8090169943749474513 ) ) ;
#2323 = CARTESIAN_POINT ( 'NONE',  ( 9.641350810849047548, 17.66889113945805789, -17.92454625180715766 ) ) ;
#2324 = CARTESIAN_POINT ( 'NONE',  ( 132.0152310637605808, -1.999999999999981348, -24.27857615940569147 ) ) ;
#2325 = CARTESIAN_POINT ( 'NONE',  ( -7.806255641895631925E-14, -4.618802153517044928, -2.092734410091829034 ) ) ;
#2326 = ORIENTED_EDGE ( 'NONE', *, *, #27824, .F. ) ;
#2327 = EDGE_LOOP ( 'NONE', ( #6846, #6618, #28633, #9427 ) ) ;
#2328 = CARTESIAN_POINT ( 'NONE',  ( -2.339468227445740123, -3.268109542640673215, -2.121182258161580993E-14 ) ) ;
#2329 = ORIENTED_EDGE ( 'NONE', *, *, #11651, .T. ) ;
#2330 = CARTESIAN_POINT ( 'NONE',  ( 10.47204342302745417, 16.45208460095963687, -17.33479495221483901 ) ) ;
#2331 = CARTESIAN_POINT ( 'NONE',  ( 34.15817405333866219, -12.44562566045073204, -20.90971876709214783 ) ) ;
#2332 = CARTESIAN_POINT ( 'NONE',  ( 25.24878800877705487, -9.370948223588685622, -14.18615728435988288 ) ) ;
#2333 = ORIENTED_EDGE ( 'NONE', *, *, #24528, .F. ) ;
#2334 = DIRECTION ( 'NONE',  ( -2.698458740408365879E-16, 1.000000000000000000, 0.000000000000000000 ) ) ;
#2335 = CARTESIAN_POINT ( 'NONE',  ( 3.999999999999996447, 0.000000000000000000, 8.673617379884035472E-16 ) ) ;
#2336 = DIRECTION ( 'NONE',  ( 1.000000000000000000, 0.000000000000000000, 0.000000000000000000 ) ) ;
#2337 = CARTESIAN_POINT ( 'NONE',  ( 19.14730738223925854, 6.711798791111892371, -15.43835307388804701 ) ) ;
#2338 = CARTESIAN_POINT ( 'NONE',  ( 26.67280208910032258, -8.806626608708889137, -18.22016464309510653 ) ) ;
#2339 = VECTOR ( 'NONE', #1378, 1000.000000000000000 ) ;
#2340 = ORIENTED_EDGE ( 'NONE', *, *, #1847, .T. ) ;
#2341 = DIRECTION ( 'NONE',  ( -1.000000000000000000, 0.000000000000000000, 1.387778780781445676E-16 ) ) ;
#2342 = CONICAL_SURFACE ( 'NONE', #2821, 4.187999999999997947, 0.7853981633974482790 ) ;
#2343 = VERTEX_POINT ( 'NONE', #5409 ) ;
#2344 = LINE ( 'NONE', #9016, #6234 ) ;
#2345 = CARTESIAN_POINT ( 'NONE',  ( 162.0152310637604671, -4.999999999999974243, -17.38167787843871182 ) ) ;
#2346 = EDGE_CURVE ( 'NONE', #22282, #18177, #5862, .T. ) ;
#2347 = DIRECTION ( 'NONE',  ( -2.698458740408365879E-16, 1.000000000000000000, 0.000000000000000000 ) ) ;
#2348 = EDGE_CURVE ( 'NONE', #28792, #14970, #24475, .T. ) ;
#2349 = EDGE_CURVE ( 'NONE', #29672, #2431, #21431, .T. ) ;
#2350 = CARTESIAN_POINT ( 'NONE',  ( 10.72031594518761466, 16.63337615353409760, -15.95439753950889106 ) ) ;
#2351 = EDGE_CURVE ( 'NONE', #11550, #15239, #24036, .T. ) ;
#2352 = CARTESIAN_POINT ( 'NONE',  ( 137.0152310637606092, -1.999999999999979572, -24.27857615940569147 ) ) ;
#2353 = ORIENTED_EDGE ( 'NONE', *, *, #483, .F. ) ;
#2354 = CARTESIAN_POINT ( 'NONE',  ( 159.5152310637604955, -4.999999999999974243, -21.71180489736091346 ) ) ;
#2355 = ORIENTED_EDGE ( 'NONE', *, *, #17783, .T. ) ;
#2356 = CARTESIAN_POINT ( 'NONE',  ( 10.43540724046455992, 14.02724713458965233, -16.28994223329847202 ) ) ;
#2357 = VECTOR ( 'NONE', #11359, 1000.000000000000000 ) ;
#2358 = CARTESIAN_POINT ( 'NONE',  ( 16.45434084995319424, 8.990804261541395448, -14.78801614696073408 ) ) ;
#2359 = CARTESIAN_POINT ( 'NONE',  ( 164.5152310637605240, -4.999999999999972466, -28.60870317832789667 ) ) ;
#2360 = CARTESIAN_POINT ( 'NONE',  ( 0.000000000000000000, 0.000000000000000000, 9.999999999999998224 ) ) ;
#2362 = ORIENTED_EDGE ( 'NONE', *, *, #9665, .T. ) ;
#2361 = CARTESIAN_POINT ( 'NONE',  ( 25.97256211245905533, -8.171536508395311316, -18.54953510021574559 ) ) ;
#2363 = VERTEX_POINT ( 'NONE', #19429 ) ;
#2364 = CYLINDRICAL_SURFACE ( 'NONE', #20773, 13.00000000000000178 ) ;
#2365 = CARTESIAN_POINT ( 'NONE',  ( 11.40579136381300174, 16.08255417555669453, -16.73093107180499928 ) ) ;
#2366 = EDGE_LOOP ( 'NONE', ( #17895, #10638, #12091, #6441 ) ) ;
#2367 = VECTOR ( 'NONE', #30002, 1000.000000000000000 ) ;
#2368 = CARTESIAN_POINT ( 'NONE',  ( 32.61797162530606187, -11.69648652134232414, -16.29118568026193614 ) ) ;
#2369 = DIRECTION ( 'NONE',  ( -0.8090169943749474513, -2.183098979609982436E-16, 0.5877852522924731371 ) ) ;
#2370 = CARTESIAN_POINT ( 'NONE',  ( 28.52362724998032917, -7.841767518281756111, -12.14325827080317666 ) ) ;
#2371 = VERTEX_POINT ( 'NONE', #28802 ) ;
#2372 = FACE_OUTER_BOUND ( 'NONE', #25370, .T. ) ;
#2373 = CARTESIAN_POINT ( 'NONE',  ( 18.54205238286641588, 5.219565156008159512, -20.23764637224795848 ) ) ;
#2374 = CARTESIAN_POINT ( 'NONE',  ( 29.75294099516071711, -10.02427176990993196, -17.65830536592410738 ) ) ;
#2375 = VERTEX_POINT ( 'NONE', #18040 ) ;
#2376 = CARTESIAN_POINT ( 'NONE',  ( 8.373952262043122374, -5.000000000000015099, 25.77237501798157737 ) ) ;
#2377 = AXIS2_PLACEMENT_3D ( 'NONE', #19077, #24266, #16932 ) ;
#2378 = DIRECTION ( 'NONE',  ( 1.000000000000000000, 0.000000000000000000, 0.000000000000000000 ) ) ;
#2379 = DIRECTION ( 'NONE',  ( 0.3090169943749475623, 8.338696094058001131E-17, 0.9510565162951536422 ) ) ;
#2380 = AXIS2_PLACEMENT_3D ( 'NONE', #13272, #29968, #17691 ) ;
#2381 = CARTESIAN_POINT ( 'NONE',  ( 2.885073759410454741, -5.000000000000016875, 8.879344012873866987 ) ) ;
#2382 = EDGE_CURVE ( 'NONE', #14798, #28792, #12863, .T. ) ;
#2383 = CARTESIAN_POINT ( 'NONE',  ( 13.00000000000000178, 0.000000000000000000, 15.00000000000000000 ) ) ;
#2384 = EDGE_CURVE ( 'NONE', #18677, #7083, #18191, .T. ) ;
#2385 = CARTESIAN_POINT ( 'NONE',  ( 9.916824447075894611, 16.40553392900050156, -16.50439446175997205 ) ) ;
#2386 = VECTOR ( 'NONE', #10186, 1000.000000000000000 ) ;
#2387 = ADVANCED_FACE ( 'NONE', ( #8725 ), #10727, .F. ) ;
#2388 = CARTESIAN_POINT ( 'NONE',  ( 27.54556670433429488, -3.970347839692917713, -18.20727554117155123 ) ) ;
#2389 = CARTESIAN_POINT ( 'NONE',  ( 22.34648740292275093, -2.602002351270185532, -19.46322174391540116 ) ) ;
#2390 = CARTESIAN_POINT ( 'NONE',  ( 32.03687507811291368, -10.31171301082699543, -18.65038288416666390 ) ) ;
#2391 = AXIS2_PLACEMENT_3D ( 'NONE', #310, #18914, #21646 ) ;
#2392 = DIRECTION ( 'NONE',  ( -2.698458740408365879E-16, 1.000000000000000000, 0.000000000000000000 ) ) ;
#2393 = DIRECTION ( 'NONE',  ( -0.5877852522924731371, -1.586114251531760235E-16, 0.8090169943749474513 ) ) ;
#2394 = DIRECTION ( 'NONE',  ( -0.000000000000000000, -0.000000000000000000, 1.000000000000000000 ) ) ;
#2395 = CARTESIAN_POINT ( 'NONE',  ( 14.33367420948735393, 6.252843122977492563, -16.41390433006782956 ) ) ;
#2396 = ORIENTED_EDGE ( 'NONE', *, *, #11470, .T. ) ;
#2397 = DIRECTION ( 'NONE',  ( -2.698458740408365879E-16, 1.000000000000000000, 0.000000000000000000 ) ) ;
#2398 = CARTESIAN_POINT ( 'NONE',  ( 10.73095126193553028, 16.58460123524055874, -15.94999808000346242 ) ) ;
#2399 = ORIENTED_EDGE ( 'NONE', *, *, #29176, .T. ) ;
#2400 = CARTESIAN_POINT ( 'NONE',  ( 168.6922820468852819, -1.999999999999972244, -0.6060766987539614181 ) ) ;
#2401 = CARTESIAN_POINT ( 'NONE',  ( 13.00000000000001243, 55.00000000000000711, 18.00000000000000000 ) ) ;
#2402 = CARTESIAN_POINT ( 'NONE',  ( 18.88762249820254624, 5.002188274287570735, -13.90571046850145542 ) ) ;
#2403 = ORIENTED_EDGE ( 'NONE', *, *, #29649, .F. ) ;
#2404 = CARTESIAN_POINT ( 'NONE',  ( 13.70585326225313771, 5.953887885347688425, -14.73188983601744617 ) ) ;
#2405 = EDGE_LOOP ( 'NONE', ( #18466, #28383, #2939, #24172 ) ) ;
#2406 = CARTESIAN_POINT ( 'NONE',  ( 32.74140904187309786, -11.17293925747269867, -20.20304766317806866 ) ) ;
#2407 = VECTOR ( 'NONE', #8647, 1000.000000000000000 ) ;
#2408 = CARTESIAN_POINT ( 'NONE',  ( 23.40821609032294859, 1.473297984346819245, -16.37969033120859308 ) ) ;
#2409 = EDGE_LOOP ( 'NONE', ( #449, #9178, #16543, #29505 ) ) ;
#2410 = CARTESIAN_POINT ( 'NONE',  ( 15.92010713857317938, 6.231155140105813395, -20.15531274222559333 ) ) ;
#2411 =( GEOMETRIC_REPRESENTATION_CONTEXT ( 3 ) GLOBAL_UNCERTAINTY_ASSIGNED_CONTEXT ( ( #15606 ) ) GLOBAL_UNIT_ASSIGNED_CONTEXT ( ( #25786, #30262, #20888 ) ) REPRESENTATION_CONTEXT ( 'NONE', 'WORKASPACE' ) );
#2412 = CARTESIAN_POINT ( 'NONE',  ( 29.77493782482978091, -9.049732786019394126, -14.43420072379011643 ) ) ;
#2413 = EDGE_CURVE ( 'NONE', #28897, #6950, #1436, .T. ) ;
#2414 = VECTOR ( 'NONE', #22022, 1000.000000000000000 ) ;
#2415 = ORIENTED_EDGE ( 'NONE', *, *, #16103, .T. ) ;
#2416 = FACE_OUTER_BOUND ( 'NONE', #535, .T. ) ;
#2418 = ORIENTED_EDGE ( 'NONE', *, *, #16387, .T. ) ;
#2417 = DIRECTION ( 'NONE',  ( -1.000000000000000000, 0.000000000000000000, 0.000000000000000000 ) ) ;
#2419 = LINE ( 'NONE', #7283, #13858 ) ;
#2420 = EDGE_CURVE ( 'NONE', #4823, #2890, #25228, .T. ) ;
#2421 = FACE_OUTER_BOUND ( 'NONE', #19990, .T. ) ;
#2422 = CARTESIAN_POINT ( 'NONE',  ( 36.54645402898028550, -21.17490248391822050, -18.49223762587710951 ) ) ;
#2423 = VECTOR ( 'NONE', #22294, 1000.000000000000000 ) ;
#2424 = CARTESIAN_POINT ( 'NONE',  ( 12.75441094417786658, 7.625102360211175601, -14.92740490885063309 ) ) ;
#2425 = FACE_OUTER_BOUND ( 'NONE', #8742, .T. ) ;
#2426 = DIRECTION ( 'NONE',  ( -2.698458740408365879E-16, 1.000000000000000000, 0.000000000000000000 ) ) ;
#2427 = CARTESIAN_POINT ( 'NONE',  ( 10.35887147716723611, 16.97110557074245563, -17.87975733919941845 ) ) ;
#2428 = CARTESIAN_POINT ( 'NONE',  ( 20.00000000000017053, 34.64101615137744972, 14.00000000000000178 ) ) ;
#2429 = AXIS2_PLACEMENT_3D ( 'NONE', #8510, #15976, #10947 ) ;
#2430 = PLANE ( 'NONE',  #9028 ) ;
#2431 = VERTEX_POINT ( 'NONE', #27406 ) ;
#2432 = CARTESIAN_POINT ( 'NONE',  ( 153.6922820468853672, -4.999999999999976907, -6.413161187712876909 ) ) ;
#2433 = VERTEX_POINT ( 'NONE', #6457 ) ;
#2434 = LINE ( 'NONE', #19043, #19038 ) ;
#2435 = ORIENTED_EDGE ( 'NONE', *, *, #26498, .T. ) ;
#2436 = DIRECTION ( 'NONE',  ( 0.3090169943749472292, 8.338696094057992503E-17, -0.9510565162951536422 ) ) ;
#2437 = ORIENTED_EDGE ( 'NONE', *, *, #21004, .T. ) ;
#2438 = CARTESIAN_POINT ( 'NONE',  ( 10.31625730718771017, 13.25378293009361563, -17.61694433892753153 ) ) ;
#2439 = CARTESIAN_POINT ( 'NONE',  ( 24.47745745569867637, -8.908941985067972524, -13.71056886683244258 ) ) ;
#2440 = CARTESIAN_POINT ( 'NONE',  ( 25.07020310977553024, -1.264175079641418398, -16.65545549153034699 ) ) ;
#2441 = ORIENTED_EDGE ( 'NONE', *, *, #6056, .T. ) ;
#2442 = CARTESIAN_POINT ( 'NONE',  ( 19.82332968365342296, 2.432204761014481242, -19.52120720162773537 ) ) ;
#2443 = CARTESIAN_POINT ( 'NONE',  ( 12.35150960650664942, -5.000000000000014211, 38.01403777520749117 ) ) ;
#2444 = LINE ( 'NONE', #11721, #17476 ) ;
#2446 = DIRECTION ( 'NONE',  ( 1.000000000000000000, 2.891205793294675861E-16, 0.000000000000000000 ) ) ;
#2445 = STYLED_ITEM ( 'NONE', ( #18984 ), #16384 ) ;
#2447 = EDGE_CURVE ( 'NONE', #11751, #2343, #1893, .T. ) ;
#2448 = AXIS2_PLACEMENT_3D ( 'NONE', #4691, #5148, #23620 ) ;
#2449 = PRODUCT_RELATED_PRODUCT_CATEGORY ( 'part', '', ( #18122 ) ) ;
#2450 = CARTESIAN_POINT ( 'NONE',  ( 23.11440248821028831, -7.346120041196752659, -16.32852059634029018 ) ) ;
#2451 = ORIENTED_EDGE ( 'NONE', *, *, #24144, .F. ) ;
#2452 = VECTOR ( 'NONE', #1485, 1000.000000000000000 ) ;
#2453 = AXIS2_PLACEMENT_3D ( 'NONE', #15182, #26515, #5445 ) ;
#2454 = DIRECTION ( 'NONE',  ( 0.000000000000000000, -2.775557561562890735E-17, 1.000000000000000000 ) ) ;
#2455 = DIRECTION ( 'NONE',  ( 2.908569913943825554E-16, -1.000000000000000000, 0.000000000000000000 ) ) ;
#2456 = CARTESIAN_POINT ( 'NONE',  ( 109.1175021841459056, -4.999999999999987566, -79.27850588649985752 ) ) ;
#2457 = DIRECTION ( 'NONE',  ( 0.9510565162951536422, 2.566386769018988816E-16, 0.3090169943749472292 ) ) ;
#2458 = CARTESIAN_POINT ( 'NONE',  ( 10.35900481074863322, 16.97049408594186914, -17.87076805301065363 ) ) ;
#2459 = CARTESIAN_POINT ( 'NONE',  ( 0.000000000000000000, 0.000000000000000000, 0.000000000000000000 ) ) ;
#2460 = CARTESIAN_POINT ( 'NONE',  ( 32.67186286342521839, -11.06527230177895227, -18.43913201350460440 ) ) ;
#2461 = VERTEX_POINT ( 'NONE', #11174 ) ;
#2462 = CARTESIAN_POINT ( 'NONE',  ( 13.32639783386816212, 7.603689066773378968, -15.75018979827038912 ) ) ;
#2463 = ORIENTED_EDGE ( 'NONE', *, *, #18246, .F. ) ;
#2464 = DIRECTION ( 'NONE',  ( -2.698458740408365879E-16, 1.000000000000000000, 0.000000000000000000 ) ) ;
#2465 = CARTESIAN_POINT ( 'NONE',  ( 17.55424633453837302, 0.6138019359854992585, -14.89346452969079060 ) ) ;
#2466 = CARTESIAN_POINT ( 'NONE',  ( 11.27518382607279968, 16.68153699222178687, -16.78494985227356295 ) ) ;
#2467 = DIRECTION ( 'NONE',  ( 6.938893903907227392E-16, -0.000000000000000000, 1.000000000000000000 ) ) ;
#2468 = PRODUCT_DEFINITION_FORMATION_WITH_SPECIFIED_SOURCE ( 'ANY', '', #20070, .NOT_KNOWN. ) ;
#2469 = ORIENTED_EDGE ( 'NONE', *, *, #17041, .T. ) ;
#2470 = ORIENTED_EDGE ( 'NONE', *, *, #3402, .F. ) ;
#2471 = VERTEX_POINT ( 'NONE', #22637 ) ;
#2472 = CARTESIAN_POINT ( 'NONE',  ( 9.916953853453376766, 16.40494045485788632, -16.50434094533541085 ) ) ;
#2473 = CARTESIAN_POINT ( 'NONE',  ( 180.7287565553229456, -9.999999999999968026, -33.50000000000000000 ) ) ;
#2474 = VECTOR ( 'NONE', #28033, 1000.000000000000000 ) ;
#2475 = CARTESIAN_POINT ( 'NONE',  ( 9.915973561396301150, 16.40943619918981256, -16.50475030878699556 ) ) ;
#2476 = FACE_OUTER_BOUND ( 'NONE', #15120, .T. ) ;
#2477 = CARTESIAN_POINT ( 'NONE',  ( 17.59495141080627789, -5.000000000000013323, -54.15169229443701937 ) ) ;
#2478 = ORIENTED_EDGE ( 'NONE', *, *, #4864, .F. ) ;
#2479 = CARTESIAN_POINT ( 'NONE',  ( -2.000000000000032863, -3.464101615137743728, 8.673617379884035472E-16 ) ) ;
#2480 = ORIENTED_EDGE ( 'NONE', *, *, #3241, .T. ) ;
#2481 = CARTESIAN_POINT ( 'NONE',  ( 10.51251736658329961, 16.26646593658467310, -17.31805759646961462 ) ) ;
#2482 = EDGE_LOOP ( 'NONE', ( #907, #19784, #9447, #8535, #27642 ) ) ;
#2483 = CARTESIAN_POINT ( 'NONE',  ( 32.62421882425100961, -9.622687980317111922, -18.08031881573170097 ) ) ;
#2484 = CARTESIAN_POINT ( 'NONE',  ( 28.67486520862709654, -7.888541471525570614, -13.83454100519475105 ) ) ;
#2485 = ORIENTED_EDGE ( 'NONE', *, *, #29448, .F. ) ;
#2486 = CARTESIAN_POINT ( 'NONE',  ( 129.5152310637605808, -10.00000000000000888, -28.60870317832789311 ) ) ;
#2487 = ORIENTED_EDGE ( 'NONE', *, *, #13895, .T. ) ;
#2488 = CARTESIAN_POINT ( 'NONE',  ( 33.68917633736438688, -10.64779379647620949, -18.96437360758372748 ) ) ;
#2489 = VECTOR ( 'NONE', #1192, 1000.000000000000000 ) ;
#2490 = DIRECTION ( 'NONE',  ( 0.000000000000000000, 0.000000000000000000, 1.000000000000000000 ) ) ;
#2491 = EDGE_CURVE ( 'NONE', #25406, #23532, #15746, .T. ) ;
#2492 = ADVANCED_FACE ( 'NONE', ( #22176 ), #11021, .T. ) ;
#2493 = CARTESIAN_POINT ( 'NONE',  ( 17.64917075666736679, 6.165203978315560995, -14.56523922633501655 ) ) ;
#2494 = AXIS2_PLACEMENT_3D ( 'NONE', #19113, #21556, #22010 ) ;
#2495 = EDGE_CURVE ( 'NONE', #18617, #28674, #20327, .T. ) ;
#2496 = CARTESIAN_POINT ( 'NONE',  ( 28.11208967899271371, -8.897075463600188527, -14.13618326516971990 ) ) ;
#2497 = EDGE_CURVE ( 'NONE', #22465, #11088, #25074, .T. ) ;
#2498 = VERTEX_POINT ( 'NONE', #8285 ) ;
#2499 = FACE_BOUND ( 'NONE', #5350, .T. ) ;
#2500 = VECTOR ( 'NONE', #10038, 1000.000000000000000 ) ;
#2501 = LINE ( 'NONE', #23088, #18403 ) ;
#2502 = CARTESIAN_POINT ( 'NONE',  ( 164.5152310637604671, -1.999999999999971800, -21.71180489736091346 ) ) ;
#2503 = LINE ( 'NONE', #4471, #13383 ) ;
#2504 =( REPRESENTATION_RELATIONSHIP ('NONE','NONE', #5250, #16744 ) REPRESENTATION_RELATIONSHIP_WITH_TRANSFORMATION ( #12509 )SHAPE_REPRESENTATION_RELATIONSHIP( ) );
#2505 = CARTESIAN_POINT ( 'NONE',  ( 10.33841720888800531, 18.38481243897025053, -17.83974501271621449 ) ) ;
#2507 = CIRCLE ( 'NONE', #25899, 5.000000000000000888 ) ;
#2506 = CARTESIAN_POINT ( 'NONE',  ( 148.6922820468853956, -1.999999999999977129, -6.413161187712876909 ) ) ;
#2508 = LINE ( 'NONE', #16812, #28637 ) ;
#2509 = ORIENTED_EDGE ( 'NONE', *, *, #10773, .F. ) ;
#2510 = AXIS2_PLACEMENT_3D ( 'NONE', #5383, #24154, #3258 ) ;
#2511 = CARTESIAN_POINT ( 'NONE',  ( 9.917015787971365626, 16.40465641526357743, -16.50431533440121257 ) ) ;
#2512 = ORIENTED_EDGE ( 'NONE', *, *, #3444, .F. ) ;
#2513 = CARTESIAN_POINT ( 'NONE',  ( 15.27107031639597423, 6.121678041989828678, -18.36639460046777828 ) ) ;
#2514 = LINE ( 'NONE', #18355, #27847 ) ;
#2515 = CARTESIAN_POINT ( 'NONE',  ( 132.2287565553230024, -1.999999999999981348, -29.49038105676660138 ) ) ;
#2516 = CARTESIAN_POINT ( 'NONE',  ( 27.83100014064079275, -5.545984359997562230, -15.13782040115233052 ) ) ;
#2517 = EDGE_LOOP ( 'NONE', ( #10511, #28396, #2117, #6335 ) ) ;
#2518 = CARTESIAN_POINT ( 'NONE',  ( -13.00000000000000178, -2.870178842070716726E-15, -18.00000000000000000 ) ) ;
#2519 = CARTESIAN_POINT ( 'NONE',  ( 11.27518382607279968, 16.68153699222178687, -16.78494985227356295 ) ) ;
#2520 = ORIENTED_EDGE ( 'NONE', *, *, #15928, .F. ) ;
#2521 = CARTESIAN_POINT ( 'NONE',  ( 33.66044826391103584, -12.70207762650279015, -18.74488588032081893 ) ) ;
#2522 = CARTESIAN_POINT ( 'NONE',  ( 17.12833724908345800, 9.171387755021909172, -19.38714867094073213 ) ) ;
#2523 = VERTEX_POINT ( 'NONE', #29715 ) ;
#2524 = DIRECTION ( 'NONE',  ( 2.698458740408365879E-16, -1.000000000000000000, 0.000000000000000000 ) ) ;
#2525 = CARTESIAN_POINT ( 'NONE',  ( 25.29949251596307036, -5.094144391296384633, -13.01082609127739076 ) ) ;
#2526 = EDGE_LOOP ( 'NONE', ( #15705, #23448, #8859, #2157 ) ) ;
#2527 = CARTESIAN_POINT ( 'NONE',  ( 0.000000000000000000, 0.000000000000000000, -23.00000000000000000 ) ) ;
#2528 = CARTESIAN_POINT ( 'NONE',  ( 20.41927524488895429, 4.553956414902842198, -14.69105443414393264 ) ) ;
#2529 = CARTESIAN_POINT ( 'NONE',  ( 18.11961939296043056, 8.971021047410516758, -18.23824686698257125 ) ) ;
#2530 = EDGE_CURVE ( 'NONE', #14970, #1987, #4164, .T. ) ;
#2531 = ADVANCED_FACE ( 'NONE', ( #22786 ), #24936, .T. ) ;
#2532 = ORIENTED_EDGE ( 'NONE', *, *, #12787, .T. ) ;
#2533 = ORIENTED_EDGE ( 'NONE', *, *, #4361, .T. ) ;
#2534 = VECTOR ( 'NONE', #21135, 1000.000000000000000 ) ;
#2535 = DIRECTION ( 'NONE',  ( 1.110223024625156540E-16, 2.995891024602366092E-32, 1.000000000000000000 ) ) ;
#2536 = VECTOR ( 'NONE', #26811, 1000.000000000000000 ) ;
#2537 = LINE ( 'NONE', #22978, #3109 ) ;
#2538 = LINE ( 'NONE', #9669, #15388 ) ;
#2539 = LINE ( 'NONE', #26328, #5787 ) ;
#2540 = CARTESIAN_POINT ( 'NONE',  ( -8.000000000000000000, 0.000000000000000000, 9.999999999999998224 ) ) ;
#2541 = CARTESIAN_POINT ( 'NONE',  ( 9.917332382238186028, 16.40320447359955125, -16.50418441153501448 ) ) ;
#2542 = CARTESIAN_POINT ( 'NONE',  ( 20.32939975687981615, -5.674178230592766603, -17.16996371750385109 ) ) ;
#2543 = CARTESIAN_POINT ( 'NONE',  ( 21.84445237452005628, 0.7298858868756038509, -19.18266460542251295 ) ) ;
#2545 = EDGE_LOOP ( 'NONE', ( #28044, #17103, #25529, #13775 ) ) ;
#2544 = CARTESIAN_POINT ( 'NONE',  ( 30.54120030308987666, -10.08143909378498293, -14.42492330020037272 ) ) ;
#2546 = DIRECTION ( 'NONE',  ( -0.5877852522924731371, -1.586114251531760728E-16, -0.8090169943749474513 ) ) ;
#2547 = CARTESIAN_POINT ( 'NONE',  ( 13.04501788334644630, 8.811555337407297017, -14.69578613943112799 ) ) ;
#2548 = DIRECTION ( 'NONE',  ( 0.9510565162951536422, 2.566386769018988816E-16, 0.3090169943749472292 ) ) ;
#2549 = CARTESIAN_POINT ( 'NONE',  ( 142.0152310637606092, -10.00000000000000355, -15.61832212156129707 ) ) ;
#2550 = CARTESIAN_POINT ( 'NONE',  ( 17.08157517049449581, 7.460725202527481947, -14.57009041681831896 ) ) ;
#2551 = ORIENTED_EDGE ( 'NONE', *, *, #27803, .F. ) ;
#2552 = DIRECTION ( 'NONE',  ( 0.5877852522924731371, 1.586114251531760728E-16, -0.8090169943749474513 ) ) ;
#2553 = CARTESIAN_POINT ( 'NONE',  ( 10.33811693838771717, 18.38618951776012267, -17.91752729848688830 ) ) ;
#2554 = ORIENTED_EDGE ( 'NONE', *, *, #28546, .F. ) ;
#2555 = FACE_OUTER_BOUND ( 'NONE', #11801, .T. ) ;
#2556 = DIRECTION ( 'NONE',  ( 0.3090169943749475623, 8.338696094058001131E-17, 0.9510565162951536422 ) ) ;
#2557 = EDGE_CURVE ( 'NONE', #4895, #24305, #17735, .T. ) ;
#2558 = CARTESIAN_POINT ( 'NONE',  ( 14.17177033308128031, 6.273687421093853800, -17.36430109743762173 ) ) ;
#2559 = CARTESIAN_POINT ( 'NONE',  ( 25.32913879335529472, -12.33208189297920221, -17.76794973357399243 ) ) ;
#2560 = VERTEX_POINT ( 'NONE', #19881 ) ;
#2561 = CARTESIAN_POINT ( 'NONE',  ( 35.46335518829674527, -22.80158341140986167, -19.83799967047498924 ) ) ;
#2562 = CARTESIAN_POINT ( 'NONE',  ( 21.26848706961299129, -1.060808783303755387, -18.71231287479539063 ) ) ;
#2563 = CARTESIAN_POINT ( 'NONE',  ( 19.79992434292498515, 0.1278105412470878222, -19.37491769885296122 ) ) ;
#2564 = ADVANCED_FACE ( 'NONE', ( #29245 ), #13018, .T. ) ;
#2565 = EDGE_CURVE ( 'NONE', #26900, #9877, #22333, .T. ) ;
#2566 = EDGE_CURVE ( 'NONE', #17684, #10350, #6157, .T. ) ;
#2567 = CARTESIAN_POINT ( 'NONE',  ( 29.18140637672732396, -9.206484972055292815, -13.74645275385354815 ) ) ;
#2568 = VECTOR ( 'NONE', #22284, 1000.000000000000000 ) ;
#2569 = VERTEX_POINT ( 'NONE', #9635 ) ;
#2570 = CARTESIAN_POINT ( 'NONE',  ( 154.5152310637604955, -1.999999999999975353, -2.627941064794695691 ) ) ;
#2571 = DIRECTION ( 'NONE',  ( -0.000000000000000000, 0.000000000000000000, 1.000000000000000000 ) ) ;
#2572 = LINE ( 'NONE', #118, #27065 ) ;
#2573 = LINE ( 'NONE', #14280, #6842 ) ;
#2574 = CARTESIAN_POINT ( 'NONE',  ( 36.54859390953724585, -21.18451583373416014, -17.99055332684694974 ) ) ;
#2575 = CARTESIAN_POINT ( 'NONE',  ( 13.02821298986966703, 7.746099194123166498, -14.70917993614958519 ) ) ;
#2576 = EDGE_LOOP ( 'NONE', ( #27818, #13186, #3069, #25362 ) ) ;
#2577 = VECTOR ( 'NONE', #41, 1000.000000000000000 ) ;
#2578 = CARTESIAN_POINT ( 'NONE',  ( 137.2287565553230309, -1.999999999999979572, -29.49038105676660138 ) ) ;
#2579 = CARTESIAN_POINT ( 'NONE',  ( -20.00000000000017053, 34.64101615137744972, -10.00000000000000000 ) ) ;
#2580 = CARTESIAN_POINT ( 'NONE',  ( 10.47705880869930084, 16.42908340295556258, -17.33272095748315422 ) ) ;
#2581 = CARTESIAN_POINT ( 'NONE',  ( 94.27072269707019814, -4.999999999999992006, 68.49168918522173044 ) ) ;
#2582 = LINE ( 'NONE', #7142, #9582 ) ;
#2583 = ORIENTED_EDGE ( 'NONE', *, *, #22381, .F. ) ;
#2584 = DIRECTION ( 'NONE',  ( 0.000000000000000000, 0.000000000000000000, 1.000000000000000000 ) ) ;
#2585 = DIRECTION ( 'NONE',  ( 0.5877852522924731371, 0.000000000000000000, 0.8090169943749474513 ) ) ;
#2586 = CIRCLE ( 'NONE', #11332, 5.000000000000000888 ) ;
#2587 = LINE ( 'NONE', #30105, #14938 ) ;
#2588 = EDGE_LOOP ( 'NONE', ( #26292, #8509, #22302, #16171, #6464 ) ) ;
#2589 = CARTESIAN_POINT ( 'NONE',  ( 11.06190012440529102, 9.834169922982590961, -17.30859480447365328 ) ) ;
#2590 = CARTESIAN_POINT ( 'NONE',  ( 23.04322939705109974, -6.346999004730295546, -16.23111451206203881 ) ) ;
#2591 = CARTESIAN_POINT ( 'NONE',  ( 19.92565466131104301, 6.686648131885553958, -19.16379146452587179 ) ) ;
#2592 = DIRECTION ( 'NONE',  ( 1.000000000000000000, 2.698458740408365879E-16, -1.110223024625156540E-16 ) ) ;
#2593 = FACE_OUTER_BOUND ( 'NONE', #19222, .T. ) ;
#2594 = EDGE_CURVE ( 'NONE', #15731, #14637, #16047, .T. ) ;
#2595 = LINE ( 'NONE', #16612, #21057 ) ;
#2596 = EDGE_CURVE ( 'NONE', #2498, #5840, #13904, .T. ) ;
#2597 = CARTESIAN_POINT ( 'NONE',  ( 25.71553203045151292, -8.406338935355361031, -18.42709291467145150 ) ) ;
#2598 = DIRECTION ( 'NONE',  ( 1.000000000000000000, 2.908569913943825554E-16, -6.938893903907227392E-16 ) ) ;
#2599 = DIRECTION ( 'NONE',  ( -2.698458740408365879E-16, 1.000000000000000000, 0.000000000000000000 ) ) ;
#2600 = CARTESIAN_POINT ( 'NONE',  ( 175.7287565553229456, -4.999999999999970690, 3.500000000000003109 ) ) ;
#2601 = DIRECTION ( 'NONE',  ( 0.000000000000000000, -2.775557561562891351E-17, 1.000000000000000000 ) ) ;
#2602 = CARTESIAN_POINT ( 'NONE',  ( 159.7287565553230309, -4.999999999999974243, -33.82050807568879947 ) ) ;
#2603 = AXIS2_PLACEMENT_3D ( 'NONE', #20401, #18720, #4388 ) ;
#2604 = CARTESIAN_POINT ( 'NONE',  ( 10.50441255335269020, 16.30363564318377811, -17.32140922184415288 ) ) ;
#2605 = CARTESIAN_POINT ( 'NONE',  ( 151.1922820468854525, -4.999999999999976907, -28.06379628232387802 ) ) ;
#2606 = CARTESIAN_POINT ( 'NONE',  ( 33.17819505895439391, -11.78846528140086924, -19.49437495119144259 ) ) ;
#2607 = ORIENTED_EDGE ( 'NONE', *, *, #5320, .T. ) ;
#2608 = CARTESIAN_POINT ( 'NONE',  ( 8.944584683310379702, 16.95159276115599667, -17.92981046679734547 ) ) ;
#2609 = ORIENTED_EDGE ( 'NONE', *, *, #26221, .F. ) ;
#2610 = CARTESIAN_POINT ( 'NONE',  ( 148.6922820468853672, -1.999999999999977129, 2.247092850131519715 ) ) ;
#2611 = CARTESIAN_POINT ( 'NONE',  ( 21.41025690189560748, 5.821651141963339882, -16.00656683556521998 ) ) ;
#2612 = CARTESIAN_POINT ( 'NONE',  ( 11.26682494837019277, 16.71987187087499294, -16.78921452078379062 ) ) ;
#2613 = FACE_BOUND ( 'NONE', #4391, .T. ) ;
#2614 = ORIENTED_EDGE ( 'NONE', *, *, #4600, .F. ) ;
#2615 = EDGE_CURVE ( 'NONE', #12978, #22805, #14492, .T. ) ;
#2616 = ORIENTED_EDGE ( 'NONE', *, *, #27322, .F. ) ;
#2617 = CARTESIAN_POINT ( 'NONE',  ( 9.745779815811758340, 17.18996641109745482, -16.82979807527155458 ) ) ;
#2618 = CARTESIAN_POINT ( 'NONE',  ( 174.5152310637604671, -9.999999999999994671, -30.37205893520531319 ) ) ;
#2619 = CARTESIAN_POINT ( 'NONE',  ( 9.916336358462064737, 16.40777236560037622, -16.50459729666445696 ) ) ;
#2620 = LINE ( 'NONE', #29311, #4429 ) ;
#2621 = CARTESIAN_POINT ( 'NONE',  ( 2.000000000000008882, -3.464101615137750390, -2.450000000000000622 ) ) ;
#2622 = ORIENTED_EDGE ( 'NONE', *, *, #6057, .T. ) ;
#2623 = DIRECTION ( 'NONE',  ( -2.698458740408365879E-16, 1.000000000000000000, 0.000000000000000000 ) ) ;
#2624 = VERTEX_POINT ( 'NONE', #7362 ) ;
#2625 = CARTESIAN_POINT ( 'NONE',  ( 10.35867142355733783, 16.97202304209818990, -17.90451223021000260 ) ) ;
#2626 = VERTEX_POINT ( 'NONE', #28305 ) ;
#2627 = CARTESIAN_POINT ( 'NONE',  ( 36.30362226317071617, -21.08398799169651738, -20.22680612736627026 ) ) ;
#2628 = CARTESIAN_POINT ( 'NONE',  ( 15.57351372253994271, 10.71565324155555388, -15.28765949597478624 ) ) ;
#2629 = CARTESIAN_POINT ( 'NONE',  ( 26.58455406938135468, -5.910422570377376950, -13.89432871846328688 ) ) ;
#2630 = DIRECTION ( 'NONE',  ( -1.000000000000000000, -2.207829878515935943E-16, 0.000000000000000000 ) ) ;
#2631 = VECTOR ( 'NONE', #18990, 1000.000000000000000 ) ;
#2632 = DIRECTION ( 'NONE',  ( -2.698458740408365879E-16, 1.000000000000000000, 0.000000000000000000 ) ) ;
#2633 = CARTESIAN_POINT ( 'NONE',  ( 30.50415327504139285, -11.36213899161910135, -13.19862950667920565 ) ) ;
#2634 = CARTESIAN_POINT ( 'NONE',  ( 16.01392728624657025, 9.853228751548474662, -15.03783782146776105 ) ) ;
#2635 = VERTEX_POINT ( 'NONE', #2191 ) ;
#2636 = FACE_BOUND ( 'NONE', #7512, .T. ) ;
#2637 = EDGE_LOOP ( 'NONE', ( #6521, #20563, #29066, #15430, #7898, #13260 ) ) ;
#2638 = CARTESIAN_POINT ( 'NONE',  ( 0.000000000000000000, 4.350936251500947638E-16, 4.187999999999997058 ) ) ;
#2639 = LINE ( 'NONE', #14509, #17992 ) ;
#2640 = FACE_BOUND ( 'NONE', #22846, .T. ) ;
#2641 = AXIS2_PLACEMENT_3D ( 'NONE', #10040, #12327, #10194 ) ;
#2642 = CARTESIAN_POINT ( 'NONE',  ( 10.33816386007038268, 18.38597432894226458, -17.88535571907410571 ) ) ;
#2643 = DIRECTION ( 'NONE',  ( 0.9510565162951536422, 2.566386769018988816E-16, 0.3090169943749472292 ) ) ;
#2644 = EDGE_CURVE ( 'NONE', #4011, #6733, #9617, .T. ) ;
#2645 = EDGE_CURVE ( 'NONE', #28670, #1603, #12057, .T. ) ;
#2646 = CARTESIAN_POINT ( 'NONE',  ( 36.04859390953723874, -22.18451583373416014, -36.50100000000000477 ) ) ;
#2647 = ORIENTED_EDGE ( 'NONE', *, *, #442, .F. ) ;
#2648 = CARTESIAN_POINT ( 'NONE',  ( 11.47269659055779378, 9.270105954394804115, -15.86098659800193644 ) ) ;
#2649 = EDGE_CURVE ( 'NONE', #6067, #14522, #9326, .T. ) ;
#2650 = CARTESIAN_POINT ( 'NONE',  ( 9.668885350391278166, 16.22271324469333109, -17.88465541571617834 ) ) ;
#2651 = CARTESIAN_POINT ( 'NONE',  ( 18.87764716858279002, 3.471780965079254599, -19.68009874701989048 ) ) ;
#2652 = DIRECTION ( 'NONE',  ( 0.5877852522924731371, 1.586114251531760728E-16, -0.8090169943749474513 ) ) ;
#2653 = FACE_OUTER_BOUND ( 'NONE', #5134, .T. ) ;
#2654 = CARTESIAN_POINT ( 'NONE',  ( 25.24878800877705487, -9.370948223588685622, -14.18615728435988288 ) ) ;
#2655 = PLANE ( 'NONE',  #28635 ) ;
#2656 = CARTESIAN_POINT ( 'NONE',  ( 11.05818223728759264, 17.67673393965927175, -17.74095938596937572 ) ) ;
#2657 = ORIENTED_EDGE ( 'NONE', *, *, #6571, .F. ) ;
#2658 = CARTESIAN_POINT ( 'NONE',  ( 35.54859390953724585, -21.18451583373416014, -18.06010107863414405 ) ) ;
#2659 = CARTESIAN_POINT ( 'NONE',  ( 154.7287565553229172, -1.999999999999975353, -16.50000000000000000 ) ) ;
#2660 = LINE ( 'NONE', #11793, #27223 ) ;
#2661 = CARTESIAN_POINT ( 'NONE',  ( 22.52525573827019301, -5.869110285238294367, -18.12586539066504798 ) ) ;
#2662 = EDGE_LOOP ( 'NONE', ( #12047, #2609 ) ) ;
#2663 = DIRECTION ( 'NONE',  ( 0.5877852522924731371, 1.586114251531760728E-16, -0.8090169943749474513 ) ) ;
#2664 = CARTESIAN_POINT ( 'NONE',  ( 21.50147616854745891, 4.214167280306792662, -18.19698480873994839 ) ) ;
#2665 = CARTESIAN_POINT ( 'NONE',  ( 17.93652952100233833, 4.843921488302829204, -14.86957952233187896 ) ) ;
#2666 = VECTOR ( 'NONE', #11845, 1000.000000000000000 ) ;
#2667 = ORIENTED_EDGE ( 'NONE', *, *, #11288, .T. ) ;
#2668 = DIRECTION ( 'NONE',  ( -0.9510565162951536422, -2.566386769018988816E-16, -0.3090169943749472292 ) ) ;
#2669 = LINE ( 'NONE', #21271, #24065 ) ;
#2670 = LINE ( 'NONE', #25714, #12468 ) ;
#2671 = CARTESIAN_POINT ( 'NONE',  ( 164.7287565553228887, -1.999999999999972689, 0.8205080756887930260 ) ) ;
#2672 = CARTESIAN_POINT ( 'NONE',  ( 0.000000000000000000, 2.099999999999997868, 1.700000000000000178 ) ) ;
#2673 = CARTESIAN_POINT ( 'NONE',  ( 9.641351021852148762, 17.66889017177091503, -17.91406276888456617 ) ) ;
#2674 = CARTESIAN_POINT ( 'NONE',  ( 21.89112544314524200, -5.209854132323804343, -13.34451667507982364 ) ) ;
#2675 = CARTESIAN_POINT ( 'NONE',  ( 19.87821071931953298, -1.530402839103173651, -15.12151443550766494 ) ) ;
#2676 = EDGE_CURVE ( 'NONE', #10978, #24619, #21087, .T. ) ;
#2678 = ORIENTED_EDGE ( 'NONE', *, *, #23481, .T. ) ;
#2677 = CARTESIAN_POINT ( 'NONE',  ( 31.74553205326546390, -10.26435202779689604, -17.82876124730869805 ) ) ;
#2679 = CARTESIAN_POINT ( 'NONE',  ( 49.00000000000000000, 0.000000000000000000, 0.000000000000000000 ) ) ;
#2680 = CARTESIAN_POINT ( 'NONE',  ( 12.63667343406881294, 8.631100619704961119, -15.02124387326777111 ) ) ;
#2681 = EDGE_CURVE ( 'NONE', #10405, #10807, #2501, .T. ) ;
#2682 = VECTOR ( 'NONE', #25076, 1000.000000000000000 ) ;
#2683 = DIRECTION ( 'NONE',  ( -0.9510565162951536422, -2.566386769018988323E-16, 0.3090169943749475623 ) ) ;
#2684 = CARTESIAN_POINT ( 'NONE',  ( 151.1922820468854241, -1.999999999999975797, -22.25671179336496053 ) ) ;
#2685 = EDGE_CURVE ( 'NONE', #2433, #14962, #875, .T. ) ;
#2686 = CARTESIAN_POINT ( 'NONE',  ( 149.5152310637605524, -1.999999999999975797, -21.71180489736091346 ) ) ;
#2687 = ORIENTED_EDGE ( 'NONE', *, *, #16523, .T. ) ;
#2688 = DIRECTION ( 'NONE',  ( -0.5877852522924731371, -1.586114251531760235E-16, 0.8090169943749474513 ) ) ;
#2689 = CARTESIAN_POINT ( 'NONE',  ( 10.33811693838771717, 18.38618951776012267, -17.91664992932185996 ) ) ;
#2690 = ORIENTED_EDGE ( 'NONE', *, *, #19611, .F. ) ;
#2691 = DIRECTION ( 'NONE',  ( 6.938893903907226800E-15, 0.000000000000000000, -1.000000000000000000 ) ) ;
#2692 = LINE ( 'NONE', #2848, #19554 ) ;
#2693 = CARTESIAN_POINT ( 'NONE',  ( 21.04385110482095200, 5.766204710259658306, -15.30406332615466347 ) ) ;
#2694 = VERTEX_POINT ( 'NONE', #23383 ) ;
#2695 = CARTESIAN_POINT ( 'NONE',  ( 25.72097854023329688, -11.95459465090917917, -18.51508836554082293 ) ) ;
#2696 = EDGE_LOOP ( 'NONE', ( #19357, #4464, #18008, #2308 ) ) ;
#2697 = CARTESIAN_POINT ( 'NONE',  ( 35.54859215833182873, -22.18450796649496226, -18.40462262104107083 ) ) ;
#2698 = CARTESIAN_POINT ( 'NONE',  ( 23.33644427035094537, 1.513498076802863190, -16.07814869553001103 ) ) ;
#2699 = CARTESIAN_POINT ( 'NONE',  ( 19.19659130220728116, 4.347481709847851761, -15.16398724834160916 ) ) ;
#2700 = ORIENTED_EDGE ( 'NONE', *, *, #23049, .F. ) ;
#2701 = CARTESIAN_POINT ( 'NONE',  ( 28.07139740185986199, -11.61962552671339388, -17.78409693965565452 ) ) ;
#2702 = VECTOR ( 'NONE', #24441, 1000.000000000000000 ) ;
#2703 = ORIENTED_EDGE ( 'NONE', *, *, #27450, .T. ) ;
#2704 = DIRECTION ( 'NONE',  ( 1.110223024625156540E-16, 2.995891024602366092E-32, 1.000000000000000000 ) ) ;
#2706 = VERTEX_POINT ( 'NONE', #9172 ) ;
#2705 = CARTESIAN_POINT ( 'NONE',  ( 164.5152310637604671, -9.999999999999998224, -2.627941064794695691 ) ) ;
#2707 = LINE ( 'NONE', #16587, #24077 ) ;
#2708 = DIRECTION ( 'NONE',  ( 0.000000000000000000, 1.000000000000000000, -1.471414886128461471E-15 ) ) ;
#2709 = AXIS2_PLACEMENT_3D ( 'NONE', #6808, #2394, #20675 ) ;
#2710 = CARTESIAN_POINT ( 'NONE',  ( 36.54859286093297754, -21.18451112290966165, -18.39168789611893118 ) ) ;
#2711 = CARTESIAN_POINT ( 'NONE',  ( 12.76449053303042902, 7.629555522264023892, -14.91937138927071160 ) ) ;
#2712 = VERTEX_POINT ( 'NONE', #11321 ) ;
#2713 = EDGE_CURVE ( 'NONE', #11968, #18587, #27852, .T. ) ;
#2714 = FACE_OUTER_BOUND ( 'NONE', #8518, .T. ) ;
#2715 = CARTESIAN_POINT ( 'NONE',  ( 153.6922820468854241, -1.999999999999975797, -23.73366926340167282 ) ) ;
#2716 = ADVANCED_FACE ( 'NONE', ( #30009 ), #23229, .T. ) ;
#2717 = EDGE_CURVE ( 'NONE', #968, #26624, #2344, .T. ) ;
#2718 = CARTESIAN_POINT ( 'NONE',  ( 11.96327893486549776, 9.613088455355432771, -16.71811665443363992 ) ) ;
#2719 = LINE ( 'NONE', #2581, #19985 ) ;
#2720 = ADVANCED_FACE ( 'NONE', ( #16505 ), #28155, .T. ) ;
#2721 = EDGE_LOOP ( 'NONE', ( #26013, #24206, #27600, #14580 ) ) ;
#2722 = FACE_OUTER_BOUND ( 'NONE', #25105, .T. ) ;
#2723 = VERTEX_POINT ( 'NONE', #23535 ) ;
#2724 = CIRCLE ( 'NONE', #18374, 9.000000000000007105 ) ;
#2725 = CARTESIAN_POINT ( 'NONE',  ( 142.2287565553230024, -10.00000000000000533, -3.509618943233403510 ) ) ;
#2726 = CARTESIAN_POINT ( 'NONE',  ( 14.02072799663827141, -5.000000000000014211, 43.15136373446576101 ) ) ;
#2727 = ORIENTED_EDGE ( 'NONE', *, *, #11512, .F. ) ;
#2728 = ORIENTED_EDGE ( 'NONE', *, *, #18823, .T. ) ;
#2729 = CARTESIAN_POINT ( 'NONE',  ( 2.500000000000000444, -1.178949249685215417, 2.042000000000002036 ) ) ;
#2730 = ORIENTED_EDGE ( 'NONE', *, *, #21680, .T. ) ;
#2731 = CARTESIAN_POINT ( 'NONE',  ( 9.671924655352764688, 16.20877460471870535, -17.88339855620073848 ) ) ;
#2732 = VERTEX_POINT ( 'NONE', #27700 ) ;
#2733 = CARTESIAN_POINT ( 'NONE',  ( 27.30941123812745275, -4.721684434479056947, -15.35818731037458029 ) ) ;
#2734 = CARTESIAN_POINT ( 'NONE',  ( 23.93603600111211804, 0.1510904554606163908, -14.93755387302875448 ) ) ;
#2735 = LINE ( 'NONE', #4709, #20367 ) ;
#2736 = DIRECTION ( 'NONE',  ( 1.000000000000000000, 2.698458740408365879E-16, -1.110223024625156540E-16 ) ) ;
#2737 = CARTESIAN_POINT ( 'NONE',  ( 143.6922820468854525, -1.999999999999978018, -26.58683881228715506 ) ) ;
#2738 = CARTESIAN_POINT ( 'NONE',  ( 25.04992766293576878, -3.547109489677171101, -13.67097983722207033 ) ) ;
#2739 = VECTOR ( 'NONE', #10171, 1000.000000000000000 ) ;
#2740 = ORIENTED_EDGE ( 'NONE', *, *, #23334, .T. ) ;
#2741 = VERTEX_POINT ( 'NONE', #2638 ) ;
#2742 = SURFACE_STYLE_USAGE ( .BOTH. , #27809 ) ;
#2743 = DIRECTION ( 'NONE',  ( -0.000000000000000000, 0.000000000000000000, 1.000000000000000000 ) ) ;
#2744 = DIRECTION ( 'NONE',  ( -2.698458740408365879E-16, 1.000000000000000000, 0.000000000000000000 ) ) ;
#2745 = CIRCLE ( 'NONE', #1287, 8.000000000000000000 ) ;
#2746 = LINE ( 'NONE', #20889, #499 ) ;
#2748 = LINE ( 'NONE', #306, #11872 ) ;
#2747 = VECTOR ( 'NONE', #6423, 1000.000000000000000 ) ;
#2749 = CARTESIAN_POINT ( 'NONE',  ( 12.01190781424926435, 9.390070215761314287, -16.69800690218674788 ) ) ;
#2750 = CARTESIAN_POINT ( 'NONE',  ( 125.7287565553229456, -84.33034373659255323, -33.50000000000000000 ) ) ;
#2751 = CARTESIAN_POINT ( 'NONE',  ( 32.48283477683061449, -11.02614750807341260, -17.91093295056291979 ) ) ;
#2752 = ORIENTED_EDGE ( 'NONE', *, *, #13723, .T. ) ;
#2753 = CARTESIAN_POINT ( 'NONE',  ( 8.944584683310379702, 16.95159276115599667, -17.98596209335946128 ) ) ;
#2754 = VERTEX_POINT ( 'NONE', #7060 ) ;
#2755 = EDGE_CURVE ( 'NONE', #14083, #2431, #16352, .T. ) ;
#2756 = DIRECTION ( 'NONE',  ( -1.000000000000000000, -4.440892098500622217E-16, 0.000000000000000000 ) ) ;
#2757 = CARTESIAN_POINT ( 'NONE',  ( 18.88762249820254624, 5.002188274287570735, -13.90571046850145542 ) ) ;
#2758 = ADVANCED_FACE ( 'NONE', ( #196 ), #9476, .T. ) ;
#2759 = CARTESIAN_POINT ( 'NONE',  ( 12.84002880955021197, 9.524163120117652426, -16.13635871874149430 ) ) ;
#2760 = PLANE ( 'NONE',  #21921 ) ;
#2761 = ADVANCED_FACE ( 'NONE', ( #11915 ), #348, .T. ) ;
#2762 = ORIENTED_EDGE ( 'NONE', *, *, #15166, .F. ) ;
#2763 = ORIENTED_EDGE ( 'NONE', *, *, #13385, .F. ) ;
#2764 = ORIENTED_EDGE ( 'NONE', *, *, #5295, .F. ) ;
#2765 = CARTESIAN_POINT ( 'NONE',  ( 9.912057827679275235, 16.42739425315605928, -16.50652470164456531 ) ) ;
#2766 = PLANE ( 'NONE',  #14007 ) ;
#2767 = VECTOR ( 'NONE', #26977, 1000.000000000000000 ) ;
#2768 = CARTESIAN_POINT ( 'NONE',  ( 9.921764701973689426, 16.38287729030320250, -16.50235149140834778 ) ) ;
#2769 = LINE ( 'NONE', #12052, #865 ) ;
#2770 = VERTEX_POINT ( 'NONE', #1105 ) ;
#2771 = CARTESIAN_POINT ( 'NONE',  ( 149.5152310637605524, -4.999999999999976907, -11.28819510263909542 ) ) ;
#2772 = VERTEX_POINT ( 'NONE', #7505 ) ;
#2773 = CARTESIAN_POINT ( 'NONE',  ( 10.35865057885519214, 16.97211863855931924, -17.91295731025335414 ) ) ;
#2774 = VERTEX_POINT ( 'NONE', #14801 ) ;
#2776 = CARTESIAN_POINT ( 'NONE',  ( 36.54859390953724585, -22.18451583373416014, -16.94733705004010460 ) ) ;
#2775 = VECTOR ( 'NONE', #28779, 1000.000000000000000 ) ;
#2777 = CARTESIAN_POINT ( 'NONE',  ( 26.32595758385100382, -12.12905223104374386, -14.21117607008287642 ) ) ;
#2778 = CARTESIAN_POINT ( 'NONE',  ( 14.76280285026742867, 7.190900411307756812, -14.35234371774122408 ) ) ;
#2779 = VECTOR ( 'NONE', #18607, 1000.000000000000000 ) ;
#2780 = CARTESIAN_POINT ( 'NONE',  ( 148.6922820468853672, -1.999999999999977573, -0.6060766987539614181 ) ) ;
#2781 = CARTESIAN_POINT ( 'NONE',  ( 33.40535544545146251, -10.40465400369240356, -18.27852168438239389 ) ) ;
#2782 = APPLICATION_PROTOCOL_DEFINITION ( 'draft international standard', 'automotive_design', 1998, #26069 ) ;
#2783 = CARTESIAN_POINT ( 'NONE',  ( 15.50826552155665183, 8.864470348925614474, -13.64319937614855149 ) ) ;
#2784 = CARTESIAN_POINT ( 'NONE',  ( 25.57659404178318141, -9.842204813007603192, -16.83936284125123706 ) ) ;
#2785 = ORIENTED_EDGE ( 'NONE', *, *, #16826, .F. ) ;
#2786 = EDGE_CURVE ( 'NONE', #26001, #27081, #5060, .T. ) ;
#2787 = CARTESIAN_POINT ( 'NONE',  ( 169.7287565553229172, -9.999999999999996447, -16.50000000000000355 ) ) ;
#2788 = CIRCLE ( 'NONE', #23227, 5.000000000000000000 ) ;
#2789 = DIRECTION ( 'NONE',  ( -0.8191520442889902442, -3.637765840953607804E-16, -0.5735764363510482688 ) ) ;
#2790 = CARTESIAN_POINT ( 'NONE',  ( 139.7287565553230309, -10.00000000000000533, -25.16025403784439973 ) ) ;
#2791 = CARTESIAN_POINT ( 'NONE',  ( -8.000000000000003553, -4.618802153517028941, -5.000000000000000888 ) ) ;
#2792 = VECTOR ( 'NONE', #29034, 1000.000000000000000 ) ;
#2793 = DIRECTION ( 'NONE',  ( -0.000000000000000000, 0.000000000000000000, 1.000000000000000000 ) ) ;
#2794 = AXIS2_PLACEMENT_3D ( 'NONE', #3031, #11856, #23622 ) ;
#2795 = UNCERTAINTY_MEASURE_WITH_UNIT (LENGTH_MEASURE( 1.000000000000000082E-05 ), #28013, 'distance_accuracy_value', 'NONE');
#2796 = B_SPLINE_CURVE_WITH_KNOTS ( 'NONE', 3,
 ( #15773, #25099, #13485, #11346, #24962, #29892 ),
 .UNSPECIFIED., .F., .F.,
 ( 4, 2, 4 ),
 ( 0.01291313371729459203, 0.01525081363757311605, 0.01758849355785164006 ),
 .UNSPECIFIED. ) ;
#2797 = CARTESIAN_POINT ( 'NONE',  ( 10.72094366404044408, 16.63049735485946101, -15.95413657539408980 ) ) ;
#2798 = CARTESIAN_POINT ( 'NONE',  ( 154.5152310637605808, -1.999999999999974021, -28.60870317832789667 ) ) ;
#2799 = ORIENTED_EDGE ( 'NONE', *, *, #16998, .F. ) ;
#2800 = CARTESIAN_POINT ( 'NONE',  ( 172.0152310637604387, -1.999999999999970024, -17.38167787843871182 ) ) ;
#2801 = ORIENTED_EDGE ( 'NONE', *, *, #647, .T. ) ;
#2802 = CARTESIAN_POINT ( 'NONE',  ( 9.915248083523094280, 16.41276333319327918, -16.50506225043874409 ) ) ;
#2803 = ORIENTED_EDGE ( 'NONE', *, *, #2420, .T. ) ;
#2804 = CARTESIAN_POINT ( 'NONE',  ( 9.666286124033039329, 16.23463362809610899, -17.88661257689534878 ) ) ;
#2805 = CARTESIAN_POINT ( 'NONE',  ( 18.15277384750198308, 2.816914934748806054, -19.48283598520044180 ) ) ;
#2806 = DIRECTION ( 'NONE',  ( 0.5877852522924731371, 0.000000000000000000, 0.8090169943749474513 ) ) ;
#2807 = CARTESIAN_POINT ( 'NONE',  ( 29.62588713853392264, -10.65184931322849060, -12.76488833982454629 ) ) ;
#2808 = ORIENTED_EDGE ( 'NONE', *, *, #1630, .F. ) ;
#2809 = CARTESIAN_POINT ( 'NONE',  ( 133.6922820468854241, -10.00000000000000711, -6.413161187712875133 ) ) ;
#2810 = CARTESIAN_POINT ( 'NONE',  ( 11.27425361364269563, 16.68580306500076915, -16.78535843524344173 ) ) ;
#2811 = ORIENTED_EDGE ( 'NONE', *, *, #7531, .T. ) ;
#2812 = CARTESIAN_POINT ( 'NONE',  ( 33.71394559998177698, -12.94241281914233355, -18.76105684162217457 ) ) ;
#2813 = CARTESIAN_POINT ( 'NONE',  ( 20.24985932600369409, 3.694099309552050237, -20.13309853732883781 ) ) ;
#2814 = VECTOR ( 'NONE', #27532, 1000.000000000000000 ) ;
#2815 = CARTESIAN_POINT ( 'NONE',  ( 133.6922820468854241, -4.999999999999981348, -26.58683881228715506 ) ) ;
#2816 = CARTESIAN_POINT ( 'NONE',  ( 8.952973202525470242, 16.91312194274802749, -17.65238394630757313 ) ) ;
#2817 = CARTESIAN_POINT ( 'NONE',  ( 30.91631662189391250, -8.208988707411489116, -18.28093047724294351 ) ) ;
#2818 = VERTEX_POINT ( 'NONE', #28455 ) ;
#2819 = DIRECTION ( 'NONE',  ( 0.000000000000000000, 0.000000000000000000, 1.000000000000000000 ) ) ;
#2820 = CARTESIAN_POINT ( 'NONE',  ( 18.63710449947919301, 3.826706299981984305, -14.11708861520305192 ) ) ;
#2821 = AXIS2_PLACEMENT_3D ( 'NONE', #15628, #6628, #8900 ) ;
#2822 = CARTESIAN_POINT ( 'NONE',  ( 15.60359850163179551, 6.442352727238609411, -18.97839103356167101 ) ) ;
#2823 = DIRECTION ( 'NONE',  ( -0.5877852522924731371, 0.000000000000000000, 0.8090169943749474513 ) ) ;
#2824 = EDGE_LOOP ( 'NONE', ( #1513, #5546, #4035, #7617, #25091 ) ) ;
#2825 = ORIENTED_EDGE ( 'NONE', *, *, #5895, .T. ) ;
#2826 = EDGE_CURVE ( 'NONE', #4536, #3628, #9783, .T. ) ;
#2827 = PLANE ( 'NONE',  #27440 ) ;
#2828 = DIRECTION ( 'NONE',  ( 0.9510565162951536422, 0.000000000000000000, -0.3090169943749475623 ) ) ;
#2829 = CARTESIAN_POINT ( 'NONE',  ( 2.000000000000026201, 3.464101615137736623, -2.450000000000000622 ) ) ;
#2830 = DIRECTION ( 'NONE',  ( 1.000000000000000000, 2.168404344971006896E-16, 0.000000000000000000 ) ) ;
#2831 = FACE_OUTER_BOUND ( 'NONE', #8191, .T. ) ;
#2832 = CIRCLE ( 'NONE', #11552, 5.000000000000006217 ) ;
#2833 = CARTESIAN_POINT ( 'NONE',  ( 9.641350810849047548, 17.66889113945805789, -17.91664992932186351 ) ) ;
#2834 = CARTESIAN_POINT ( 'NONE',  ( 25.27624414898354388, -7.528478751523516088, -13.47981680254768655 ) ) ;
#2835 = CARTESIAN_POINT ( 'NONE',  ( 24.59961324288297391, 0.2024632608770970121, -16.27125138369466484 ) ) ;
#2837 = ORIENTED_EDGE ( 'NONE', *, *, #10306, .F. ) ;
#2836 = CARTESIAN_POINT ( 'NONE',  ( 31.02293300316137348, -10.15460426738793664, -15.78645847904462052 ) ) ;
#2838 = CARTESIAN_POINT ( 'NONE',  ( 0.000000000000000000, 0.000000000000000000, 18.00000000000000000 ) ) ;
#2839 = AXIS2_PLACEMENT_3D ( 'NONE', #16651, #28295, #11604 ) ;
#2840 = DIRECTION ( 'NONE',  ( 0.3090169943749475623, 8.338696094058001131E-17, 0.9510565162951536422 ) ) ;
#2841 = CARTESIAN_POINT ( 'NONE',  ( 169.7287565553229172, -9.999999999999996447, -16.50000000000000355 ) ) ;
#2842 = DIRECTION ( 'NONE',  ( -2.698458740408365879E-16, 1.000000000000000000, 0.000000000000000000 ) ) ;
#2843 = CARTESIAN_POINT ( 'NONE',  ( 14.18486973814142793, 6.324582201221724098, -17.68508340245422872 ) ) ;
#2844 = EDGE_LOOP ( 'NONE', ( #9643, #26462, #23724, #7699 ) ) ;
#2845 = DIRECTION ( 'NONE',  ( 0.000000000000000000, 0.7071067811865462405, -0.7071067811865489050 ) ) ;
#2846 = CARTESIAN_POINT ( 'NONE',  ( 10.72061166913284325, 16.63201992582523658, -15.95427402900266856 ) ) ;
#2847 = CARTESIAN_POINT ( 'NONE',  ( 153.6922820468853388, -1.999999999999976241, -0.6060766987539614181 ) ) ;
#2848 = CARTESIAN_POINT ( 'NONE',  ( 129.5152310637605524, -10.00000000000000888, -30.37205893520530964 ) ) ;
#2849 = VERTEX_POINT ( 'NONE', #8092 ) ;
#2850 = CARTESIAN_POINT ( 'NONE',  ( 15.22033579473957410, 7.355362781181614018, -19.64495939069069763 ) ) ;
#2851 = CARTESIAN_POINT ( 'NONE',  ( 26.55477173981947914, -11.17418396328012342, -19.38009549175560053 ) ) ;
#2852 = ORIENTED_EDGE ( 'NONE', *, *, #20783, .T. ) ;
#2853 = CARTESIAN_POINT ( 'NONE',  ( 32.54305136433941215, -11.03529315477374517, -18.08112484791816499 ) ) ;
#2854 = CARTESIAN_POINT ( 'NONE',  ( 23.72730982194951466, -1.509008702439352589, -18.09242500859757996 ) ) ;
#2855 = CARTESIAN_POINT ( 'NONE',  ( 18.47998620531167902, -1.197692507188573785, -16.87724725366775402 ) ) ;
#2856 = CIRCLE ( 'NONE', #14517, 4.000000000000000000 ) ;
#2857 = CARTESIAN_POINT ( 'NONE',  ( 29.53935142057454755, -5.962610374456907003, -16.12847026952743690 ) ) ;
#2858 = ADVANCED_FACE ( 'NONE', ( #19098 ), #25984, .T. ) ;
#2859 = EDGE_CURVE ( 'NONE', #7377, #1843, #14351, .T. ) ;
#2860 = VECTOR ( 'NONE', #24545, 1000.000000000000000 ) ;
#2861 = EDGE_CURVE ( 'NONE', #14702, #25081, #21996, .T. ) ;
#2862 = EDGE_LOOP ( 'NONE', ( #22736, #7896, #25769, #21484, #4484, #9143 ) ) ;
#2863 = EDGE_CURVE ( 'NONE', #7345, #8301, #5214, .T. ) ;
#2864 = DIRECTION ( 'NONE',  ( -0.5877852522924731371, -1.586114251531760235E-16, 0.8090169943749474513 ) ) ;
#2865 = VECTOR ( 'NONE', #597, 1000.000000000000000 ) ;
#2867 = ORIENTED_EDGE ( 'NONE', *, *, #3241, .F. ) ;
#2866 = PLANE ( 'NONE',  #29779 ) ;
#2868 = LINE ( 'NONE', #23771, #19216 ) ;
#2869 = DIRECTION ( 'NONE',  ( 0.3090169943749475623, 8.338696094058001131E-17, 0.9510565162951536422 ) ) ;
#2870 = CARTESIAN_POINT ( 'NONE',  ( 36.54859390954302967, -21.18451583373416014, -15.55638201429745848 ) ) ;
#2871 = CARTESIAN_POINT ( 'NONE',  ( 9.649959050778257108, 17.62941265384766254, -17.56860460898032628 ) ) ;
#2872 = PLANE ( 'NONE',  #20969 ) ;
#2873 = LINE ( 'NONE', #10012, #5127 ) ;
#2874 = CARTESIAN_POINT ( 'NONE',  ( 12.03006260835556951, 9.306948544855226046, -16.69048869075990638 ) ) ;
#2875 = DIRECTION ( 'NONE',  ( -2.698458740408365879E-16, 1.000000000000000000, 0.000000000000000000 ) ) ;
#2876 = ORIENTED_EDGE ( 'NONE', *, *, #5634, .F. ) ;
#2877 = CARTESIAN_POINT ( 'NONE',  ( 0.000000000000000000, 0.000000000000000000, -15.00000000000000000 ) ) ;
#2878 = VERTEX_POINT ( 'NONE', #16805 ) ;
#2879 = VECTOR ( 'NONE', #21888, 1000.000000000000000 ) ;
#2880 = LINE ( 'NONE', #14290, #25154 ) ;
#2881 = DIRECTION ( 'NONE',  ( 0.000000000000000000, 0.000000000000000000, 1.000000000000000000 ) ) ;
#2882 = ORIENTED_EDGE ( 'NONE', *, *, #11285, .T. ) ;
#2883 = CARTESIAN_POINT ( 'NONE',  ( 147.2287565553230309, -4.999999999999977796, -20.83012701892220164 ) ) ;
#2884 = AXIS2_PLACEMENT_3D ( 'NONE', #12421, #15005, #22044 ) ;
#2885 = ORIENTED_EDGE ( 'NONE', *, *, #5510, .T. ) ;
#2886 = CARTESIAN_POINT ( 'NONE',  ( 13.37720302390605553, 7.624891072754538257, -15.70979247928349132 ) ) ;
#2887 = ADVANCED_FACE ( 'NONE', ( #498 ), #18904, .T. ) ;
#2888 = AXIS2_PLACEMENT_3D ( 'NONE', #6881, #16169, #25492 ) ;
#2889 = CARTESIAN_POINT ( 'NONE',  ( 25.37470919123784086, -4.075530507763302168, -17.99687124876041011 ) ) ;
#2890 = VERTEX_POINT ( 'NONE', #5372 ) ;
#2891 = CARTESIAN_POINT ( 'NONE',  ( 21.59786356094703308, -0.7637721020719707710, -13.97513905925265298 ) ) ;
#2892 = CARTESIAN_POINT ( 'NONE',  ( 0.000000000000000000, 0.000000000000000000, 0.000000000000000000 ) ) ;
#2893 = LINE ( 'NONE', #1058, #28725 ) ;
#2894 = CARTESIAN_POINT ( 'NONE',  ( -8.000000000000003553, -4.618802153517037823, -0.7145311798163362926 ) ) ;
#2895 = EDGE_CURVE ( 'NONE', #8851, #3493, #22818, .T. ) ;
#2896 = EDGE_CURVE ( 'NONE', #11499, #983, #12520, .T. ) ;
#2897 = ADVANCED_FACE ( 'NONE', ( #26440 ), #17257, .T. ) ;
#2898 = VERTEX_POINT ( 'NONE', #19392 ) ;
#2899 = LINE ( 'NONE', #14758, #1605 ) ;
#2900 = EDGE_CURVE ( 'NONE', #17052, #16411, #21840, .T. ) ;
#2901 = CARTESIAN_POINT ( 'NONE',  ( 134.5152310637605808, -4.999999999999980460, -28.60870317832789311 ) ) ;
#2902 = AXIS2_PLACEMENT_3D ( 'NONE', #11022, #11461, #9017 ) ;
#2903 = DIRECTION ( 'NONE',  ( -0.9510565162951536422, -2.566386769018988323E-16, 0.3090169943749475623 ) ) ;
#2904 = CARTESIAN_POINT ( 'NONE',  ( -2.000000000000008882, 3.464101615137750390, 0.000000000000000000 ) ) ;
#2905 = CARTESIAN_POINT ( 'NONE',  ( 134.5152310637605524, -4.999999999999981348, -1.493419066897600538E-14 ) ) ;
#2906 = MECHANICAL_DESIGN_GEOMETRIC_PRESENTATION_REPRESENTATION (  '', ( #23841 ), #2411 ) ;
#2907 = CARTESIAN_POINT ( 'NONE',  ( 12.00785540763395254, 9.408655069060824161, -16.69968271487400813 ) ) ;
#2908 = DIRECTION ( 'NONE',  ( 0.5877852522924731371, 1.586114251531760728E-16, -0.8090169943749474513 ) ) ;
#2909 = CARTESIAN_POINT ( 'NONE',  ( 32.12153525177792091, -10.97127362787143312, -16.88978156643115724 ) ) ;
#2910 = VERTEX_POINT ( 'NONE', #10232 ) ;
#2911 = CARTESIAN_POINT ( 'NONE',  ( 8.944667066222118379, 16.95121494262130213, -17.88907156968992496 ) ) ;
#2912 = DIRECTION ( 'NONE',  ( -1.000000000000000000, 0.000000000000000000, 0.000000000000000000 ) ) ;
#2913 = CARTESIAN_POINT ( 'NONE',  ( 19.40121574091639189, 1.432572567346982240, -13.43353846741550406 ) ) ;
#2914 = CARTESIAN_POINT ( 'NONE',  ( 12.86106464449595777, 9.514195438118767001, -16.12106201145810047 ) ) ;
#2915 = FACE_BOUND ( 'NONE', #5984, .T. ) ;
#2916 = ORIENTED_EDGE ( 'NONE', *, *, #8493, .F. ) ;
#2917 = CARTESIAN_POINT ( 'NONE',  ( 10.43540724046455992, 14.02724713458965233, -16.28994223329847202 ) ) ;
#2918 = DIRECTION ( 'NONE',  ( 1.000000000000000000, 4.440892098500622217E-16, 0.000000000000000000 ) ) ;
#2919 = CARTESIAN_POINT ( 'NONE',  ( 9.916637298967875935, 16.40639221407973380, -16.50447193873893781 ) ) ;
#2920 = LINE ( 'NONE', #18777, #14976 ) ;
#2921 = VERTEX_POINT ( 'NONE', #19243 ) ;
#2922 = DIRECTION ( 'NONE',  ( -1.110223024625156540E-16, 0.000000000000000000, -1.000000000000000000 ) ) ;
#2923 = ORIENTED_EDGE ( 'NONE', *, *, #6603, .F. ) ;
#2924 = CARTESIAN_POINT ( 'NONE',  ( 12.02609123740286101, 9.325023229212996867, -16.69214155778140096 ) ) ;
#2925 = EDGE_CURVE ( 'NONE', #11270, #756, #24289, .T. ) ;
#2926 = VERTEX_POINT ( 'NONE', #3099 ) ;
#2927 = VECTOR ( 'NONE', #11292, 1000.000000000000000 ) ;
#2928 = CARTESIAN_POINT ( 'NONE',  ( 32.54894808986480115, -9.611255921941241454, -17.86757894403779900 ) ) ;
#2929 = CARTESIAN_POINT ( 'NONE',  ( 31.22280883588763700, -10.09333740185288875, -13.86128061636125786 ) ) ;
#2930 = CARTESIAN_POINT ( 'NONE',  ( 29.90031526554274777, -7.862644070287768905, -16.42500436498598049 ) ) ;
#2931 = ORIENTED_EDGE ( 'NONE', *, *, #17744, .F. ) ;
#2932 = CARTESIAN_POINT ( 'NONE',  ( 133.6922820468854241, -10.00000000000000711, -23.73366926340167282 ) ) ;
#2933 = LINE ( 'NONE', #28591, #25948 ) ;
#2934 = PRODUCT_CONTEXT ( 'NONE', #26477, 'mechanical' ) ;
#2935 = CARTESIAN_POINT ( 'NONE',  ( 18.57704598647189798, -1.039939211366111005, -17.60664924018008293 ) ) ;
#2936 = CARTESIAN_POINT ( 'NONE',  ( 27.10702390817755614, -8.414881854042032927, -18.30456363717458146 ) ) ;
#2937 = ADVANCED_FACE ( 'NONE', ( #3384 ), #12578, .T. ) ;
#2938 = EDGE_CURVE ( 'NONE', #8559, #25751, #14657, .T. ) ;
#2939 = ORIENTED_EDGE ( 'NONE', *, *, #23417, .F. ) ;
#2940 = ADVANCED_FACE ( 'NONE', ( #17112 ), #12676, .T. ) ;
#2941 = LINE ( 'NONE', #14503, #22725 ) ;
#2942 = EDGE_CURVE ( 'NONE', #7113, #24158, #19840, .T. ) ;
#2943 = FACE_BOUND ( 'NONE', #14033, .T. ) ;
#2944 = AXIS2_PLACEMENT_3D ( 'NONE', #1006, #17307, #17456 ) ;
#2945 = VERTEX_POINT ( 'NONE', #15716 ) ;
#2946 = PRODUCT_DEFINITION_FORMATION_WITH_SPECIFIED_SOURCE ( 'ANY', '', #14920, .NOT_KNOWN. ) ;
#2947 = PLANE ( 'NONE',  #20859 ) ;
#2948 = DIRECTION ( 'NONE',  ( 1.110223024625156540E-16, 2.995891024602366092E-32, 1.000000000000000000 ) ) ;
#2949 = VECTOR ( 'NONE', #9870, 1000.000000000000000 ) ;
#2950 = CARTESIAN_POINT ( 'NONE',  ( 153.6922820468853388, -4.999999999999975131, 2.247092850131519715 ) ) ;
#2951 = DIRECTION ( 'NONE',  ( -0.5877852522924731371, -1.586114251531760235E-16, 0.8090169943749474513 ) ) ;
#2952 = AXIS2_PLACEMENT_3D ( 'NONE', #6492, #20660, #25551 ) ;
#2953 = CARTESIAN_POINT ( 'NONE',  ( 12.24830724310059082, 9.517209185634078139, -15.33080109912759070 ) ) ;
#2954 = CARTESIAN_POINT ( 'NONE',  ( 25.07260858567070372, -5.000000000000010658, -77.16555467815769020 ) ) ;
#2955 = CARTESIAN_POINT ( 'NONE',  ( 143.6922820468854241, -1.999999999999978462, -6.413161187712876909 ) ) ;
#2956 = ORIENTED_EDGE ( 'NONE', *, *, #11250, .F. ) ;
#2957 = CARTESIAN_POINT ( 'NONE',  ( 11.48043977940431226, 9.236673419044803879, -15.85762597608872326 ) ) ;
#2958 = ORIENTED_EDGE ( 'NONE', *, *, #29135, .F. ) ;
#2959 = CARTESIAN_POINT ( 'NONE',  ( 23.26502027940742678, 3.673231887600847845, -16.77589761210995789 ) ) ;
#2960 = CYLINDRICAL_SURFACE ( 'NONE', #12674, 49.99999999999998579 ) ;
#2961 = DIRECTION ( 'NONE',  ( 0.5877852522924731371, 1.586114251531760728E-16, -0.8090169943749474513 ) ) ;
#2962 = EDGE_LOOP ( 'NONE', ( #16694, #21576, #18341, #27834, #8161, #7484, #19166, #22520, #25922, #589 ) ) ;
#2963 = PLANE ( 'NONE',  #22438 ) ;
#2964 = ORIENTED_EDGE ( 'NONE', *, *, #15363, .T. ) ;
#2965 = PLANE ( 'NONE',  #24708 ) ;
#2966 = CARTESIAN_POINT ( 'NONE',  ( 11.05552354607739929, 17.68892703645376585, -17.88069451076903249 ) ) ;
#2967 = VECTOR ( 'NONE', #3993, 1000.000000000000000 ) ;
#2968 = VERTEX_POINT ( 'NONE', #29839 ) ;
#2970 = CIRCLE ( 'NONE', #10229, 3.150000000000000799 ) ;
#2969 = CARTESIAN_POINT ( 'NONE',  ( 35.54859390953724585, -21.18451583373416014, -17.64281456791166391 ) ) ;
#2971 = CARTESIAN_POINT ( 'NONE',  ( 15.54217852991911997, 3.796156774867226247, -18.16774540469225485 ) ) ;
#2972 = PLANE ( 'NONE',  #16930 ) ;
#2973 = CARTESIAN_POINT ( 'NONE',  ( 9.057417708256320310, 16.43412612588882027, -17.11704294810955318 ) ) ;
#2974 = CARTESIAN_POINT ( 'NONE',  ( 28.55206495951409096, -10.69471729813234795, -19.99811924356017911 ) ) ;
#2975 = VERTEX_POINT ( 'NONE', #22602 ) ;
#2976 = CARTESIAN_POINT ( 'NONE',  ( 133.7287565553229456, -9.999999999999982236, 3.500000000000003109 ) ) ;
#2977 = FILL_AREA_STYLE ('',( #14981 ) ) ;
#2978 = VECTOR ( 'NONE', #6080, 1000.000000000000000 ) ;
#2979 = CARTESIAN_POINT ( 'NONE',  ( 23.41849298471255381, -3.203224238779429633, -13.27670244232306018 ) ) ;
#2980 = CARTESIAN_POINT ( 'NONE',  ( 16.99436549934495133, 9.190724047982882894, -15.08166918603070528 ) ) ;
#2981 = ORIENTED_EDGE ( 'NONE', *, *, #5896, .F. ) ;
#2982 = DIRECTION ( 'NONE',  ( 0.000000000000000000, 0.000000000000000000, -1.000000000000000000 ) ) ;
#2984 = ORIENTED_EDGE ( 'NONE', *, *, #12627, .F. ) ;
#2983 = EDGE_CURVE ( 'NONE', #23709, #8851, #22290, .T. ) ;
#2985 = DIRECTION ( 'NONE',  ( 0.000000000000000000, 0.000000000000000000, -1.000000000000000000 ) ) ;
#2986 = DIRECTION ( 'NONE',  ( -2.698458740408365879E-16, 1.000000000000000000, 0.000000000000000000 ) ) ;
#2987 = AXIS2_PLACEMENT_3D ( 'NONE', #17203, #10327, #10020 ) ;
#2988 = CARTESIAN_POINT ( 'NONE',  ( 13.00000000000000178, -2.870178842070716726E-15, 23.00000000000000000 ) ) ;
#2989 = DIRECTION ( 'NONE',  ( -2.698458740408365879E-16, 1.000000000000000000, 0.000000000000000000 ) ) ;
#2990 = VECTOR ( 'NONE', #5459, 1000.000000000000000 ) ;
#2991 = DIRECTION ( 'NONE',  ( 1.110223024625156540E-16, 2.995891024602366092E-32, 1.000000000000000000 ) ) ;
#2992 = CARTESIAN_POINT ( 'NONE',  ( 11.47652547240386944, 9.253065934422213701, -15.85936358228339316 ) ) ;
#2993 = CARTESIAN_POINT ( 'NONE',  ( 26.84622329165386745, -11.42663724297536554, -16.80226328336580366 ) ) ;
#2994 = CARTESIAN_POINT ( 'NONE',  ( 21.12965431673027794, -4.223434333162931154, -14.75790768142083031 ) ) ;
#2996 = EDGE_LOOP ( 'NONE', ( #24377, #11855, #13712, #737 ) ) ;
#2995 = CARTESIAN_POINT ( 'NONE',  ( 32.62126879184269512, -11.04717877266006987, -18.30218954475424908 ) ) ;
#2997 = DIRECTION ( 'NONE',  ( -0.000000000000000000, -0.000000000000000000, -1.000000000000000000 ) ) ;
#2998 = DIRECTION ( 'NONE',  ( -1.110223024625156540E-16, 0.000000000000000000, -1.000000000000000000 ) ) ;
#2999 = CARTESIAN_POINT ( 'NONE',  ( 12.50736435846123484, 8.573956625762026107, -15.12430548898761806 ) ) ;
#3000 = DIRECTION ( 'NONE',  ( -1.000000000000000000, 0.000000000000000000, 0.000000000000000000 ) ) ;
#3001 = CARTESIAN_POINT ( 'NONE',  ( 138.6922820468854241, -1.999999999999979572, 2.247092850131519715 ) ) ;
#3002 = CARTESIAN_POINT ( 'NONE',  ( 21.04385110482095200, 5.766204710259658306, -15.30406332615466347 ) ) ;
#3003 = LINE ( 'NONE', #9526, #12458 ) ;
#3004 = CARTESIAN_POINT ( 'NONE',  ( 10.69507909363156628, 16.74911557172037391, -15.96836912279556309 ) ) ;
#3005 = EDGE_CURVE ( 'NONE', #981, #10296, #20850, .T. ) ;
#3006 = LINE ( 'NONE', #21142, #14428 ) ;
#3007 = PLANE ( 'NONE',  #13229 ) ;
#3008 = CARTESIAN_POINT ( 'NONE',  ( 17.96884874826282186, 1.586046385177752871, -19.67104016136476119 ) ) ;
#3009 = CARTESIAN_POINT ( 'NONE',  ( 17.34455430865552472, 11.59597468841007384, -15.61519298676701695 ) ) ;
#3010 = VERTEX_POINT ( 'NONE', #2605 ) ;
#3012 = AXIS2_PLACEMENT_3D ( 'NONE', #1943, #6054, #11227 ) ;
#3011 = CARTESIAN_POINT ( 'NONE',  ( 34.93238815599637803, -19.41622979634004764, -20.17168434421570922 ) ) ;
#3013 = CARTESIAN_POINT ( 'NONE',  ( 21.98307778806466928, -1.383504679822651795, -14.66368364926259460 ) ) ;
#3014 = AXIS2_PLACEMENT_3D ( 'NONE', #15472, #3892, #22962 ) ;
#3015 = CARTESIAN_POINT ( 'NONE',  ( 18.61935276534875783, -1.259532457306228315, -15.72749031817820331 ) ) ;
#3016 = CARTESIAN_POINT ( 'NONE',  ( 27.79808892257030806, -9.771933472778439267, -13.29678235002263165 ) ) ;
#3017 = EDGE_LOOP ( 'NONE', ( #10896, #20345, #23474, #22065, #2703 ) ) ;
#3018 = ORIENTED_EDGE ( 'NONE', *, *, #2895, .T. ) ;
#3019 = LINE ( 'NONE', #12597, #23079 ) ;
#3020 = VERTEX_POINT ( 'NONE', #11291 ) ;
#3022 = ORIENTED_EDGE ( 'NONE', *, *, #11914, .F. ) ;
#3021 =( LENGTH_UNIT ( ) NAMED_UNIT ( * ) SI_UNIT ( .MILLI., .METRE. ) );
#3023 = LINE ( 'NONE', #10310, #13362 ) ;
#3024 = CARTESIAN_POINT ( 'NONE',  ( 427.0000000000002274, 34.64101615137744972, 14.00000000000000178 ) ) ;
#3025 = CARTESIAN_POINT ( 'NONE',  ( 36.12281451779777797, -20.27171456826661355, -20.44288436412734100 ) ) ;
#3026 = CARTESIAN_POINT ( 'NONE',  ( 9.641350810849047548, 17.66889113945805789, -17.95086732675817132 ) ) ;
#3027 = DIRECTION ( 'NONE',  ( 0.000000000000000000, -1.000000000000000000, -0.000000000000000000 ) ) ;
#3028 = CARTESIAN_POINT ( 'NONE',  ( 133.7287565553229456, -9.999999999999980460, 8.500000000000007105 ) ) ;
#3029 = CARTESIAN_POINT ( 'NONE',  ( 12.90142504057275197, 8.513187104919181181, -16.08590544042818493 ) ) ;
#3030 = CARTESIAN_POINT ( 'NONE',  ( 132.0152310637605524, -10.00000000000000711, -26.04193191628310800 ) ) ;
#3031 = CARTESIAN_POINT ( 'NONE',  ( 0.8120000000000002771, 0.000000000000000000, 0.000000000000000000 ) ) ;
#3032 = EDGE_CURVE ( 'NONE', #18212, #9897, #11880, .T. ) ;
#3033 = EDGE_CURVE ( 'NONE', #23017, #18285, #27660, .T. ) ;
#3034 = ORIENTED_EDGE ( 'NONE', *, *, #5777, .T. ) ;
#3035 = CARTESIAN_POINT ( 'NONE',  ( 142.2287565553230309, -4.999999999999978684, -29.49038105676659427 ) ) ;
#3036 = EDGE_CURVE ( 'NONE', #475, #10764, #14012, .T. ) ;
#3037 = VECTOR ( 'NONE', #25520, 1000.000000000000000 ) ;
#3038 = FACE_OUTER_BOUND ( 'NONE', #4714, .T. ) ;
#3039 = ORIENTED_EDGE ( 'NONE', *, *, #13566, .F. ) ;
#3040 = ADVANCED_FACE ( 'NONE', ( #7024, #21193 ), #4, .F. ) ;
#3041 = EDGE_LOOP ( 'NONE', ( #10760, #4891, #29811, #26534 ) ) ;
#3042 = B_SPLINE_CURVE_WITH_KNOTS ( 'NONE', 3,
 ( #382, #26026, #23731, #2829 ),
 .UNSPECIFIED., .F., .F.,
 ( 4, 4 ),
 ( 2.380737581676944055E-07, 0.002336974151641584615 ),
 .UNSPECIFIED. ) ;
#3043 = CARTESIAN_POINT ( 'NONE',  ( 11.23377902493292879, 9.047655202846097922, -17.23738383348171865 ) ) ;
#3044 = CARTESIAN_POINT ( 'NONE',  ( 24.46642504186807088, -8.279991823955473507, -18.31266784446766493 ) ) ;
#3045 = CARTESIAN_POINT ( 'NONE',  ( 20.86695504291294156, -3.984745147917406971, -17.88565525751875995 ) ) ;
#3046 = DIRECTION ( 'NONE',  ( 0.000000000000000000, 0.000000000000000000, 1.000000000000000000 ) ) ;
#3047 = DIRECTION ( 'NONE',  ( 1.000000000000000000, 0.000000000000000000, 0.000000000000000000 ) ) ;
#3048 = VECTOR ( 'NONE', #3377, 1000.000000000000000 ) ;
#3049 = DIRECTION ( 'NONE',  ( -2.698458740408365879E-16, 1.000000000000000000, 0.000000000000000000 ) ) ;
#3050 = DIRECTION ( 'NONE',  ( 0.000000000000000000, -1.000000000000000000, 0.000000000000000000 ) ) ;
#3051 = DIRECTION ( 'NONE',  ( -2.698458740408365879E-16, 1.000000000000000000, 0.000000000000000000 ) ) ;
#3052 = DIRECTION ( 'NONE',  ( 0.000000000000000000, 0.000000000000000000, 1.000000000000000000 ) ) ;
#3053 = AXIS2_PLACEMENT_3D ( 'NONE', #23053, #2005, #29522 ) ;
#3054 = FACE_OUTER_BOUND ( 'NONE', #22028, .T. ) ;
#3055 = LINE ( 'NONE', #21502, #22611 ) ;
#3056 = CARTESIAN_POINT ( 'NONE',  ( 10.51251736658329961, 16.26646593658467310, -17.31805759646961462 ) ) ;
#3057 = LINE ( 'NONE', #5177, #30207 ) ;
#3058 = CARTESIAN_POINT ( 'NONE',  ( 33.66044826391103584, -12.70207762650279015, -18.74488588032081893 ) ) ;
#3059 = ORIENTED_EDGE ( 'NONE', *, *, #23172, .F. ) ;
#3060 = CARTESIAN_POINT ( 'NONE',  ( 13.39626964006587428, 7.633314995549595139, -15.69459619883729928 ) ) ;
#3061 = LINE ( 'NONE', #2610, #21729 ) ;
#3062 = VECTOR ( 'NONE', #21797, 1000.000000000000000 ) ;
#3063 = CARTESIAN_POINT ( 'NONE',  ( 24.52797215547132836, -1.897736678990579184, -19.26084780660264073 ) ) ;
#3064 = CARTESIAN_POINT ( 'NONE',  ( 12.83519646890166577, 9.531778640408997916, -16.13946648208032641 ) ) ;
#3065 = CARTESIAN_POINT ( 'NONE',  ( 13.00000000000001243, 55.00000000000000711, -23.00000000000000000 ) ) ;
#3066 = ORIENTED_EDGE ( 'NONE', *, *, #3952, .F. ) ;
#3067 = VERTEX_POINT ( 'NONE', #2155 ) ;
#3068 = EDGE_CURVE ( 'NONE', #16190, #15401, #23344, .T. ) ;
#3069 = ORIENTED_EDGE ( 'NONE', *, *, #23686, .T. ) ;
#3070 = CARTESIAN_POINT ( 'NONE',  ( 11.47748818427356987, 9.248962635895034978, -15.85894168489154765 ) ) ;
#3071 = FACE_OUTER_BOUND ( 'NONE', #14781, .T. ) ;
#3072 = EDGE_CURVE ( 'NONE', #29919, #26117, #21869, .T. ) ;
#3073 = EDGE_CURVE ( 'NONE', #10747, #2878, #13101, .T. ) ;
#3074 = EDGE_CURVE ( 'NONE', #1424, #887, #5794, .T. ) ;
#3075 = CARTESIAN_POINT ( 'NONE',  ( 9.655099948573186097, 17.60583584124798051, -17.48406748397995614 ) ) ;
#3076 = DIRECTION ( 'NONE',  ( -1.110223024625156540E-16, 0.000000000000000000, -1.000000000000000000 ) ) ;
#3077 = EDGE_CURVE ( 'NONE', #9008, #21764, #23325, .T. ) ;
#3078 = ORIENTED_EDGE ( 'NONE', *, *, #28842, .F. ) ;
#3079 = EDGE_LOOP ( 'NONE', ( #2051, #17623, #29281, #13153, #6344, #2329, #5999, #6858, #17247, #29588 ) ) ;
#3080 = CARTESIAN_POINT ( 'NONE',  ( 174.5152310637604671, -1.999999999999969358, -19.94844914048349693 ) ) ;
#3081 = ORIENTED_EDGE ( 'NONE', *, *, #17585, .T. ) ;
#3082 = CARTESIAN_POINT ( 'NONE',  ( 11.50940939395034768, 11.69459202490242689, -16.90580767540677343 ) ) ;
#3083 = ORIENTED_EDGE ( 'NONE', *, *, #20735, .F. ) ;
#3084 = CARTESIAN_POINT ( 'NONE',  ( 36.51148101492068321, -23.01778725746827803, -19.37219236604238759 ) ) ;
#3085 = CARTESIAN_POINT ( 'NONE',  ( 27.20760296572909809, -8.488227175050779394, -13.35743234967312354 ) ) ;
#3086 = CARTESIAN_POINT ( 'NONE',  ( 16.19004574127830054, 9.516462436566445859, -20.03842800660303070 ) ) ;
#3087 = AXIS2_PLACEMENT_3D ( 'NONE', #22904, #13420, #25338 ) ;
#3088 = CARTESIAN_POINT ( 'NONE',  ( 157.0152310637604671, -4.999999999999975131, 1.702185954127501066 ) ) ;
#3089 = ORIENTED_EDGE ( 'NONE', *, *, #12760, .T. ) ;
#3090 = ORIENTED_EDGE ( 'NONE', *, *, #25828, .T. ) ;
#3091 = CARTESIAN_POINT ( 'NONE',  ( 33.07549275714919901, -10.34104163876563831, -17.35407900654646340 ) ) ;
#3092 = ITEM_DEFINED_TRANSFORMATION ( 'NONE', 'NONE', #16075,  #13190 ) ;
#3093 = CARTESIAN_POINT ( 'NONE',  ( 16.81761937449845234, 3.371063479271922514, -17.17107737352595720 ) ) ;
#3094 = CARTESIAN_POINT ( 'NONE',  ( 19.23836061553175369, 5.151828676608854352, -13.99136221198299168 ) ) ;
#3095 = VECTOR ( 'NONE', #1629, 1000.000000000000000 ) ;
#3096 = SURFACE_STYLE_FILL_AREA ( #12821 ) ;
#3097 = FACE_BOUND ( 'NONE', #21375, .T. ) ;
#3098 = CARTESIAN_POINT ( 'NONE',  ( 173.6922820468852819, -9.999999999999996447, -6.413161187712876909 ) ) ;
#3099 = CARTESIAN_POINT ( 'NONE',  ( 152.0152310637605240, -4.999999999999976907, -6.958068083716895558 ) ) ;
#3100 = DIRECTION ( 'NONE',  ( -2.698458740408365879E-16, 1.000000000000000000, 0.000000000000000000 ) ) ;
#3101 = CARTESIAN_POINT ( 'NONE',  ( 152.0152310637606092, -10.00000000000000000, -32.93883019725009120 ) ) ;
#3102 = CARTESIAN_POINT ( 'NONE',  ( 12.27682979692750997, 9.494989133591600350, -15.31072415319233215 ) ) ;
#3103 = CARTESIAN_POINT ( 'NONE',  ( 157.0152310637605240, -10.00000000000000000, -15.61832212156129707 ) ) ;
#3104 = DIRECTION ( 'NONE',  ( -0.8090169943749474513, -2.183098979609982436E-16, -0.5877852522924731371 ) ) ;
#3105 = ORIENTED_EDGE ( 'NONE', *, *, #10861, .T. ) ;
#3106 = CARTESIAN_POINT ( 'NONE',  ( 12.44984726620633353, 8.550925603015029353, -15.16996558791898231 ) ) ;
#3107 = ADVANCED_FACE ( 'NONE', ( #16314 ), #2306, .T. ) ;
#3108 = EDGE_CURVE ( 'NONE', #20929, #24158, #5023, .T. ) ;
#3109 = VECTOR ( 'NONE', #30197, 1000.000000000000000 ) ;
#3110 = CARTESIAN_POINT ( 'NONE',  ( 16.85369750842388825, 4.841181898090542113, -18.70119709635011418 ) ) ;
#3111 = FACE_OUTER_BOUND ( 'NONE', #29817, .T. ) ;
#3112 = DIRECTION ( 'NONE',  ( -0.8090169943749474513, -2.183098979609982436E-16, 0.5877852522924731371 ) ) ;
#3113 = EDGE_CURVE ( 'NONE', #28338, #23116, #14619, .T. ) ;
#3114 = CARTESIAN_POINT ( 'NONE',  ( 153.6922820468853388, -1.999999999999976241, -17.92658477444275533 ) ) ;
#3115 = EDGE_LOOP ( 'NONE', ( #14230, #7190, #14496, #28854 ) ) ;
#3116 = CARTESIAN_POINT ( 'NONE',  ( 156.1922820468853672, -1.999999999999974909, -13.59645775552055902 ) ) ;
#3117 = EDGE_CURVE ( 'NONE', #570, #12491, #17523, .T. ) ;
#3118 = CARTESIAN_POINT ( 'NONE',  ( 12.83225144795546235, 9.540626470039393681, -16.14103964284477399 ) ) ;
#3119 = VERTEX_POINT ( 'NONE', #7615 ) ;
#3120 = CARTESIAN_POINT ( 'NONE',  ( 33.61336211056222112, -12.49217533051321993, -18.72970452740151970 ) ) ;
#3121 = CARTESIAN_POINT ( 'NONE',  ( 17.88091890332929523, 4.544920326333207861, -13.91018511019278669 ) ) ;
#3122 = CARTESIAN_POINT ( 'NONE',  ( 416.0000000000002274, 34.64101615137744972, 14.00000000000000178 ) ) ;
#3123 = CARTESIAN_POINT ( 'NONE',  ( 16.22940209442605308, 10.22534693890197133, -14.12725775589269084 ) ) ;
#3124 = ORIENTED_EDGE ( 'NONE', *, *, #23242, .T. ) ;
#3125 = CARTESIAN_POINT ( 'NONE',  ( 133.6922820468854241, -1.999999999999980904, 2.247092850131519715 ) ) ;
#3126 = CARTESIAN_POINT ( 'NONE',  ( 21.59786356094703308, -0.7637721020719707710, -13.97513905925265298 ) ) ;
#3127 = CARTESIAN_POINT ( 'NONE',  ( 16.47391574482200483, 4.481796633190492152, -18.19319569287263150 ) ) ;
#3128 = ORIENTED_EDGE ( 'NONE', *, *, #27009, .T. ) ;
#3129 = CARTESIAN_POINT ( 'NONE',  ( 172.0152310637604103, -9.999999999999996447, 1.702185954127501066 ) ) ;
#3130 = ORIENTED_EDGE ( 'NONE', *, *, #8422, .F. ) ;
#3131 = VERTEX_POINT ( 'NONE', #3611 ) ;
#3132 = LINE ( 'NONE', #14085, #24889 ) ;
#3133 = VECTOR ( 'NONE', #15221, 1000.000000000000000 ) ;
#3134 = DIRECTION ( 'NONE',  ( -2.698458740408365879E-16, 1.000000000000000000, 0.000000000000000000 ) ) ;
#3135 = EDGE_CURVE ( 'NONE', #25090, #26900, #16774, .T. ) ;
#3136 = DIRECTION ( 'NONE',  ( -2.698458740408365879E-16, 1.000000000000000000, 0.000000000000000000 ) ) ;
#3137 = CARTESIAN_POINT ( 'NONE',  ( 131.1922820468854241, -10.00000000000000888, -4.936203717676158398 ) ) ;
#3138 = CARTESIAN_POINT ( 'NONE',  ( 86.87998469340118390, -4.999999999999993783, 63.12200371221075557 ) ) ;
#3139 = CARTESIAN_POINT ( 'NONE',  ( 10.43540724046455992, 14.02724713458965233, -16.28994223329847202 ) ) ;
#3140 = CARTESIAN_POINT ( 'NONE',  ( 29.29807706749550889, -8.594015191909356588, -15.50881839395299444 ) ) ;
#3141 = CARTESIAN_POINT ( 'NONE',  ( 30.68845550234816244, -8.154108532121835395, -15.50657635367809917 ) ) ;
#3143 = ORIENTED_EDGE ( 'NONE', *, *, #24560, .F. ) ;
#3142 = CARTESIAN_POINT ( 'NONE',  ( 33.37634376253905089, -12.42895282922877342, -19.69946502924221932 ) ) ;
#3144 = LINE ( 'NONE', #690, #11009 ) ;
#3145 = LINE ( 'NONE', #10281, #4824 ) ;
#3146 = CARTESIAN_POINT ( 'NONE',  ( 420.0000000000002274, 34.64101615137744972, 12.00000000000000178 ) ) ;
#3147 = LINE ( 'NONE', #17454, #12744 ) ;
#3148 = EDGE_CURVE ( 'NONE', #7135, #10866, #3057, .T. ) ;
#3149 = DIRECTION ( 'NONE',  ( -0.5877852522924731371, 0.000000000000000000, 0.8090169943749474513 ) ) ;
#3150 = PLANE ( 'NONE',  #13903 ) ;
#3151 = EDGE_CURVE ( 'NONE', #24767, #29985, #9743, .T. ) ;
#3152 = CARTESIAN_POINT ( 'NONE',  ( 22.39939798857497877, 2.694615832958070722, -14.02792042734668065 ) ) ;
#3153 = DIRECTION ( 'NONE',  ( -0.5877852522924731371, 0.000000000000000000, 0.8090169943749474513 ) ) ;
#3154 = ADVANCED_FACE ( 'NONE', ( #14469 ), #608, .T. ) ;
#3155 = CARTESIAN_POINT ( 'NONE',  ( 12.26306961015461461, 9.515005556349402482, -15.31970085818224980 ) ) ;
#3156 = CARTESIAN_POINT ( 'NONE',  ( 139.7287565553230309, -10.00000000000000533, -33.82050807568879947 ) ) ;
#3157 = FACE_OUTER_BOUND ( 'NONE', #9557, .T. ) ;
#3158 = CARTESIAN_POINT ( 'NONE',  ( 21.63873165585565417, 2.424707942738766331, -13.54651715722292060 ) ) ;
#3159 = AXIS2_PLACEMENT_3D ( 'NONE', #4835, #14133, #23462 ) ;
#3160 = CARTESIAN_POINT ( 'NONE',  ( 21.48460829514769799, 2.948577479130256584, -19.81588663513211657 ) ) ;
#3161 = ORIENTED_EDGE ( 'NONE', *, *, #23629, .T. ) ;
#3162 = CARTESIAN_POINT ( 'NONE',  ( 33.40713826534622655, -12.56408340279653757, -19.71064172033093698 ) ) ;
#3163 =( LENGTH_UNIT ( ) NAMED_UNIT ( * ) SI_UNIT ( .MILLI., .METRE. ) );
#3164 = CARTESIAN_POINT ( 'NONE',  ( 25.66261690555348807, -4.931278859741150100, -13.05994810794548933 ) ) ;
#3165 = CARTESIAN_POINT ( 'NONE',  ( 16.89975486243277913, 3.514059009776604015, -17.86885937027150817 ) ) ;
#3166 = EDGE_LOOP ( 'NONE', ( #2099, #5032, #27069, #28833 ) ) ;
#3167 = ORIENTED_EDGE ( 'NONE', *, *, #2900, .F. ) ;
#3168 = DIRECTION ( 'NONE',  ( -0.5877852522924731371, -1.586114251531760235E-16, 0.8090169943749474513 ) ) ;
#3169 = ORIENTED_EDGE ( 'NONE', *, *, #24776, .T. ) ;
#3170 = ORIENTED_EDGE ( 'NONE', *, *, #28913, .F. ) ;
#3171 = EDGE_CURVE ( 'NONE', #1746, #20723, #21351, .T. ) ;
#3172 = DIRECTION ( 'NONE',  ( -1.000000000000000000, 0.000000000000000000, 0.000000000000000000 ) ) ;
#3173 = LINE ( 'NONE', #12442, #22318 ) ;
#3174 = FACE_OUTER_BOUND ( 'NONE', #2526, .T. ) ;
#3175 = CIRCLE ( 'NONE', #8990, 4.756499999999999950 ) ;
#3176 = CARTESIAN_POINT ( 'NONE',  ( 18.00441060066494003, 9.543425513107552050, -19.87907960298149490 ) ) ;
#3177 = CARTESIAN_POINT ( 'NONE',  ( 35.48977118337261771, -17.42778619908077076, -20.26990708652652629 ) ) ;
#3178 = CARTESIAN_POINT ( 'NONE',  ( 10.82443827553465177, 12.24310121783546634, -16.12906421532448675 ) ) ;
#3179 = PLANE ( 'NONE',  #9788 ) ;
#3180 = CARTESIAN_POINT ( 'NONE',  ( 152.0152310637604955, -1.999999999999976241, -15.61832212156129351 ) ) ;
#3181 = CARTESIAN_POINT ( 'NONE',  ( 12.03842576178837298, 9.272001309349649389, -16.68677036593512497 ) ) ;
#3182 = LINE ( 'NONE', #26525, #9732 ) ;
#3183 = DIRECTION ( 'NONE',  ( 0.3090169943749475623, 8.338696094058001131E-17, 0.9510565162951536422 ) ) ;
#3184 = ORIENTED_EDGE ( 'NONE', *, *, #2942, .T. ) ;
#3185 = CARTESIAN_POINT ( 'NONE',  ( 168.6922820468852819, -1.999999999999971800, 2.247092850131519715 ) ) ;
#3186 = PLANE ( 'NONE',  #26876 ) ;
#3187 = CARTESIAN_POINT ( 'NONE',  ( 129.5152310637605524, -10.00000000000000888, -4.391296821672111328 ) ) ;
#3188 = ORIENTED_EDGE ( 'NONE', *, *, #7623, .F. ) ;
#3189 = ORIENTED_EDGE ( 'NONE', *, *, #14200, .F. ) ;
#3190 = CARTESIAN_POINT ( 'NONE',  ( 11.22446318822032296, 9.088639264749929225, -17.24136893309019669 ) ) ;
#3191 = ORIENTED_EDGE ( 'NONE', *, *, #2786, .T. ) ;
#3192 = CARTESIAN_POINT ( 'NONE',  ( 24.94601217299843654, -12.81575267032737742, -15.97323768315044035 ) ) ;
#3193 = CARTESIAN_POINT ( 'NONE',  ( 26.55721583451634160, -2.971036115494387175, -18.36415422809029607 ) ) ;
#3194 = LINE ( 'NONE', #12318, #12114 ) ;
#3195 = CARTESIAN_POINT ( 'NONE',  ( 9.407815906149622265, -5.000000000000015099, 28.95428013513216925 ) ) ;
#3196 = CIRCLE ( 'NONE', #27587, 3.000000000000002665 ) ;
#3197 = DIRECTION ( 'NONE',  ( 0.5877852522924731371, 0.000000000000000000, 0.8090169943749474513 ) ) ;
#3198 = FACE_OUTER_BOUND ( 'NONE', #21569, .T. ) ;
#3199 = ADVANCED_FACE ( 'NONE', ( #12903 ), #12332, .T. ) ;
#3200 = LINE ( 'NONE', #12632, #19158 ) ;
#3201 = LINE ( 'NONE', #2120, #21910 ) ;
#3202 = EDGE_CURVE ( 'NONE', #6766, #7950, #10617, .T. ) ;
#3203 = DIRECTION ( 'NONE',  ( 0.3090169943749472292, 8.338696094057992503E-17, -0.9510565162951536422 ) ) ;
#3204 = CARTESIAN_POINT ( 'NONE',  ( 137.0152310637605808, -4.999999999999980460, -26.04193191628310800 ) ) ;
#3205 = CARTESIAN_POINT ( 'NONE',  ( 11.96327893486549776, 9.613088455355432771, -16.71811665443363992 ) ) ;
#3206 = CARTESIAN_POINT ( 'NONE',  ( 35.54859390953724585, -22.18451583373416014, -17.22552805718784441 ) ) ;
#3207 = VERTEX_POINT ( 'NONE', #7471 ) ;
#3208 = CARTESIAN_POINT ( 'NONE',  ( 9.436770671236972774, 14.69436508140356246, -16.92063988783295159 ) ) ;
#3209 =( GEOMETRIC_REPRESENTATION_CONTEXT ( 3 ) GLOBAL_UNCERTAINTY_ASSIGNED_CONTEXT ( ( #25987 ) ) GLOBAL_UNIT_ASSIGNED_CONTEXT ( ( #18544, #16247, #22987 ) ) REPRESENTATION_CONTEXT ( 'NONE', 'WORKASPACE' ) );
#3210 = CARTESIAN_POINT ( 'NONE',  ( 23.77086030874127687, -7.150112426529108944, -14.59934731766091431 ) ) ;
#3211 = CARTESIAN_POINT ( 'NONE',  ( 12.83227036137552446, 9.540540802112166929, -16.14103173976383587 ) ) ;
#3212 = FACE_BOUND ( 'NONE', #24, .T. ) ;
#3213 = VERTEX_POINT ( 'NONE', #28561 ) ;
#3214 = CARTESIAN_POINT ( 'NONE',  ( 11.51951884677450266, 9.108496074915260365, -15.83757232928968683 ) ) ;
#3215 = LINE ( 'NONE', #14484, #16494 ) ;
#3216 = CARTESIAN_POINT ( 'NONE',  ( 11.47269659055779378, 9.270105954394804115, -15.86098659800193644 ) ) ;
#3217 = PLANE ( 'NONE',  #13049 ) ;
#3218 = VERTEX_POINT ( 'NONE', #28417 ) ;
#3219 = CARTESIAN_POINT ( 'NONE',  ( 133.7287565553229172, -1.999999999999980904, -33.50000000000000000 ) ) ;
#3220 = ORIENTED_EDGE ( 'NONE', *, *, #22422, .T. ) ;
#3221 = CARTESIAN_POINT ( 'NONE',  ( 11.70392491148546732, 10.80251906652491556, -16.82536866641744311 ) ) ;
#3222 = CIRCLE ( 'NONE', #5140, 13.00000000000000178 ) ;
#3223 = ORIENTED_EDGE ( 'NONE', *, *, #26222, .T. ) ;
#3224 = CARTESIAN_POINT ( 'NONE',  ( 36.54859390953724585, -23.18451583373416014, -16.94733705004010105 ) ) ;
#3225 = CARTESIAN_POINT ( 'NONE',  ( 25.90632082398269276, -12.28056132945115841, -15.12647891527467969 ) ) ;
#3226 = CARTESIAN_POINT ( 'NONE',  ( 14.03447742461322534, 10.03307406631979326, -15.27079475659193086 ) ) ;
#3227 = VECTOR ( 'NONE', #11407, 1000.000000000000000 ) ;
#3228 = DIRECTION ( 'NONE',  ( -0.9510565162951536422, -2.566386769018988323E-16, 0.3090169943749475623 ) ) ;
#3229 = EDGE_LOOP ( 'NONE', ( #13560, #4298, #26514, #13626 ) ) ;
#3230 = ORIENTED_EDGE ( 'NONE', *, *, #20276, .F. ) ;
#3231 = CARTESIAN_POINT ( 'NONE',  ( 36.54859390953724585, -22.18451583373416014, -16.94733705004010460 ) ) ;
#3232 = PRODUCT_CONTEXT ( 'NONE', #11423, 'mechanical' ) ;
#3233 = CARTESIAN_POINT ( 'NONE',  ( 17.18133768520950255, 3.791981501156216350, -18.48732239789962506 ) ) ;
#3234 = CIRCLE ( 'NONE', #9538, 1.500000000000001332 ) ;
#3235 = CARTESIAN_POINT ( 'NONE',  ( 19.20291185354690811, 8.143073066566493878, -16.32372945079811188 ) ) ;
#3236 = COLOUR_RGB ( '', 0.09019608, 0.27058824, 0.51372549) ;
#3237 = ORIENTED_EDGE ( 'NONE', *, *, #29958, .F. ) ;
#3238 = CARTESIAN_POINT ( 'NONE',  ( 144.5152310637605808, -1.999999999999977129, -21.71180489736091346 ) ) ;
#3239 = FACE_BOUND ( 'NONE', #18051, .T. ) ;
#3240 = ADVANCED_FACE ( 'NONE', ( #5335 ), #16919, .T. ) ;
#3241 = EDGE_CURVE ( 'NONE', #18375, #23025, #19355, .T. ) ;
#3242 = ADVANCED_FACE ( 'NONE', ( #21504, #17633, #24672 ), #26248, .T. ) ;
#3243 = CYLINDRICAL_SURFACE ( 'NONE', #13074, 2.928571428571432378 ) ;
#3244 = CARTESIAN_POINT ( 'NONE',  ( 0.000000000000000000, 0.000000000000000000, 0.000000000000000000 ) ) ;
#3245 = FACE_OUTER_BOUND ( 'NONE', #24557, .T. ) ;
#3246 = ORIENTED_EDGE ( 'NONE', *, *, #1450, .T. ) ;
#3247 = FACE_OUTER_BOUND ( 'NONE', #25710, .T. ) ;
#3248 = VECTOR ( 'NONE', #27756, 1000.000000000000000 ) ;
#3249 = CARTESIAN_POINT ( 'NONE',  ( 12.27129069473257239, 9.507470051170034964, -15.31400031939534045 ) ) ;
#3250 = LINE ( 'NONE', #17409, #27020 ) ;
#3251 = ORIENTED_EDGE ( 'NONE', *, *, #7811, .F. ) ;
#3252 = DIRECTION ( 'NONE',  ( -2.698458740408365879E-16, 1.000000000000000000, 0.000000000000000000 ) ) ;
#3253 = ORIENTED_EDGE ( 'NONE', *, *, #7874, .T. ) ;
#3254 = VECTOR ( 'NONE', #27076, 1000.000000000000000 ) ;
#3255 = CARTESIAN_POINT ( 'NONE',  ( 11.69419402147360110, 8.800013620902292999, -15.72776802682527730 ) ) ;
#3256 = AXIS2_PLACEMENT_3D ( 'NONE', #29199, #19541, #942 ) ;
#3257 = CARTESIAN_POINT ( 'NONE',  ( 19.77054944300549622, 4.331964111641410042, -19.42026316723860901 ) ) ;
#3258 = DIRECTION ( 'NONE',  ( -2.698458740408365879E-16, 1.000000000000000000, 0.000000000000000000 ) ) ;
#3259 = LINE ( 'NONE', #16820, #11693 ) ;
#3260 = ORIENTED_EDGE ( 'NONE', *, *, #23380, .F. ) ;
#3261 = PLANE ( 'NONE',  #21758 ) ;
#3262 = ORIENTED_EDGE ( 'NONE', *, *, #685, .F. ) ;
#3263 = CARTESIAN_POINT ( 'NONE',  ( 12.85347977544317111, 9.515020184875311315, -16.12678873937763413 ) ) ;
#3264 = EDGE_LOOP ( 'NONE', ( #9545, #14785, #26529, #1094 ) ) ;
#3265 = CARTESIAN_POINT ( 'NONE',  ( 36.36958547251401797, -20.38032574959806098, -19.43068663056894252 ) ) ;
#3266 = CARTESIAN_POINT ( 'NONE',  ( 14.57776618122778700, 6.338444840345393239, -15.85465340776532095 ) ) ;
#3267 = ORIENTED_EDGE ( 'NONE', *, *, #9277, .T. ) ;
#3268 = DIRECTION ( 'NONE',  ( -1.000000000000000000, 0.000000000000000000, 0.000000000000000000 ) ) ;
#3269 = CARTESIAN_POINT ( 'NONE',  ( 15.02162844583664736, 5.759011576665847620, -14.59661587647459591 ) ) ;
#3270 = CARTESIAN_POINT ( 'NONE',  ( 8.000000000000001776, 4.336808689942017736E-15, -5.000000000000000888 ) ) ;
#3271 = LINE ( 'NONE', #29551, #29637 ) ;
#3272 = CARTESIAN_POINT ( 'NONE',  ( 26.55721583451634160, -2.971036115494387175, -18.36415422809029607 ) ) ;
#3273 = CARTESIAN_POINT ( 'NONE',  ( 20.29966856415212817, 4.923229158599749411, -18.85509502865480869 ) ) ;
#3274 = AXIS2_PLACEMENT_3D ( 'NONE', #13005, #17580, #15441 ) ;
#3275 = VERTEX_POINT ( 'NONE', #744 ) ;
#3276 = DIRECTION ( 'NONE',  ( -0.8090169943749474513, -2.183098979609982436E-16, -0.5877852522924731371 ) ) ;
#3277 = AXIS2_PLACEMENT_3D ( 'NONE', #22584, #29818, #6253 ) ;
#3278 = EDGE_CURVE ( 'NONE', #4517, #3213, #28268, .T. ) ;
#3279 = AXIS2_PLACEMENT_3D ( 'NONE', #8884, #9026, #6167 ) ;
#3280 = ADVANCED_FACE ( 'NONE', ( #7322 ), #16623, .T. ) ;
#3281 = EDGE_CURVE ( 'NONE', #25944, #7041, #29909, .T. ) ;
#3282 = CARTESIAN_POINT ( 'NONE',  ( 151.1922820468854241, -10.00000000000000178, -22.25671179336496053 ) ) ;
#3283 = EDGE_CURVE ( 'NONE', #17861, #5150, #11219, .T. ) ;
#3284 = CARTESIAN_POINT ( 'NONE',  ( 169.5152310637604671, -9.999999999999996447, -21.71180489736091346 ) ) ;
#3285 = CARTESIAN_POINT ( 'NONE',  ( -5.000000000000000000, 0.000000000000000000, -23.00000000000000000 ) ) ;
#3286 = CARTESIAN_POINT ( 'NONE',  ( 8.000000000000000000, 9.797174393178825657E-16, 4.999999999999997335 ) ) ;
#3287 = CARTESIAN_POINT ( 'NONE',  ( 11.82447321682112751, 8.672047275158794477, -15.63808403058127006 ) ) ;
#3288 = CARTESIAN_POINT ( 'NONE',  ( 25.57659404178318141, -9.842204813007603192, -16.83936284125123706 ) ) ;
#3289 = CARTESIAN_POINT ( 'NONE',  ( 24.97892660363778106, -6.291154998746494087, -12.74939059104742256 ) ) ;
#3291 = ORIENTED_EDGE ( 'NONE', *, *, #21767, .F. ) ;
#3290 = CARTESIAN_POINT ( 'NONE',  ( 32.89062095351589932, -11.25267498498577723, -18.96775996542842435 ) ) ;
#3292 = DIRECTION ( 'NONE',  ( 1.000000000000000000, 0.000000000000000000, 0.000000000000000000 ) ) ;
#3293 = DIRECTION ( 'NONE',  ( -2.698458740408365879E-16, 1.000000000000000000, 0.000000000000000000 ) ) ;
#3294 = CARTESIAN_POINT ( 'NONE',  ( 8.469702402841419307E-15, 60.00000000000000711, 12.49999999999999112 ) ) ;
#3295 = LINE ( 'NONE', #19892, #25365 ) ;
#3296 = CIRCLE ( 'NONE', #20319, 1.499999999999996225 ) ;
#3297 = DIRECTION ( 'NONE',  ( -2.698458740408365879E-16, 1.000000000000000000, 0.000000000000000000 ) ) ;
#3298 = PRESENTATION_STYLE_ASSIGNMENT (( #1298 ) ) ;
#3299 = CARTESIAN_POINT ( 'NONE',  ( 19.50856600871340873, -1.908691058934758100, -18.90332006808282728 ) ) ;
#3300 = ORIENTED_EDGE ( 'NONE', *, *, #28102, .T. ) ;
#3301 = LINE ( 'NONE', #10289, #19309 ) ;
#3302 = CARTESIAN_POINT ( 'NONE',  ( 11.62855932722735908, 12.46805622939721836, -15.57880556977976916 ) ) ;
#3303 = VECTOR ( 'NONE', #287, 1000.000000000000000 ) ;
#3304 = CARTESIAN_POINT ( 'NONE',  ( 33.10952763335142635, -11.62914684427059697, -19.38687730282833499 ) ) ;
#3305 = LINE ( 'NONE', #1158, #21016 ) ;
#3306 = VERTEX_POINT ( 'NONE', #30052 ) ;
#3307 = CARTESIAN_POINT ( 'NONE',  ( 25.21413058671614849, -1.115224416820481457, -18.44856734933592080 ) ) ;
#3308 = CARTESIAN_POINT ( 'NONE',  ( 17.05458169553830317, 2.837819561348359887, -13.69156784695313611 ) ) ;
#3309 = EDGE_LOOP ( 'NONE', ( #19974, #23855, #29841, #13234 ) ) ;
#3310 = CARTESIAN_POINT ( 'NONE',  ( 32.77977724007769211, -11.13765286058784554, -18.71157503069099448 ) ) ;
#3311 = CARTESIAN_POINT ( 'NONE',  ( 25.92665957894408280, -9.004797978260709712, -12.14503282074142909 ) ) ;
#3312 = CARTESIAN_POINT ( 'NONE',  ( 24.07185007603571592, -6.521566527568181115, -20.06683206624251525 ) ) ;
#3313 = CARTESIAN_POINT ( 'NONE',  ( 25.23810427664335165, -6.496417100615061280, -13.69959235629456629 ) ) ;
#3314 = EDGE_CURVE ( 'NONE', #4331, #14937, #11614, .T. ) ;
#3315 = AXIS2_PLACEMENT_3D ( 'NONE', #6044, #15034, #24220 ) ;
#3316 = ADVANCED_FACE ( 'NONE', ( #8769 ), #20222, .T. ) ;
#3317 = DIRECTION ( 'NONE',  ( -0.9510565162951536422, -2.566386769018988323E-16, 0.3090169943749475623 ) ) ;
#3318 = ADVANCED_FACE ( 'NONE', ( #24980 ), #27300, .T. ) ;
#3319 = EDGE_LOOP ( 'NONE', ( #2678, #3367, #5310, #25559, #28021 ) ) ;
#3320 = DIRECTION ( 'NONE',  ( 1.110223024625156540E-16, 2.995891024602366092E-32, 1.000000000000000000 ) ) ;
#3321 = VECTOR ( 'NONE', #21531, 1000.000000000000000 ) ;
#3322 = FACE_OUTER_BOUND ( 'NONE', #6386, .T. ) ;
#3323 = PLANE ( 'NONE',  #12883 ) ;
#3324 = CARTESIAN_POINT ( 'NONE',  ( 16.36264732604271899, 7.873549196589271659, -20.78255227469630739 ) ) ;
#3325 = CARTESIAN_POINT ( 'NONE',  ( 36.18478257229246964, -20.55010421171508028, -20.40673782175607442 ) ) ;
#3326 = CARTESIAN_POINT ( 'NONE',  ( 9.957223259857686415, 16.22025982393231303, -16.48768813039480818 ) ) ;
#3327 = LINE ( 'NONE', #3466, #5433 ) ;
#3328 = CARTESIAN_POINT ( 'NONE',  ( 147.0152310637605808, -1.999999999999976241, -34.70218595412750773 ) ) ;
#3329 = CARTESIAN_POINT ( 'NONE',  ( 12.02805304935487563, 9.316025821727821565, -16.69133030147860453 ) ) ;
#3330 = DIRECTION ( 'NONE',  ( 0.000000000000000000, 0.000000000000000000, 1.000000000000000000 ) ) ;
#3331 = FACE_OUTER_BOUND ( 'NONE', #20608, .T. ) ;
#3332 = ORIENTED_EDGE ( 'NONE', *, *, #17624, .F. ) ;
#3333 = CARTESIAN_POINT ( 'NONE',  ( 172.0152310637604103, -4.999999999999970690, -1.909752701132032663E-14 ) ) ;
#3334 = CARTESIAN_POINT ( 'NONE',  ( 172.0152310637604671, -1.999999999999970024, -15.61832212156129707 ) ) ;
#3335 = VECTOR ( 'NONE', #7361, 1000.000000000000000 ) ;
#3336 = LINE ( 'NONE', #19334, #25381 ) ;
#3337 = ORIENTED_EDGE ( 'NONE', *, *, #4358, .F. ) ;
#3338 = ORIENTED_EDGE ( 'NONE', *, *, #11651, .F. ) ;
#3339 = CARTESIAN_POINT ( 'NONE',  ( 11.22879857168519813, 9.069188343361037852, -17.23954317433854300 ) ) ;
#3340 = VECTOR ( 'NONE', #23794, 1000.000000000000000 ) ;
#3341 = CARTESIAN_POINT ( 'NONE',  ( 27.55585723563325473, -10.26521964199731407, -19.78748283923107820 ) ) ;
#3342 = CARTESIAN_POINT ( 'NONE',  ( 22.09907825138052218, -7.445301066569870230, -16.29136317631293807 ) ) ;
#3343 = LINE ( 'NONE', #14901, #11625 ) ;
#3344 = DIRECTION ( 'NONE',  ( 1.110223024625156540E-16, 2.995891024602366092E-32, 1.000000000000000000 ) ) ;
#3345 = DIRECTION ( 'NONE',  ( 0.000000000000000000, 0.000000000000000000, 1.000000000000000000 ) ) ;
#3346 = ORIENTED_EDGE ( 'NONE', *, *, #20329, .T. ) ;
#3347 = LINE ( 'NONE', #7463, #25488 ) ;
#3348 = EDGE_CURVE ( 'NONE', #16128, #5097, #12599, .T. ) ;
#3349 = LINE ( 'NONE', #10189, #11351 ) ;
#3350 = CARTESIAN_POINT ( 'NONE',  ( 6.938893903907228378E-15, 60.00000000000000711, -1.040834085586084257E-14 ) ) ;
#3351 = CARTESIAN_POINT ( 'NONE',  ( 162.0152310637604955, -1.999999999999972244, -26.04193191628311155 ) ) ;
#3352 = LINE ( 'NONE', #29018, #10902 ) ;
#3353 = CARTESIAN_POINT ( 'NONE',  ( 12.02932678857878734, 9.310239991255825132, -16.69079931733866218 ) ) ;
#3354 = CARTESIAN_POINT ( 'NONE',  ( 31.77493940018505114, -11.56844746753418640, -13.90849911728625266 ) ) ;
#3355 = AXIS2_PLACEMENT_3D ( 'NONE', #18834, #25871, #2830 ) ;
#3356 = ORIENTED_EDGE ( 'NONE', *, *, #16529, .T. ) ;
#3357 = CARTESIAN_POINT ( 'NONE',  ( 9.110807846758516959, 16.18927214505777812, -17.05547580459120383 ) ) ;
#3358 = CARTESIAN_POINT ( 'NONE',  ( 21.54098841764929873, -5.100688324319140321, -15.19385678519978633 ) ) ;
#3359 = CARTESIAN_POINT ( 'NONE',  ( 12.82210747586494293, 9.587147947373788170, -16.14523453761016825 ) ) ;
#3360 = FACE_BOUND ( 'NONE', #11696, .T. ) ;
#3361 = ORIENTED_EDGE ( 'NONE', *, *, #18637, .F. ) ;
#3362 = AXIS2_PLACEMENT_3D ( 'NONE', #27447, #17924, #15493 ) ;
#3363 = EDGE_LOOP ( 'NONE', ( #29885, #23813, #6486, #12961 ) ) ;
#3364 = DIRECTION ( 'NONE',  ( 0.9510565162951536422, 2.566386769018988816E-16, 0.3090169943749472292 ) ) ;
#3365 = CARTESIAN_POINT ( 'NONE',  ( 11.47338783222600789, 9.266948822715743717, -15.86069975447064806 ) ) ;
#3366 = CARTESIAN_POINT ( 'NONE',  ( 123.0533251596896918, -4.999999999999984901, -89.40347394098662903 ) ) ;
#3367 = ORIENTED_EDGE ( 'NONE', *, *, #23339, .T. ) ;
#3368 = DIRECTION ( 'NONE',  ( 0.9510565162951536422, 0.000000000000000000, -0.3090169943749475623 ) ) ;
#3369 = ORIENTED_EDGE ( 'NONE', *, *, #4832, .F. ) ;
#3370 = CARTESIAN_POINT ( 'NONE',  ( 12.02871927673971619, 9.312984558958580905, -16.69105371450780595 ) ) ;
#3371 = EDGE_CURVE ( 'NONE', #4554, #22145, #6648, .T. ) ;
#3372 = ORIENTED_EDGE ( 'NONE', *, *, #13657, .F. ) ;
#3373 = CARTESIAN_POINT ( 'NONE',  ( 20.04052888069229610, 8.940267654624740601, -17.40200224619232117 ) ) ;
#3374 = CARTESIAN_POINT ( 'NONE',  ( 16.83828815103352028, 11.11029360287396983, -16.41243972054167344 ) ) ;
#3375 = LINE ( 'NONE', #10519, #14983 ) ;
#3376 = ORIENTED_EDGE ( 'NONE', *, *, #6513, .T. ) ;
#3377 = DIRECTION ( 'NONE',  ( -2.698458740408365879E-16, 1.000000000000000000, 0.000000000000000000 ) ) ;
#3378 = CARTESIAN_POINT ( 'NONE',  ( 17.06466135374324011, 3.680263393506696179, -18.28590298471088005 ) ) ;
#3379 = AXIS2_PLACEMENT_3D ( 'NONE', #23689, #946, #24439 ) ;
#3380 = CARTESIAN_POINT ( 'NONE',  ( 15.14574614762244487, 6.587483969391940697, -15.14885142785537830 ) ) ;
#3381 = CIRCLE ( 'NONE', #20420, 2.749999999999999112 ) ;
#3382 = FACE_BOUND ( 'NONE', #29804, .T. ) ;
#3383 = DIRECTION ( 'NONE',  ( 1.000000000000000000, -0.000000000000000000, 0.000000000000000000 ) ) ;
#3384 = FACE_OUTER_BOUND ( 'NONE', #16591, .T. ) ;
#3385 = CARTESIAN_POINT ( 'NONE',  ( 12.89848499353137434, 9.804829592035655850, -14.81257543908856000 ) ) ;
#3386 = DIRECTION ( 'NONE',  ( 0.5877852522924731371, 1.586114251531760728E-16, 0.8090169943749474513 ) ) ;
#3387 = CARTESIAN_POINT ( 'NONE',  ( 12.27681432698556918, 9.495076167121005994, -15.31072932366845407 ) ) ;
#3388 = FACE_OUTER_BOUND ( 'NONE', #18207, .T. ) ;
#3389 = VECTOR ( 'NONE', #11402, 1000.000000000000000 ) ;
#3390 = LINE ( 'NONE', #7954, #6688 ) ;
#3391 = VERTEX_POINT ( 'NONE', #24824 ) ;
#3392 = CARTESIAN_POINT ( 'NONE',  ( 12.53458732174692258, 8.585986940276173485, -15.10260830673100330 ) ) ;
#3393 = EDGE_LOOP ( 'NONE', ( #430, #28432, #8760, #4768 ) ) ;
#3394 = CARTESIAN_POINT ( 'NONE',  ( 10.50660601767968139, 9.787963810330234438, -16.47822533839871539 ) ) ;
#3395 = FACE_OUTER_BOUND ( 'NONE', #18625, .T. ) ;
#3396 = LINE ( 'NONE', #511, #18039 ) ;
#3397 = AXIS2_PLACEMENT_3D ( 'NONE', #26209, #10457, #24515 ) ;
#3398 = VERTEX_POINT ( 'NONE', #4355 ) ;
#3399 = DIRECTION ( 'NONE',  ( 1.000000000000000000, 0.000000000000000000, 0.000000000000000000 ) ) ;
#3400 = ORIENTED_EDGE ( 'NONE', *, *, #16305, .T. ) ;
#3401 = CARTESIAN_POINT ( 'NONE',  ( 12.84461350077944886, 9.519659821018855439, -16.13320262440205966 ) ) ;
#3402 = EDGE_CURVE ( 'NONE', #27090, #11338, #13658, .T. ) ;
#3403 = EDGE_CURVE ( 'NONE', #24408, #24131, #22681, .T. ) ;
#3404 = CARTESIAN_POINT ( 'NONE',  ( 34.39665924806198660, -11.72086467124742981, -18.77862448471655199 ) ) ;
#3405 = CARTESIAN_POINT ( 'NONE',  ( 16.06572049258021195, 3.735912457719189117, -15.00855390560170477 ) ) ;
#3406 = EDGE_CURVE ( 'NONE', #16269, #29646, #4507, .T. ) ;
#3407 = CARTESIAN_POINT ( 'NONE',  ( 176.1922820468852535, -1.999999999999969580, -2.083034168790677043 ) ) ;
#3408 = EDGE_CURVE ( 'NONE', #570, #887, #15361, .T. ) ;
#3409 = CARTESIAN_POINT ( 'NONE',  ( 25.50411877999659893, -13.63830170496968996, -16.08255890605547123 ) ) ;
#3410 = ORIENTED_EDGE ( 'NONE', *, *, #21711, .T. ) ;
#3411 = DIRECTION ( 'NONE',  ( -2.698458740408365879E-16, 1.000000000000000000, 0.000000000000000000 ) ) ;
#3412 =( LENGTH_UNIT ( ) NAMED_UNIT ( * ) SI_UNIT ( .MILLI., .METRE. ) );
#3413 = CARTESIAN_POINT ( 'NONE',  ( 24.52508672555368463, -0.3756359333432500169, -18.08805785897195051 ) ) ;
#3414 = CARTESIAN_POINT ( 'NONE',  ( 19.73758642798775753, -1.564653675968832314, -13.27997001701493041 ) ) ;
#3415 = ORIENTED_EDGE ( 'NONE', *, *, #8987, .T. ) ;
#3416 =( GEOMETRIC_REPRESENTATION_CONTEXT ( 3 ) GLOBAL_UNCERTAINTY_ASSIGNED_CONTEXT ( ( #13762 ) ) GLOBAL_UNIT_ASSIGNED_CONTEXT ( ( #1729, #8569, #3709 ) ) REPRESENTATION_CONTEXT ( 'NONE', 'WORKASPACE' ) );
#3417 = EDGE_LOOP ( 'NONE', ( #25701, #28488, #21252, #25724 ) ) ;
#3418 = FACE_OUTER_BOUND ( 'NONE', #14283, .T. ) ;
#3419 = VECTOR ( 'NONE', #1824, 1000.000000000000000 ) ;
#3420 = CARTESIAN_POINT ( 'NONE',  ( 163.6922820468853104, -1.999999999999972689, -6.413161187712876909 ) ) ;
#3421 = CARTESIAN_POINT ( 'NONE',  ( -7.345652830558757174, 4.996589667937388235, -4.503584543331204060 ) ) ;
#3422 = DIRECTION ( 'NONE',  ( -2.698458740408365879E-16, 1.000000000000000000, 0.000000000000000000 ) ) ;
#3423 = CARTESIAN_POINT ( 'NONE',  ( 144.5152310637605524, -1.999999999999978018, -2.627941064794695691 ) ) ;
#3424 = ORIENTED_EDGE ( 'NONE', *, *, #7605, .T. ) ;
#3425 = CARTESIAN_POINT ( 'NONE',  ( 9.949118446627077006, 16.25742953053141804, -16.49103975576934644 ) ) ;
#3426 = CARTESIAN_POINT ( 'NONE',  ( 29.41685937463160272, -8.713933360145817986, -16.19581194183416883 ) ) ;
#3427 = CARTESIAN_POINT ( 'NONE',  ( 23.43951749033787735, -6.062008688038916127, -19.28752554440484701 ) ) ;
#3428 = AXIS2_PLACEMENT_3D ( 'NONE', #10745, #844, #28962 ) ;
#3429 = FACE_OUTER_BOUND ( 'NONE', #5444, .T. ) ;
#3430 = DIRECTION ( 'NONE',  ( 1.000000000000000000, 0.000000000000000000, 0.000000000000000000 ) ) ;
#3431 = CYLINDRICAL_SURFACE ( 'NONE', #6294, 1.500000000000001332 ) ;
#3432 = CIRCLE ( 'NONE', #2494, 0.4999999999999986677 ) ;
#3433 = LINE ( 'NONE', #19295, #15174 ) ;
#3434 = CARTESIAN_POINT ( 'NONE',  ( 142.2287565553230024, -1.999999999999978462, -3.509618943233403510 ) ) ;
#3435 = CARTESIAN_POINT ( 'NONE',  ( 0.000000000000000000, 0.000000000000000000, -5.000000000000000888 ) ) ;
#3436 = CARTESIAN_POINT ( 'NONE',  ( 19.40121574091639189, 1.432572567346982240, -13.43353846741550406 ) ) ;
#3437 = ORIENTED_EDGE ( 'NONE', *, *, #21134, .F. ) ;
#3438 = DIRECTION ( 'NONE',  ( 1.000000000000000000, 0.000000000000000000, 0.000000000000000000 ) ) ;
#3439 = CARTESIAN_POINT ( 'NONE',  ( 12.27691635572497830, 9.494607244959519576, -15.31068720787289728 ) ) ;
#3440 = EDGE_CURVE ( 'NONE', #8350, #23249, #13584, .T. ) ;
#3441 = AXIS2_PLACEMENT_3D ( 'NONE', #19559, #24155, #23864 ) ;
#3442 = CARTESIAN_POINT ( 'NONE',  ( 32.30218501430429967, -10.99871056796995816, -17.40035725849610060 ) ) ;
#3443 = DIRECTION ( 'NONE',  ( -6.938893903907227392E-16, 0.000000000000000000, -1.000000000000000000 ) ) ;
#3444 = EDGE_CURVE ( 'NONE', #17843, #2040, #6353, .T. ) ;
#3445 = AXIS2_PLACEMENT_3D ( 'NONE', #4645, #13936, #23267 ) ;
#3446 = CARTESIAN_POINT ( 'NONE',  ( 16.94076125623460527, 0.4124075662712927692, -16.40086227390004936 ) ) ;
#3447 = LINE ( 'NONE', #29273, #1850 ) ;
#3448 = ADVANCED_FACE ( 'NONE', ( #27137 ), #5061, .F. ) ;
#3449 = CARTESIAN_POINT ( 'NONE',  ( 19.77430725462212635, 0.2453161447429414443, -14.21425550582737074 ) ) ;
#3450 = ORIENTED_EDGE ( 'NONE', *, *, #25757, .F. ) ;
#3451 = CARTESIAN_POINT ( 'NONE',  ( 173.6922820468853104, -1.999999999999969580, -15.07341522555727664 ) ) ;
#3452 = CARTESIAN_POINT ( 'NONE',  ( 22.52525573827019301, -5.869110285238294367, -18.12586539066504798 ) ) ;
#3453 = CARTESIAN_POINT ( 'NONE',  ( 19.78633661418711043, -4.982883274218824710, -16.00186916550291727 ) ) ;
#3454 = ORIENTED_EDGE ( 'NONE', *, *, #27182, .T. ) ;
#3455 = STYLED_ITEM ( 'NONE', ( #3298 ), #11247 ) ;
#3456 = CARTESIAN_POINT ( 'NONE',  ( 26.08768104250457753, -11.87935956797728210, -17.28510650846989805 ) ) ;
#3457 = VECTOR ( 'NONE', #21931, 999.9999999999998863 ) ;
#3458 = DIRECTION ( 'NONE',  ( -1.000000000000000000, 0.000000000000000000, 0.000000000000000000 ) ) ;
#3459 = VECTOR ( 'NONE', #10492, 1000.000000000000000 ) ;
#3460 = ORIENTED_EDGE ( 'NONE', *, *, #10987, .T. ) ;
#3461 = CARTESIAN_POINT ( 'NONE',  ( 4.000000000000010658, -2.309401076758560656, -2.450000000000000178 ) ) ;
#3462 = CARTESIAN_POINT ( 'NONE',  ( 169.5152310637604387, -4.999999999999971578, -2.627941064794695691 ) ) ;
#3463 = DIRECTION ( 'NONE',  ( 1.000000000000000000, 0.000000000000000000, 0.000000000000000000 ) ) ;
#3464 = CARTESIAN_POINT ( 'NONE',  ( 34.41982446195410716, -12.62108234628556680, -19.94648786050102274 ) ) ;
#3465 = CARTESIAN_POINT ( 'NONE',  ( 9.997747326010761881, 16.03441129093729245, -16.47093000352221637 ) ) ;
#3466 = CARTESIAN_POINT ( 'NONE',  ( 174.7287565553228319, -9.999999999999996447, 0.8205080756887930260 ) ) ;
#3467 = DIRECTION ( 'NONE',  ( -0.000000000000000000, -0.000000000000000000, 1.000000000000000000 ) ) ;
#3468 = CARTESIAN_POINT ( 'NONE',  ( 13.55939796120610019, 8.763434079353435990, -15.56458004748339619 ) ) ;
#3469 = CARTESIAN_POINT ( 'NONE',  ( 132.2287565553230024, -10.00000000000000888, -3.509618943233403510 ) ) ;
#3470 = ORIENTED_EDGE ( 'NONE', *, *, #5328, .T. ) ;
#3471 = LINE ( 'NONE', #6212, #13421 ) ;
#3472 = VECTOR ( 'NONE', #13062, 1000.000000000000000 ) ;
#3473 = ORIENTED_EDGE ( 'NONE', *, *, #2007, .T. ) ;
#3474 = AXIS2_PLACEMENT_3D ( 'NONE', #8157, #28824, #19302 ) ;
#3475 = DIRECTION ( 'NONE',  ( -0.8090169943749474513, -2.183098979609982436E-16, 0.5877852522924731371 ) ) ;
#3476 = LINE ( 'NONE', #12768, #8320 ) ;
#3477 = ADVANCED_FACE ( 'NONE', ( #25560 ), #5110, .F. ) ;
#3478 = EDGE_CURVE ( 'NONE', #27514, #28443, #27899, .T. ) ;
#3479 = LINE ( 'NONE', #12462, #17572 ) ;
#3480 = ORIENTED_EDGE ( 'NONE', *, *, #6299, .T. ) ;
#3481 = EDGE_CURVE ( 'NONE', #14185, #102, #7415, .T. ) ;
#3482 = ORIENTED_EDGE ( 'NONE', *, *, #29290, .T. ) ;
#3483 = EDGE_CURVE ( 'NONE', #10508, #28576, #14252, .T. ) ;
#3484 = CARTESIAN_POINT ( 'NONE',  ( 11.22423757029256741, 9.089670537749404033, -17.24146249637195183 ) ) ;
#3485 = ORIENTED_EDGE ( 'NONE', *, *, #18589, .T. ) ;
#3486 = ORIENTED_EDGE ( 'NONE', *, *, #5155, .F. ) ;
#3487 = PRESENTATION_LAYER_ASSIGNMENT (  '', '', ( #3963 ) ) ;
#3488 = CARTESIAN_POINT ( 'NONE',  ( 26.88742137321887427, -10.86886578961255978, -19.57440296808016100 ) ) ;
#3489 = CARTESIAN_POINT ( 'NONE',  ( 22.33774198005919587, -7.088069534354142220, -17.87445411435389886 ) ) ;
#3490 = CARTESIAN_POINT ( 'NONE',  ( 86.45715817750404142, -4.999999999999993783, 62.81480226644314513 ) ) ;
#3491 = CARTESIAN_POINT ( 'NONE',  ( 137.2287565553230309, -10.00000000000000533, -3.509618943233403510 ) ) ;
#3492 = CARTESIAN_POINT ( 'NONE',  ( -24.00000000000017053, 34.64101615137744972, 4.999999999999998224 ) ) ;
#3493 = VERTEX_POINT ( 'NONE', #4807 ) ;
#3494 = ORIENTED_EDGE ( 'NONE', *, *, #25411, .T. ) ;
#3495 = LINE ( 'NONE', #28709, #20620 ) ;
#3496 = VECTOR ( 'NONE', #5726, 1000.000000000000000 ) ;
#3497 = DIRECTION ( 'NONE',  ( 1.000000000000000000, 0.000000000000000000, 1.387778780781445922E-16 ) ) ;
#3498 = VECTOR ( 'NONE', #15993, 1000.000000000000000 ) ;
#3499 = ORIENTED_EDGE ( 'NONE', *, *, #9963, .F. ) ;
#3500 = DIRECTION ( 'NONE',  ( 1.000000000000000000, 0.000000000000000000, -0.000000000000000000 ) ) ;
#3501 = CARTESIAN_POINT ( 'NONE',  ( 142.2287565553230309, -1.999999999999978018, -29.49038105676660138 ) ) ;
#3502 = CARTESIAN_POINT ( 'NONE',  ( 13.12216094266758581, 8.570213704404382682, -15.91306547940487448 ) ) ;
#3503 = CARTESIAN_POINT ( 'NONE',  ( 35.13870703111577143, -20.34311121210408757, -20.23074448643712486 ) ) ;
#3504 = ORIENTED_EDGE ( 'NONE', *, *, #22671, .T. ) ;
#3505 = CARTESIAN_POINT ( 'NONE',  ( 9.112223960064733674, 16.18277766892301983, -17.05485288603163951 ) ) ;
#3506 = CARTESIAN_POINT ( 'NONE',  ( 26.04489551603160180, -6.130266781319400948, -13.71289979607875154 ) ) ;
#3507 = CARTESIAN_POINT ( 'NONE',  ( 10.35865005771744762, 16.97212102856341787, -17.91352035578586310 ) ) ;
#3508 = FACE_BOUND ( 'NONE', #13244, .T. ) ;
#3509 = ORIENTED_EDGE ( 'NONE', *, *, #11404, .F. ) ;
#3510 = LINE ( 'NONE', #13103, #9532 ) ;
#3511 = ORIENTED_EDGE ( 'NONE', *, *, #29290, .F. ) ;
#3512 = CARTESIAN_POINT ( 'NONE',  ( 12.50016782010997751, 8.570776461014483871, -15.13004124836345632 ) ) ;
#3513 = CARTESIAN_POINT ( 'NONE',  ( 132.0152310637605808, -4.999999999999982236, -24.27857615940569147 ) ) ;
#3514 = ORIENTED_EDGE ( 'NONE', *, *, #5438, .T. ) ;
#3515 = CARTESIAN_POINT ( 'NONE',  ( 13.00000000000000178, -2.870178842070716726E-15, 23.00000000000000000 ) ) ;
#3516 = VERTEX_POINT ( 'NONE', #23742 ) ;
#3517 = ADVANCED_FACE ( 'NONE', ( #20981 ), #20825, .T. ) ;
#3518 = CARTESIAN_POINT ( 'NONE',  ( 13.05603179413191839, 8.545058472539723837, -15.96546128479914373 ) ) ;
#3519 = EDGE_LOOP ( 'NONE', ( #20293, #10582, #11280, #18291 ) ) ;
#3520 = CARTESIAN_POINT ( 'NONE',  ( 21.27922114827105204, 3.617311378231426566, -20.53498548623805675 ) ) ;
#3521 = CARTESIAN_POINT ( 'NONE',  ( 19.69280650922798515, 8.111729275751024204, -19.45082099569356160 ) ) ;
#3522 = CARTESIAN_POINT ( 'NONE',  ( 163.6922820468853672, -4.999999999999974243, -26.58683881228715862 ) ) ;
#3523 = ORIENTED_EDGE ( 'NONE', *, *, #14405, .F. ) ;
#3524 = CARTESIAN_POINT ( 'NONE',  ( 36.30362226317071617, -21.08398799169651738, -20.22680612736627026 ) ) ;
#3525 = ORIENTED_EDGE ( 'NONE', *, *, #22283, .T. ) ;
#3526 = CARTESIAN_POINT ( 'NONE',  ( 15.78240017141095741, 4.038647184180326200, -18.77507866864583619 ) ) ;
#3527 = VECTOR ( 'NONE', #675, 1000.000000000000000 ) ;
#3528 = FILL_AREA_STYLE_COLOUR ( '', #18328 ) ;
#3529 = DIRECTION ( 'NONE',  ( -1.110223024625156540E-16, 0.000000000000000000, -1.000000000000000000 ) ) ;
#3530 = VECTOR ( 'NONE', #15251, 1000.000000000000000 ) ;
#3531 = ADVANCED_FACE ( 'NONE', ( #16715 ), #7554, .T. ) ;
#3532 = PLANE ( 'NONE',  #14588 ) ;
#3533 = CARTESIAN_POINT ( 'NONE',  ( 35.13870703111577143, -20.34311121210408757, -20.23074448643712486 ) ) ;
#3534 = CARTESIAN_POINT ( 'NONE',  ( 158.6922820468854241, -1.999999999999974021, -32.39392330124607611 ) ) ;
#3535 = ORIENTED_EDGE ( 'NONE', *, *, #29533, .T. ) ;
#3536 = CARTESIAN_POINT ( 'NONE',  ( 17.11749389674364963, -5.000000000000013323, -52.68222916370584130 ) ) ;
#3537 = CARTESIAN_POINT ( 'NONE',  ( 12.27692691330339514, 9.494559429826583852, -15.31068279593241144 ) ) ;
#3538 = DIRECTION ( 'NONE',  ( 0.3090169943749472292, 8.338696094057992503E-17, -0.9510565162951536422 ) ) ;
#3539 = LINE ( 'NONE', #22146, #28159 ) ;
#3540 = ORIENTED_EDGE ( 'NONE', *, *, #24659, .F. ) ;
#3541 = CARTESIAN_POINT ( 'NONE',  ( 12.49664108868010182, 8.569232744350554043, -15.13285098609708790 ) ) ;
#3542 = ORIENTED_EDGE ( 'NONE', *, *, #8065, .T. ) ;
#3543 = AXIS2_PLACEMENT_3D ( 'NONE', #15895, #13310, #22633 ) ;
#3544 = CARTESIAN_POINT ( 'NONE',  ( 11.38288633050183307, 7.831121701799675705, -15.95859485361821939 ) ) ;
#3545 = DIRECTION ( 'NONE',  ( -0.5877852522924731371, 0.000000000000000000, 0.8090169943749474513 ) ) ;
#3546 = DIRECTION ( 'NONE',  ( 0.9510565162951535312, 2.566386769018988816E-16, -0.3090169943749475623 ) ) ;
#3547 = ADVANCED_FACE ( 'NONE', ( #19149 ), #9741, .F. ) ;
#3548 = VERTEX_POINT ( 'NONE', #21282 ) ;
#3549 = DIRECTION ( 'NONE',  ( -0.8090169943749474513, -2.183098979609982436E-16, -0.5877852522924731371 ) ) ;
#3550 = EDGE_LOOP ( 'NONE', ( #25606, #8516, #3369, #29957 ) ) ;
#3551 = CARTESIAN_POINT ( 'NONE',  ( 12.81197645932666163, 9.633610080622574401, -16.14942406932820163 ) ) ;
#3552 = ORIENTED_EDGE ( 'NONE', *, *, #27900, .T. ) ;
#3553 = CARTESIAN_POINT ( 'NONE',  ( 33.94960473074984009, -11.12362044852780407, -17.82291586202971700 ) ) ;
#3554 = CARTESIAN_POINT ( 'NONE',  ( 23.66272512268759343, 2.894330346666426745, -16.12005855839824520 ) ) ;
#3555 = VERTEX_POINT ( 'NONE', #4655 ) ;
#3556 = LINE ( 'NONE', #3407, #27249 ) ;
#3557 = VECTOR ( 'NONE', #14688, 1000.000000000000000 ) ;
#3558 = CARTESIAN_POINT ( 'NONE',  ( 28.19717681610909210, -11.01075670644066662, -19.96981485020118541 ) ) ;
#3559 = LINE ( 'NONE', #22479, #2414 ) ;
#3560 = CARTESIAN_POINT ( 'NONE',  ( -3.149999999999999023, -1.013117269296279552E-15, 1.700000000000000178 ) ) ;
#3561 = VERTEX_POINT ( 'NONE', #30208 ) ;
#3562 =( NAMED_UNIT ( * ) PLANE_ANGLE_UNIT ( ) SI_UNIT ( $, .RADIAN. ) );
#3563 = CARTESIAN_POINT ( 'NONE',  ( 20.53420570626898822, -0.4664991210283321310, -19.04361528682417415 ) ) ;
#3564 = CARTESIAN_POINT ( 'NONE',  ( 19.61234978942155038, 5.539603999143367652, -15.30853080630118512 ) ) ;
#3565 = ORIENTED_EDGE ( 'NONE', *, *, #25043, .T. ) ;
#3566 = EDGE_LOOP ( 'NONE', ( #23777, #5741, #3837 ) ) ;
#3567 = DIRECTION ( 'NONE',  ( 0.8660254037844369313, 0.5000000000000028866, 0.000000000000000000 ) ) ;
#3568 = CARTESIAN_POINT ( 'NONE',  ( 129.5152310637605524, -10.00000000000000888, -13.05155085951650840 ) ) ;
#3569 = LINE ( 'NONE', #14312, #16259 ) ;
#3570 = EDGE_CURVE ( 'NONE', #20929, #27090, #9217, .T. ) ;
#3571 = EDGE_CURVE ( 'NONE', #30215, #16128, #28205, .T. ) ;
#3572 = CARTESIAN_POINT ( 'NONE',  ( 176.1922820468853104, -1.999999999999969358, -22.25671179336496053 ) ) ;
#3573 = FACE_OUTER_BOUND ( 'NONE', #7576, .T. ) ;
#3574 = EDGE_CURVE ( 'NONE', #12466, #26303, #393, .T. ) ;
#3575 = LINE ( 'NONE', #1739, #27088 ) ;
#3576 = VECTOR ( 'NONE', #17067, 1000.000000000000000 ) ;
#3577 = CARTESIAN_POINT ( 'NONE',  ( 11.46269231744662420, 9.315986823159681407, -15.86512371708112212 ) ) ;
#3578 = CARTESIAN_POINT ( 'NONE',  ( 17.17204249742301059, 10.23148044644768362, -15.96021614775051667 ) ) ;
#3579 = CARTESIAN_POINT ( 'NONE',  ( 29.30807694892355286, -8.357723062633453992, -13.20244061823602522 ) ) ;
#3580 = EDGE_LOOP ( 'NONE', ( #8529, #9094, #5921, #30149 ) ) ;
#3581 = CARTESIAN_POINT ( 'NONE',  ( 134.5152310637605524, -10.00000000000000533, -30.37205893520530964 ) ) ;
#3582 = LINE ( 'NONE', #1000, #19919 ) ;
#3583 = CARTESIAN_POINT ( 'NONE',  ( 141.1922820468854525, -10.00000000000000533, -10.74328820663507678 ) ) ;
#3584 = LINE ( 'NONE', #22188, #8766 ) ;
#3585 =( NAMED_UNIT ( * ) PLANE_ANGLE_UNIT ( ) SI_UNIT ( $, .RADIAN. ) );
#3586 = CARTESIAN_POINT ( 'NONE',  ( 21.40051611374530793, -0.1690565882708310874, -20.18282279970310000 ) ) ;
#3587 = ORIENTED_EDGE ( 'NONE', *, *, #14990, .T. ) ;
#3588 = CARTESIAN_POINT ( 'NONE',  ( 420.0000000000002274, 34.64101615137744972, 12.00000000000000178 ) ) ;
#3589 = CARTESIAN_POINT ( 'NONE',  ( 12.27644674946102832, 9.496504630232381672, -15.31090095340427304 ) ) ;
#3590 = CARTESIAN_POINT ( 'NONE',  ( 164.5152310637604671, -1.999999999999972689, -2.627941064794695691 ) ) ;
#3591 = CARTESIAN_POINT ( 'NONE',  ( 18.50902107916489570, 2.085137940960992697, -20.06823964296112450 ) ) ;
#3592 = DIRECTION ( 'NONE',  ( 0.000000000000000000, -2.775557561562890735E-17, 1.000000000000000000 ) ) ;
#3593 = CARTESIAN_POINT ( 'NONE',  ( 20.23665759668125474, 8.554704514664523529, -15.35188933034790182 ) ) ;
#3594 = VERTEX_POINT ( 'NONE', #12724 ) ;
#3595 = PLANE ( 'NONE',  #15896 ) ;
#3596 = CARTESIAN_POINT ( 'NONE',  ( 28.15806058933612022, -5.108324757233392077, -18.51472486207664758 ) ) ;
#3597 = CARTESIAN_POINT ( 'NONE',  ( 22.44149885728860028, -8.037961521189897596, -18.19026436706728234 ) ) ;
#3598 = VECTOR ( 'NONE', #28495, 1000.000000000000000 ) ;
#3599 = ORIENTED_EDGE ( 'NONE', *, *, #2566, .F. ) ;
#3600 = EDGE_CURVE ( 'NONE', #22117, #3702, #24404, .T. ) ;
#3601 = CARTESIAN_POINT ( 'NONE',  ( 429.0000000000002274, 34.64101615137744972, 12.00000000000000178 ) ) ;
#3602 = LINE ( 'NONE', #12897, #26508 ) ;
#3603 = VERTEX_POINT ( 'NONE', #12422 ) ;
#3604 = EDGE_CURVE ( 'NONE', #12245, #8342, #21890, .T. ) ;
#3605 = DIRECTION ( 'NONE',  ( 0.000000000000000000, 0.000000000000000000, -1.000000000000000000 ) ) ;
#3606 = DIRECTION ( 'NONE',  ( 0.5000000000000066613, 0.8660254037844349329, 0.000000000000000000 ) ) ;
#3607 = EDGE_CURVE ( 'NONE', #15349, #12234, #3147, .T. ) ;
#3608 = EDGE_CURVE ( 'NONE', #23763, #18633, #6018, .T. ) ;
#3609 = CARTESIAN_POINT ( 'NONE',  ( 163.6922820468852819, -4.999999999999973355, -0.6060766987539614181 ) ) ;
#3610 = ADVANCED_FACE ( 'NONE', ( #10429 ), #10133, .T. ) ;
#3611 = CARTESIAN_POINT ( 'NONE',  ( 148.6922820468854241, -4.999999999999977796, -17.92658477444275889 ) ) ;
#3612 = CARTESIAN_POINT ( 'NONE',  ( 28.02170931380428698, -7.325026966936788675, -12.85224998211816860 ) ) ;
#3613 = CARTESIAN_POINT ( 'NONE',  ( 10.00000000000008527, 17.32050807568872486, -30.00000000000000711 ) ) ;
#3614 = CARTESIAN_POINT ( 'NONE',  ( 33.97319001242765779, -11.13623552147873141, -19.50814438409551954 ) ) ;
#3615 = CARTESIAN_POINT ( 'NONE',  ( 176.1922820468853388, -9.999999999999994671, -28.06379628232387802 ) ) ;
#3616 = CARTESIAN_POINT ( 'NONE',  ( 9.918725397012197575, 16.39681593027784956, -16.50360835092378409 ) ) ;
#3617 = CONICAL_SURFACE ( 'NONE', #7984, 4.000000000000003553, 1.047197551196597853 ) ;
#3618 = CARTESIAN_POINT ( 'NONE',  ( 63.44486372867152824, -29.99999999999998934, -15.00000000000000000 ) ) ;
#3619 = CARTESIAN_POINT ( 'NONE',  ( 5.637851296924623057E-15, 9.237604307034036566, -4.285468820183664818 ) ) ;
#3620 = CARTESIAN_POINT ( 'NONE',  ( 13.12341270237516078, 8.570764515250925086, -15.91206798513452192 ) ) ;
#3621 = CARTESIAN_POINT ( 'NONE',  ( 131.1922820468854241, -10.00000000000000888, -22.25671179336495697 ) ) ;
#3622 = PLANE ( 'NONE',  #29074 ) ;
#3623 = ORIENTED_EDGE ( 'NONE', *, *, #21344, .F. ) ;
#3624 = CARTESIAN_POINT ( 'NONE',  ( 162.0152310637604103, -4.999999999999974243, -1.798730398669517009E-14 ) ) ;
#3625 = CARTESIAN_POINT ( 'NONE',  ( 173.6922820468852535, -1.999999999999970468, 2.247092850131519715 ) ) ;
#3626 = CARTESIAN_POINT ( 'NONE',  ( 171.1922820468852819, -9.999999999999996447, -2.083034168790677043 ) ) ;
#3627 = ORIENTED_EDGE ( 'NONE', *, *, #23084, .F. ) ;
#3628 = VERTEX_POINT ( 'NONE', #9979 ) ;
#3629 = CARTESIAN_POINT ( 'NONE',  ( 8.944584683310379702, 16.95159276115599667, -17.91796598306941135 ) ) ;
#3630 = CARTESIAN_POINT ( 'NONE',  ( 16.69609108537820674, 9.478167028156011753, -20.90851310094495474 ) ) ;
#3631 = CARTESIAN_POINT ( 'NONE',  ( 30.27313844582349489, -8.115497507854934511, -14.41531361995715876 ) ) ;
#3632 = PLANE ( 'NONE',  #22856 ) ;
#3633 = PLANE ( 'NONE',  #14533 ) ;
#3634 = DIRECTION ( 'NONE',  ( 0.000000000000000000, -0.4999999999999993894, 0.8660254037844389297 ) ) ;
#3635 = VECTOR ( 'NONE', #26212, 1000.000000000000000 ) ;
#3636 = ORIENTED_EDGE ( 'NONE', *, *, #29447, .F. ) ;
#3637 = LINE ( 'NONE', #10647, #154 ) ;
#3639 = EDGE_LOOP ( 'NONE', ( #9050, #22822, #15923, #16135, #21280 ) ) ;
#3638 = DIRECTION ( 'NONE',  ( -0.06678507476159963041, 0.9947851038922184141, -0.07708664516786083165 ) ) ;
#3640 = EDGE_CURVE ( 'NONE', #8714, #19917, #8145, .T. ) ;
#3641 = APPLICATION_CONTEXT ( 'automotive_design' ) ;
#3642 = LINE ( 'NONE', #17222, #3459 ) ;
#3643 = FACE_OUTER_BOUND ( 'NONE', #1172, .T. ) ;
#3644 = EDGE_CURVE ( 'NONE', #11898, #24567, #24488, .T. ) ;
#3645 = EDGE_CURVE ( 'NONE', #27580, #29940, #3295, .T. ) ;
#3646 = EDGE_CURVE ( 'NONE', #28740, #7514, #22998, .T. ) ;
#3647 = CARTESIAN_POINT ( 'NONE',  ( 12.04525852301462585, 9.245982119944198274, -16.68353927915122981 ) ) ;
#3648 = CARTESIAN_POINT ( 'NONE',  ( 32.25667210025905263, -11.64161264113965011, -15.27003429613047025 ) ) ;
#3649 = ORIENTED_EDGE ( 'NONE', *, *, #26284, .T. ) ;
#3650 = CARTESIAN_POINT ( 'NONE',  ( 8.946690830082905777, 16.94193370358561879, -17.78270686867927708 ) ) ;
#3651 = ORIENTED_EDGE ( 'NONE', *, *, #18862, .T. ) ;
#3652 = CARTESIAN_POINT ( 'NONE',  ( 25.31619048431776875, -0.2099727537683927225, -15.56338435260822628 ) ) ;
#3653 = CARTESIAN_POINT ( 'NONE',  ( 12.86836073382838563, 9.516082146233362238, -16.11534891376273748 ) ) ;
#3654 = FACE_BOUND ( 'NONE', #4449, .T. ) ;
#3655 = ORIENTED_EDGE ( 'NONE', *, *, #23252, .T. ) ;
#3656 = ORIENTED_EDGE ( 'NONE', *, *, #20407, .T. ) ;
#3657 = DIRECTION ( 'NONE',  ( 2.698458740408365879E-16, -1.000000000000000000, 0.000000000000000000 ) ) ;
#3658 = VECTOR ( 'NONE', #7406, 1000.000000000000000 ) ;
#3659 = CARTESIAN_POINT ( 'NONE',  ( 11.48249212886396897, 9.228508165798535501, -15.85668214399537845 ) ) ;
#3660 = LINE ( 'NONE', #14634, #18888 ) ;
#3661 = EDGE_LOOP ( 'NONE', ( #23442, #28271, #21830, #25501 ) ) ;
#3662 = CARTESIAN_POINT ( 'NONE',  ( 9.806324804231010717, -5.000000000000015099, 30.18076441017510803 ) ) ;
#3663 = ORIENTED_EDGE ( 'NONE', *, *, #16797, .F. ) ;
#3664 = CARTESIAN_POINT ( 'NONE',  ( 9.661883079970770893, 16.25482654942367233, -17.91569817988508362 ) ) ;
#3665 = ORIENTED_EDGE ( 'NONE', *, *, #29249, .T. ) ;
#3666 = CARTESIAN_POINT ( 'NONE',  ( 14.64418905516944314, 2.941711854493593403, -16.63492386420942282 ) ) ;
#3667 = CARTESIAN_POINT ( 'NONE',  ( 20.94368124868196901, 3.275021729503806878, -20.72479390824751633 ) ) ;
#3668 = DIRECTION ( 'NONE',  ( 1.000000000000000000, 0.000000000000000000, 0.000000000000000000 ) ) ;
#3669 = ORIENTED_EDGE ( 'NONE', *, *, #14273, .T. ) ;
#3670 = CARTESIAN_POINT ( 'NONE',  ( -13.00000000000001243, 55.00000000000000711, 23.00000000000000000 ) ) ;
#3671 = VECTOR ( 'NONE', #21317, 1000.000000000000000 ) ;
#3672 = CARTESIAN_POINT ( 'NONE',  ( 19.05868480923028940, 8.129737193291200370, -16.02886444249750042 ) ) ;
#3673 = CYLINDRICAL_SURFACE ( 'NONE', #26664, 5.000000000000000000 ) ;
#3674 = FACE_BOUND ( 'NONE', #15846, .T. ) ;
#3675 = EDGE_CURVE ( 'NONE', #28746, #9780, #15303, .T. ) ;
#3676 = VECTOR ( 'NONE', #21236, 1000.000000000000000 ) ;
#3677 = ORIENTED_EDGE ( 'NONE', *, *, #29652, .T. ) ;
#3678 = EDGE_CURVE ( 'NONE', #19490, #2471, #692, .T. ) ;
#3679 = CARTESIAN_POINT ( 'NONE',  ( 156.1922820468854241, -10.00000000000000000, -28.06379628232387802 ) ) ;
#3680 = CARTESIAN_POINT ( 'NONE',  ( 32.77977724007769211, -11.13765286058784554, -18.71157503069099448 ) ) ;
#3681 = CARTESIAN_POINT ( 'NONE',  ( -4.250000000000003553, -1.366904252225140556E-15, -5.000000000000000888 ) ) ;
#3682 = ORIENTED_EDGE ( 'NONE', *, *, #1080, .F. ) ;
#3683 = LINE ( 'NONE', #12983, #14852 ) ;
#3684 = CARTESIAN_POINT ( 'NONE',  ( 12.27235684156208961, 9.528132359803098694, -15.31161062812042317 ) ) ;
#3685 = EDGE_LOOP ( 'NONE', ( #14827, #17290, #18917, #9630 ) ) ;
#3686 = DIRECTION ( 'NONE',  ( 0.9510565162951536422, 2.566386769018988816E-16, 0.3090169943749472292 ) ) ;
#3687 = ORIENTED_EDGE ( 'NONE', *, *, #24489, .F. ) ;
#3688 = DIRECTION ( 'NONE',  ( 0.000000000000000000, 0.000000000000000000, 1.000000000000000000 ) ) ;
#3689 = ORIENTED_EDGE ( 'NONE', *, *, #19397, .T. ) ;
#3690 = CIRCLE ( 'NONE', #28101, 8.000000000000007105 ) ;
#3691 = CARTESIAN_POINT ( 'NONE',  ( 10.67054149815029618, 9.036200773601834157, -16.41042721873081689 ) ) ;
#3692 = FACE_OUTER_BOUND ( 'NONE', #3685, .T. ) ;
#3693 = FACE_OUTER_BOUND ( 'NONE', #28279, .T. ) ;
#3694 = ORIENTED_EDGE ( 'NONE', *, *, #15888, .T. ) ;
#3695 = DIRECTION ( 'NONE',  ( 0.9510565162951535312, 2.566386769018988816E-16, -0.3090169943749475623 ) ) ;
#3696 = ORIENTED_EDGE ( 'NONE', *, *, #25754, .F. ) ;
#3697 = CARTESIAN_POINT ( 'NONE',  ( 12.83226850357503501, 9.540548187773516986, -16.14103259455261608 ) ) ;
#3699 = CARTESIAN_POINT ( 'NONE',  ( 34.22536682013040377, -11.37642754387024979, -18.47965768629886085 ) ) ;
#3698 = AXIS2_PLACEMENT_3D ( 'NONE', #26593, #28769, #19699 ) ;
#3700 = CARTESIAN_POINT ( 'NONE',  ( 20.72626264887238534, -1.914771856900582714, -13.62749948506543518 ) ) ;
#3701 = ORIENTED_EDGE ( 'NONE', *, *, #8983, .T. ) ;
#3702 = VERTEX_POINT ( 'NONE', #28960 ) ;
#3703 = AXIS2_PLACEMENT_3D ( 'NONE', #11367, #2997, #12273 ) ;
#3704 = CARTESIAN_POINT ( 'NONE',  ( 174.5152310637604387, -9.999999999999994671, -21.71180489736091346 ) ) ;
#3705 = CARTESIAN_POINT ( 'NONE',  ( 26.19910047366428429, -13.48590472426672626, -13.82108881675422829 ) ) ;
#3706 = VERTEX_POINT ( 'NONE', #17162 ) ;
#3707 = DIRECTION ( 'NONE',  ( 0.5877852522924731371, 1.586114251531760728E-16, 0.8090169943749474513 ) ) ;
#3708 = ADVANCED_FACE ( 'NONE', ( #29263 ), #12873, .T. ) ;
#3709 =( NAMED_UNIT ( * ) SI_UNIT ( $, .STERADIAN. ) SOLID_ANGLE_UNIT ( ) );
#3710 = CARTESIAN_POINT ( 'NONE',  ( 30.27313844582349489, -8.115497507854934511, -14.41531361995715876 ) ) ;
#3711 = AXIS2_PLACEMENT_3D ( 'NONE', #28349, #25553, #6799 ) ;
#3712 = CARTESIAN_POINT ( 'NONE',  ( 20.76503381105741397, 0.5146303624313508518, -20.54264311693622602 ) ) ;
#3713 = VERTEX_POINT ( 'NONE', #29107 ) ;
#3714 = ORIENTED_EDGE ( 'NONE', *, *, #815, .F. ) ;
#3715 = DIRECTION ( 'NONE',  ( 0.3090169943749472292, 8.338696094057992503E-17, -0.9510565162951536422 ) ) ;
#3716 = LINE ( 'NONE', #26785, #28266 ) ;
#3717 = VECTOR ( 'NONE', #5427, 1000.000000000000000 ) ;
#3718 = DIRECTION ( 'NONE',  ( -2.698458740408365879E-16, 1.000000000000000000, 0.000000000000000000 ) ) ;
#3719 = DIRECTION ( 'NONE',  ( -1.110223024625156540E-16, 0.000000000000000000, -1.000000000000000000 ) ) ;
#3720 = CARTESIAN_POINT ( 'NONE',  ( 134.5152310637605808, -10.00000000000000533, -28.60870317832789311 ) ) ;
#3721 = VECTOR ( 'NONE', #25280, 1000.000000000000000 ) ;
#3722 = DIRECTION ( 'NONE',  ( 1.000000000000000000, 0.000000000000000000, 0.000000000000000000 ) ) ;
#3723 = AXIS2_PLACEMENT_3D ( 'NONE', #1241, #5667, #14947 ) ;
#3724 = CARTESIAN_POINT ( 'NONE',  ( 13.35290877858212255, 7.614465999429414822, -15.72913170295453966 ) ) ;
#3725 = ORIENTED_EDGE ( 'NONE', *, *, #25254, .T. ) ;
#3726 = CARTESIAN_POINT ( 'NONE',  ( 16.84948243412402036, 10.49281628697410262, -11.66356073909478575 ) ) ;
#3727 = CARTESIAN_POINT ( 'NONE',  ( 24.40455984355908114, -10.10244183743681035, -17.68366952546245585 ) ) ;
#3728 = ORIENTED_EDGE ( 'NONE', *, *, #21754, .F. ) ;
#3729 = FACE_OUTER_BOUND ( 'NONE', #23065, .T. ) ;
#3730 = LINE ( 'NONE', #17602, #29725 ) ;
#3731 = ORIENTED_EDGE ( 'NONE', *, *, #2071, .F. ) ;
#3732 = CARTESIAN_POINT ( 'NONE',  ( 9.893572868141015775, 16.51216863388285461, -16.51808063826580408 ) ) ;
#3733 = CARTESIAN_POINT ( 'NONE',  ( -4.000000000000003553, -0.7779732554280821555, -2.416455648918319987 ) ) ;
#3735 = ORIENTED_EDGE ( 'NONE', *, *, #11286, .F. ) ;
#3734 = CARTESIAN_POINT ( 'NONE',  ( 25.57370974413349884, -0.4222200280313516685, -16.88676729435558599 ) ) ;
#3736 = ORIENTED_EDGE ( 'NONE', *, *, #11470, .F. ) ;
#3737 = DIRECTION ( 'NONE',  ( 2.908569913943825554E-16, -1.000000000000000000, -0.000000000000000000 ) ) ;
#3738 = CARTESIAN_POINT ( 'NONE',  ( 11.04501277462238029, 15.14427510452705583, -15.82012259674246657 ) ) ;
#3739 = CARTESIAN_POINT ( 'NONE',  ( 32.67186286342521839, -11.06527230177895227, -18.43913201350460440 ) ) ;
#3740 = DIRECTION ( 'NONE',  ( -0.9510565162951536422, -2.566386769018988816E-16, -0.3090169943749472292 ) ) ;
#3741 = CARTESIAN_POINT ( 'NONE',  ( 25.07290406138036687, -9.006318079059196791, -17.79994936451110732 ) ) ;
#3742 = CARTESIAN_POINT ( 'NONE',  ( 0.000000000000000000, 0.000000000000000000, -2.450000000000000622 ) ) ;
#3743 = CARTESIAN_POINT ( 'NONE',  ( 21.98221344960014889, 4.819993630401092410, -14.81438138791982162 ) ) ;
#3744 = ORIENTED_EDGE ( 'NONE', *, *, #5489, .F. ) ;
#3745 = CARTESIAN_POINT ( 'NONE',  ( 147.2287565553229740, -1.999999999999977129, -3.509618943233403510 ) ) ;
#3746 = EDGE_CURVE ( 'NONE', #9765, #2890, #24338, .T. ) ;
#3747 = SURFACE_STYLE_USAGE ( .BOTH. , #24352 ) ;
#3748 = CARTESIAN_POINT ( 'NONE',  ( 23.96437976099892708, -9.208260125601851698, -18.67152130837153123 ) ) ;
#3749 = EDGE_CURVE ( 'NONE', #27863, #4596, #19685, .T. ) ;
#3750 = CARTESIAN_POINT ( 'NONE',  ( 23.15972007162554291, -8.148303969466700991, -13.79129035937103431 ) ) ;
#3751 = VECTOR ( 'NONE', #23392, 1000.000000000000000 ) ;
#3752 = ORIENTED_EDGE ( 'NONE', *, *, #2596, .T. ) ;
#3753 = ORIENTED_EDGE ( 'NONE', *, *, #5511, .T. ) ;
#3754 = DIRECTION ( 'NONE',  ( -0.5877852522924731371, -1.586114251531760235E-16, 0.8090169943749474513 ) ) ;
#3755 = PRODUCT_DEFINITION_SHAPE ( 'NONE', 'NONE',  #7839 ) ;
#3756 = CARTESIAN_POINT ( 'NONE',  ( 144.5152310637605240, -10.00000000000000355, -4.391296821672111328 ) ) ;
#3757 = VERTEX_POINT ( 'NONE', #7996 ) ;
#3758 = DIRECTION ( 'NONE',  ( 2.908569913943825554E-16, -1.000000000000000000, 0.000000000000000000 ) ) ;
#3759 = CARTESIAN_POINT ( 'NONE',  ( 144.7287565553230024, -1.999999999999977573, -7.839745962155603820 ) ) ;
#3760 = DIRECTION ( 'NONE',  ( -0.5877852522924731371, -1.586114251531760728E-16, -0.8090169943749474513 ) ) ;
#3761 = VECTOR ( 'NONE', #6283, 1000.000000000000000 ) ;
#3762 = DIRECTION ( 'NONE',  ( -0.8090169943749474513, -2.183098979609982436E-16, 0.5877852522924731371 ) ) ;
#3763 = CARTESIAN_POINT ( 'NONE',  ( 26.82298874931487020, -4.830090842487210878, -14.67398021261910301 ) ) ;
#3764 = CARTESIAN_POINT ( 'NONE',  ( 176.1922820468852819, -1.999999999999969358, -10.74328820663507678 ) ) ;
#3765 = CARTESIAN_POINT ( 'NONE',  ( 34.10649047503919462, -12.21345526111254287, -20.89408644300621987 ) ) ;
#3766 = CARTESIAN_POINT ( 'NONE',  ( -7.806255641895631925E-14, -4.618802153517044928, -0.3572655899081716435 ) ) ;
#3767 = VECTOR ( 'NONE', #10364, 1000.000000000000000 ) ;
#3768 = CARTESIAN_POINT ( 'NONE',  ( 9.916551108984865692, 16.40678749232849398, -16.50450761325770443 ) ) ;
#3769 = CARTESIAN_POINT ( 'NONE',  ( 166.1922820468853388, -9.999999999999998224, -10.74328820663507678 ) ) ;
#3770 = CARTESIAN_POINT ( 'NONE',  ( 172.7287565553229456, -9.999999999999971578, -36.50000000000000711 ) ) ;
#3771 = CARTESIAN_POINT ( 'NONE',  ( 9.661883079970770893, 16.25482654942367233, -17.91569817988508362 ) ) ;
#3772 = DIRECTION ( 'NONE',  ( 1.000000000000000000, 4.440892098500622217E-16, 0.000000000000000000 ) ) ;
#3773 = LINE ( 'NONE', #10924, #6612 ) ;
#3774 = CARTESIAN_POINT ( 'NONE',  ( 9.926830210242822972, 16.35964622367879784, -16.50025672554925293 ) ) ;
#3775 = EDGE_LOOP ( 'NONE', ( #13198, #6077, #9123, #12958 ) ) ;
#3776 = CARTESIAN_POINT ( 'NONE',  ( -13.00000000000000178, -2.870178842070716726E-15, -18.00000000000000000 ) ) ;
#3777 = DIRECTION ( 'NONE',  ( 1.000000000000000000, 0.000000000000000000, 0.000000000000000000 ) ) ;
#3778 = DIRECTION ( 'NONE',  ( -0.8090169943749474513, -2.183098979609982436E-16, -0.5877852522924731371 ) ) ;
#3779 = ORIENTED_EDGE ( 'NONE', *, *, #7162, .F. ) ;
#3780 = CARTESIAN_POINT ( 'NONE',  ( 13.65148492087865151, 7.746099194123166498, -15.49118511517110619 ) ) ;
#3781 = CARTESIAN_POINT ( 'NONE',  ( 36.54859390953724585, -23.18451583373416014, -17.78191007148576119 ) ) ;
#3782 = EDGE_CURVE ( 'NONE', #12691, #4011, #3433, .T. ) ;
#3783 = ADVANCED_FACE ( 'NONE', ( #17015 ), #22006, .T. ) ;
#3784 = CARTESIAN_POINT ( 'NONE',  ( 30.21326039400183561, -7.476461571224066738, -17.86537319528562051 ) ) ;
#3785 = ADVANCED_FACE ( 'NONE', ( #11184 ), #8445, .T. ) ;
#3786 = CARTESIAN_POINT ( 'NONE',  ( 22.98083118076628040, -7.181321033737746440, -13.97658420854277850 ) ) ;
#3787 = VECTOR ( 'NONE', #21818, 1000.000000000000000 ) ;
#3788 = LINE ( 'NONE', #29321, #15535 ) ;
#3789 = CARTESIAN_POINT ( 'NONE',  ( 151.1922820468854241, -4.999999999999976907, -19.40354224447947828 ) ) ;
#3790 = EDGE_CURVE ( 'NONE', #4117, #28729, #8735, .T. ) ;
#3791 = FACE_OUTER_BOUND ( 'NONE', #25500, .T. ) ;
#3792 = AXIS2_PLACEMENT_3D ( 'NONE', #16831, #9950, #16984 ) ;
#3793 = VERTEX_POINT ( 'NONE', #8886 ) ;
#3794 = VERTEX_POINT ( 'NONE', #17749 ) ;
#3795 = DIRECTION ( 'NONE',  ( -0.9510565162951536422, -2.566386769018988816E-16, -0.3090169943749472292 ) ) ;
#3797 = ORIENTED_EDGE ( 'NONE', *, *, #9804, .F. ) ;
#3796 = PRESENTATION_STYLE_ASSIGNMENT (( #20554 ) ) ;
#3798 = CARTESIAN_POINT ( 'NONE',  ( 5.000000000000000000, 6.123233995736766282E-16, 18.00000000000000000 ) ) ;
#3799 = LINE ( 'NONE', #13089, #12359 ) ;
#3800 = CARTESIAN_POINT ( 'NONE',  ( 12.05017172662707381, 9.228765020691243492, -16.68110209197688221 ) ) ;
#3801 = CARTESIAN_POINT ( 'NONE',  ( 35.54582861202835886, -21.17209281684672817, -18.49356017204852520 ) ) ;
#3802 = EDGE_LOOP ( 'NONE', ( #12869, #5834, #5457, #26760 ) ) ;
#3803 = CARTESIAN_POINT ( 'NONE',  ( 9.113084692838755885, 16.17883023870341930, -17.05449542622726966 ) ) ;
#3804 = VECTOR ( 'NONE', #9308, 1000.000000000000000 ) ;
#3805 = CARTESIAN_POINT ( 'NONE',  ( 24.68825858685077179, -9.385095155728059524, -16.92495907518576104 ) ) ;
#3806 = CARTESIAN_POINT ( 'NONE',  ( 10.35864918915110877, 16.97212501191939538, -17.92454625180715766 ) ) ;
#3807 = FACE_BOUND ( 'NONE', #8755, .T. ) ;
#3808 = ORIENTED_EDGE ( 'NONE', *, *, #16385, .T. ) ;
#3809 = ORIENTED_EDGE ( 'NONE', *, *, #17753, .T. ) ;
#3810 = VECTOR ( 'NONE', #22162, 1000.000000000000000 ) ;
#3811 = CARTESIAN_POINT ( 'NONE',  ( 172.7287565553229456, -4.999999999999970690, -33.50000000000000000 ) ) ;
#3812 = CARTESIAN_POINT ( 'NONE',  ( 11.47288049726737214, 9.269262779257836371, -15.86091052746238184 ) ) ;
#3813 = CARTESIAN_POINT ( 'NONE',  ( 149.5152310637605808, -4.999999999999976907, -19.94844914048349693 ) ) ;
#3814 = ORIENTED_EDGE ( 'NONE', *, *, #5212, .T. ) ;
#3815 = DIRECTION ( 'NONE',  ( -0.000000000000000000, 1.000000000000000000, -0.000000000000000000 ) ) ;
#3816 = VERTEX_POINT ( 'NONE', #30018 ) ;
#3817 = CARTESIAN_POINT ( 'NONE',  ( 13.12489394565217005, 8.571418981294288031, -15.91088741739120671 ) ) ;
#3818 = ORIENTED_EDGE ( 'NONE', *, *, #21933, .T. ) ;
#3819 = CARTESIAN_POINT ( 'NONE',  ( 19.58395429099637752, 5.031901065175194532, -13.05446103591450147 ) ) ;
#3820 = CARTESIAN_POINT ( 'NONE',  ( 21.27922114827105204, 3.617311378231426566, -20.53498548623805675 ) ) ;
#3821 = EDGE_CURVE ( 'NONE', #2433, #29043, #12772, .T. ) ;
#3822 = CARTESIAN_POINT ( 'NONE',  ( 49.00000000000000000, 7.511012776518210972E-16, -5.000000000000000000 ) ) ;
#3823 = ADVANCED_FACE ( 'NONE', ( #18016 ), #13136, .T. ) ;
#3824 = ORIENTED_EDGE ( 'NONE', *, *, #6947, .F. ) ;
#3825 = EDGE_CURVE ( 'NONE', #29239, #6973, #6852, .T. ) ;
#3826 = CARTESIAN_POINT ( 'NONE',  ( 36.04209255463945993, -19.90907354740926394, -20.43687144983462289 ) ) ;
#3827 = CARTESIAN_POINT ( 'NONE',  ( 18.34549112274340033, 0.9605221043122941227, -13.99314825615798341 ) ) ;
#3828 = VECTOR ( 'NONE', #18384, 1000.000000000000000 ) ;
#3829 = DIRECTION ( 'NONE',  ( -1.000000000000000000, 0.000000000000000000, -0.000000000000000000 ) ) ;
#3830 = CARTESIAN_POINT ( 'NONE',  ( 164.5152310637604955, -1.999999999999971356, -30.37205893520531319 ) ) ;
#3831 = CIRCLE ( 'NONE', #22829, 9.000000000000007105 ) ;
#3832 = ORIENTED_EDGE ( 'NONE', *, *, #4124, .T. ) ;
#3833 = CARTESIAN_POINT ( 'NONE',  ( 152.0152310637605524, -10.00000000000000000, -26.04193191628311155 ) ) ;
#3834 = CARTESIAN_POINT ( 'NONE',  ( 129.5152310637605808, -10.00000000000000888, -19.94844914048349338 ) ) ;
#3835 = DIRECTION ( 'NONE',  ( 0.4108911781748706971, -0.9116843969807022496, 0.000000000000000000 ) ) ;
#3836 = ORIENTED_EDGE ( 'NONE', *, *, #1931, .F. ) ;
#3837 = ORIENTED_EDGE ( 'NONE', *, *, #2310, .F. ) ;
#3838 = DIRECTION ( 'NONE',  ( 1.000000000000000000, 2.698458740408365879E-16, -1.110223024625156540E-16 ) ) ;
#3839 = CARTESIAN_POINT ( 'NONE',  ( 12.24523086077475220, 9.516144614896692389, -15.33323053563244898 ) ) ;
#3840 = CARTESIAN_POINT ( 'NONE',  ( 32.57315965809380742, -11.03986597812349935, -18.16622079659612510 ) ) ;
#3841 = CARTESIAN_POINT ( 'NONE',  ( 25.00000000000000000, 55.00000000000000711, -24.99999999999999289 ) ) ;
#3842 = ORIENTED_EDGE ( 'NONE', *, *, #16064, .T. ) ;
#3843 = LINE ( 'NONE', #29535, #4470 ) ;
#3844 = ORIENTED_EDGE ( 'NONE', *, *, #1004, .T. ) ;
#3845 = CARTESIAN_POINT ( 'NONE',  ( 12.74005437760208181, 7.618877980503234504, -14.93883819022932080 ) ) ;
#3846 = CARTESIAN_POINT ( 'NONE',  ( 176.1922820468853388, -1.999999999999968470, -28.06379628232387802 ) ) ;
#3847 = DIRECTION ( 'NONE',  ( 1.110223024625156540E-16, 2.995891024602366092E-32, 1.000000000000000000 ) ) ;
#3848 = ORIENTED_EDGE ( 'NONE', *, *, #11792, .F. ) ;
#3849 = DIRECTION ( 'NONE',  ( -0.8090169943749474513, -2.183098979609982436E-16, 0.5877852522924731371 ) ) ;
#3850 = ORIENTED_EDGE ( 'NONE', *, *, #24493, .T. ) ;
#3851 = CARTESIAN_POINT ( 'NONE',  ( 10.35864918915110877, 16.97212501191939538, -17.92981046679734547 ) ) ;
#3852 = AXIS2_PLACEMENT_3D ( 'NONE', #6310, #8435, #24626 ) ;
#3853 = CARTESIAN_POINT ( 'NONE',  ( 33.92041909680281719, -11.11917911243856238, -17.74043268107170235 ) ) ;
#3854 = CARTESIAN_POINT ( 'NONE',  ( 22.29983652437130814, 0.6627547066652448304, -20.09853802436992964 ) ) ;
#3855 = VERTEX_POINT ( 'NONE', #6583 ) ;
#3856 = EDGE_CURVE ( 'NONE', #2318, #6495, #8703, .T. ) ;
#3857 = EDGE_CURVE ( 'NONE', #438, #18375, #26915, .T. ) ;
#3858 = DIRECTION ( 'NONE',  ( -0.000000000000000000, -0.000000000000000000, -1.000000000000000000 ) ) ;
#3859 = ADVANCED_FACE ( 'NONE', ( #17563 ), #15871, .T. ) ;
#3860 = CARTESIAN_POINT ( 'NONE',  ( 164.7287565553229740, -1.999999999999970912, -33.82050807568879947 ) ) ;
#3861 = AXIS2_PLACEMENT_3D ( 'NONE', #3146, #5571, #17603 ) ;
#3862 = EDGE_CURVE ( 'NONE', #15686, #5157, #11281, .T. ) ;
#3863 = DIRECTION ( 'NONE',  ( -2.698458740408365879E-16, 1.000000000000000000, 0.000000000000000000 ) ) ;
#3864 = CARTESIAN_POINT ( 'NONE',  ( 24.27430760268559595, -10.23567508289028716, -17.26834523416827949 ) ) ;
#3865 = CARTESIAN_POINT ( 'NONE',  ( 27.87740037347163735, -3.310382910926334521, -16.69022314910379734 ) ) ;
#3866 = ORIENTED_EDGE ( 'NONE', *, *, #11834, .T. ) ;
#3867 = EDGE_LOOP ( 'NONE', ( #11348, #30172, #3454, #2533, #20063 ) ) ;
#3868 = DIRECTION ( 'NONE',  ( -0.9510565162951536422, 0.000000000000000000, -0.3090169943749472292 ) ) ;
#3869 = DIRECTION ( 'NONE',  ( 0.9510565162951536422, 0.000000000000000000, -0.3090169943749475623 ) ) ;
#3870 = PLANE ( 'NONE',  #5051 ) ;
#3871 = DIRECTION ( 'NONE',  ( -2.698458740408365879E-16, 1.000000000000000000, 0.000000000000000000 ) ) ;
#3872 = CIRCLE ( 'NONE', #20913, 2.928571428571432378 ) ;
#3873 = DIRECTION ( 'NONE',  ( -1.110223024625156540E-16, 0.000000000000000000, -1.000000000000000000 ) ) ;
#3874 = FACE_OUTER_BOUND ( 'NONE', #25916, .T. ) ;
#3875 = CARTESIAN_POINT ( 'NONE',  ( 11.46306169112780537, 8.437560028716553973, -17.10890052424691632 ) ) ;
#3876 = CARTESIAN_POINT ( 'NONE',  ( 12.50162201464318557, 8.571418981294288031, -15.12888223836978341 ) ) ;
#3877 = AXIS2_PLACEMENT_3D ( 'NONE', #9701, #23304, #4679 ) ;
#3878 = CARTESIAN_POINT ( 'NONE',  ( 146.4575131106458912, -10.00000000000000178, -17.99999999999998934 ) ) ;
#3879 = EDGE_LOOP ( 'NONE', ( #12280, #21299, #25060, #4877, #29548 ) ) ;
#3880 = CARTESIAN_POINT ( 'NONE',  ( 76.21670420379477662, -4.999999999999996447, 55.37467694846187527 ) ) ;
#3881 = DIRECTION ( 'NONE',  ( -2.698458740408365879E-16, 1.000000000000000000, 0.000000000000000000 ) ) ;
#3882 = VERTEX_POINT ( 'NONE', #11301 ) ;
#3883 = DIRECTION ( 'NONE',  ( 0.000000000000000000, 0.000000000000000000, 1.000000000000000000 ) ) ;
#3884 = CARTESIAN_POINT ( 'NONE',  ( 172.7287565553229740, -84.33034373659253902, -41.50000000000000711 ) ) ;
#3885 = LINE ( 'NONE', #12573, #18048 ) ;
#3887 = ORIENTED_EDGE ( 'NONE', *, *, #27588, .F. ) ;
#3886 = CARTESIAN_POINT ( 'NONE',  ( 25.04992766293576878, -3.547109489677171101, -13.67097983722207033 ) ) ;
#3888 = ORIENTED_EDGE ( 'NONE', *, *, #11210, .F. ) ;
#3889 = LINE ( 'NONE', #1755, #22253 ) ;
#3890 = CARTESIAN_POINT ( 'NONE',  ( 12.24710219714225268, 9.516853694884586545, -15.33174803936941366 ) ) ;
#3891 = DIRECTION ( 'NONE',  ( 0.5877852522924731371, 0.000000000000000000, 0.8090169943749474513 ) ) ;
#3892 = DIRECTION ( 'NONE',  ( 1.000000000000000000, 0.000000000000000000, 0.000000000000000000 ) ) ;
#3893 = VERTEX_POINT ( 'NONE', #17856 ) ;
#3894 = CARTESIAN_POINT ( 'NONE',  ( 25.04068920418659161, -5.475481712173364990, -18.92835678451453774 ) ) ;
#3895 = DIRECTION ( 'NONE',  ( -2.698458740408365879E-16, 1.000000000000000000, 0.000000000000000000 ) ) ;
#3896 = CARTESIAN_POINT ( 'NONE',  ( 22.92155253933561809, -3.178009374129639131, -14.34666800710537693 ) ) ;
#3897 = ORIENTED_EDGE ( 'NONE', *, *, #28842, .T. ) ;
#3898 = ADVANCED_FACE ( 'NONE', ( #24598 ), #20604, .T. ) ;
#3899 = CARTESIAN_POINT ( 'NONE',  ( 176.1922820468852535, -9.999999999999994671, -4.936203717676158398 ) ) ;
#3900 = AXIS2_PLACEMENT_3D ( 'NONE', #6246, #8521, #17823 ) ;
#3901 = CARTESIAN_POINT ( 'NONE',  ( 16.06097560829885040, 7.604535090956617616, -20.76572858943923094 ) ) ;
#3902 = CARTESIAN_POINT ( 'NONE',  ( 27.27607810006200140, -2.061267822988343656, -14.60586277656102006 ) ) ;
#3903 = VECTOR ( 'NONE', #6573, 1000.000000000000000 ) ;
#3904 = ORIENTED_EDGE ( 'NONE', *, *, #11114, .T. ) ;
#3905 = CARTESIAN_POINT ( 'NONE',  ( 29.88803641097454999, -7.968445601786871002, -16.75847372370488131 ) ) ;
#3906 = CARTESIAN_POINT ( 'NONE',  ( 154.7287565553229172, -4.999999999999976019, -16.50000000000000000 ) ) ;
#3907 = ORIENTED_EDGE ( 'NONE', *, *, #25658, .T. ) ;
#3908 = LINE ( 'NONE', #22979, #11680 ) ;
#3909 = LINE ( 'NONE', #4504, #23804 ) ;
#3910 = DIRECTION ( 'NONE',  ( -0.9510565162951536422, -2.566386769018988816E-16, -0.3090169943749472292 ) ) ;
#3911 = CARTESIAN_POINT ( 'NONE',  ( 7.345652830558766055, -4.996589667937400669, -0.4964154566688059877 ) ) ;
#3912 =( GEOMETRIC_REPRESENTATION_CONTEXT ( 3 ) GLOBAL_UNCERTAINTY_ASSIGNED_CONTEXT ( ( #6760 ) ) GLOBAL_UNIT_ASSIGNED_CONTEXT ( ( #22024, #19422, #10411 ) ) REPRESENTATION_CONTEXT ( 'NONE', 'WORKASPACE' ) );
#3913 = CARTESIAN_POINT ( 'NONE',  ( 25.04433344647707571, -4.420048373160954114, -18.22226412361657921 ) ) ;
#3914 = CARTESIAN_POINT ( 'NONE',  ( 19.30972751531945519, 5.994221256738944348, -19.84686166629000326 ) ) ;
#3915 = EDGE_CURVE ( 'NONE', #20048, #2560, #27070, .T. ) ;
#3916 = CARTESIAN_POINT ( 'NONE',  ( 34.26516872548082659, -12.92629604573065549, -20.94206068969455004 ) ) ;
#3918 = LINE ( 'NONE', #3615, #18302 ) ;
#3917 = VECTOR ( 'NONE', #16976, 1000.000000000000000 ) ;
#3919 = CARTESIAN_POINT ( 'NONE',  ( 11.47288049726737214, 9.269262779257836371, -15.86091052746238184 ) ) ;
#3920 = VECTOR ( 'NONE', #13647, 1000.000000000000000 ) ;
#3921 = DIRECTION ( 'NONE',  ( -0.000000000000000000, -0.000000000000000000, 1.000000000000000000 ) ) ;
#3922 = CARTESIAN_POINT ( 'NONE',  ( 141.1922820468854525, -10.00000000000000533, -19.40354224447947473 ) ) ;
#3923 = CARTESIAN_POINT ( 'NONE',  ( 13.12278719711289732, 8.570488965836000617, -15.91256645732111430 ) ) ;
#3924 = CARTESIAN_POINT ( 'NONE',  ( -4.683753385137379155E-14, -9.237604307034027684, -4.285468820183664818 ) ) ;
#3925 = CARTESIAN_POINT ( 'NONE',  ( 137.0152310637605808, -4.999999999999980460, -1.521174642513229767E-14 ) ) ;
#3926 = CARTESIAN_POINT ( 'NONE',  ( 11.47338783222600789, 9.266948822715743717, -15.86069975447064806 ) ) ;
#3927 = ORIENTED_EDGE ( 'NONE', *, *, #18941, .T. ) ;
#3928 = FACE_OUTER_BOUND ( 'NONE', #13646, .T. ) ;
#3929 = LINE ( 'NONE', #25134, #22475 ) ;
#3930 = LINE ( 'NONE', #11087, #7824 ) ;
#3931 = VERTEX_POINT ( 'NONE', #5977 ) ;
#3932 = CARTESIAN_POINT ( 'NONE',  ( 8.944914148442956403, 16.95008179206086396, -17.86239244656949765 ) ) ;
#3934 = AXIS2_PLACEMENT_3D ( 'NONE', #11544, #581, #25760 ) ;
#3933 = CARTESIAN_POINT ( 'NONE',  ( 31.96909791962396596, -10.29830001063286460, -18.46063605759182735 ) ) ;
#3935 = CARTESIAN_POINT ( 'NONE',  ( 18.76228799092704236, 0.4007544294800896578, -19.29634928253052806 ) ) ;
#3936 = VECTOR ( 'NONE', #6769, 1000.000000000000000 ) ;
#3937 = CARTESIAN_POINT ( 'NONE',  ( 27.61484239614359737, -11.78684095324212855, -18.66559939683001446 ) ) ;
#3938 = DIRECTION ( 'NONE',  ( -1.000000000000000000, -4.440892098500622217E-16, 0.000000000000000000 ) ) ;
#3939 = FACE_OUTER_BOUND ( 'NONE', #21966, .T. ) ;
#3940 = DIRECTION ( 'NONE',  ( 0.000000000000000000, 0.000000000000000000, 1.000000000000000000 ) ) ;
#3941 = CARTESIAN_POINT ( 'NONE',  ( 18.31666763169264911, 2.112308299563359970, -18.35152529819803746 ) ) ;
#3942 =( GEOMETRIC_REPRESENTATION_CONTEXT ( 3 ) GLOBAL_UNCERTAINTY_ASSIGNED_CONTEXT ( ( #30012 ) ) GLOBAL_UNIT_ASSIGNED_CONTEXT ( ( #3163, #10603, #21756 ) ) REPRESENTATION_CONTEXT ( 'NONE', 'WORKASPACE' ) );
#3943 = ORIENTED_EDGE ( 'NONE', *, *, #23889, .F. ) ;
#3944 = DIRECTION ( 'NONE',  ( 0.9510565162951536422, 2.566386769018988816E-16, 0.3090169943749472292 ) ) ;
#3945 = ORIENTED_EDGE ( 'NONE', *, *, #12796, .F. ) ;
#3947 = ORIENTED_EDGE ( 'NONE', *, *, #10935, .F. ) ;
#3946 = CYLINDRICAL_SURFACE ( 'NONE', #2429, 4.000000000000000000 ) ;
#3948 = CARTESIAN_POINT ( 'NONE',  ( 175.7287565553229456, -9.999999999999971578, 3.500000000000003109 ) ) ;
#3949 = VECTOR ( 'NONE', #4963, 1000.000000000000000 ) ;
#3950 = CARTESIAN_POINT ( 'NONE',  ( 12.03842576178837298, 9.272001309349649389, -16.68677036593512497 ) ) ;
#3951 = EDGE_CURVE ( 'NONE', #438, #24310, #6435, .T. ) ;
#3952 = EDGE_CURVE ( 'NONE', #18704, #6853, #3843, .T. ) ;
#3953 = CARTESIAN_POINT ( 'NONE',  ( 35.54859390953723164, -21.18451583373416014, -14.99999999999999822 ) ) ;
#3954 = EDGE_LOOP ( 'NONE', ( #24631, #30157, #16632, #3485, #1097 ) ) ;
#3955 = VECTOR ( 'NONE', #24601, 1000.000000000000000 ) ;
#3956 = CARTESIAN_POINT ( 'NONE',  ( 10.66984875114861886, 9.039338215604900029, -16.41071671300888823 ) ) ;
#3957 = EDGE_CURVE ( 'NONE', #6726, #16400, #13435, .T. ) ;
#3958 = EDGE_CURVE ( 'NONE', #26594, #27211, #25055, .T. ) ;
#3959 = CARTESIAN_POINT ( 'NONE',  ( 27.20760296572909809, -8.488227175050779394, -13.35743234967312354 ) ) ;
#3960 = CARTESIAN_POINT ( 'NONE',  ( 12.93646321750111916, 9.546177831575306527, -16.06107003375496944 ) ) ;
#3961 = FACE_BOUND ( 'NONE', #43, .T. ) ;
#3962 = ORIENTED_EDGE ( 'NONE', *, *, #16480, .T. ) ;
#3963 = STYLED_ITEM ( 'NONE', ( #14685 ), #17465 ) ;
#3964 = VERTEX_POINT ( 'NONE', #22764 ) ;
#3965 = DIRECTION ( 'NONE',  ( 0.000000000000000000, 0.000000000000000000, 1.000000000000000000 ) ) ;
#3966 = CARTESIAN_POINT ( 'NONE',  ( 12.50481220565295004, 8.572828783776230921, -15.12633959982445653 ) ) ;
#3967 = CARTESIAN_POINT ( 'NONE',  ( 147.0152310637605808, -4.999999999999977796, -15.61832212156129707 ) ) ;
#3968 = FACE_OUTER_BOUND ( 'NONE', #10680, .T. ) ;
#3969 = ORIENTED_EDGE ( 'NONE', *, *, #6710, .T. ) ;
#3970 = CARTESIAN_POINT ( 'NONE',  ( 13.25994536507779742, 8.631100619704961119, -15.80324905228922994 ) ) ;
#3971 = CARTESIAN_POINT ( 'NONE',  ( 20.85347709306256547, 5.504344946561741558, -13.72608531385973407 ) ) ;
#3972 = CARTESIAN_POINT ( 'NONE',  ( 18.68383238644686273, 8.832144196210188980, -14.76942027321762119 ) ) ;
#3973 = DIRECTION ( 'NONE',  ( 0.000000000000000000, 0.000000000000000000, 1.000000000000000000 ) ) ;
#3974 = CARTESIAN_POINT ( 'NONE',  ( 137.0152310637605808, -10.00000000000000533, -34.70218595412750773 ) ) ;
#3975 = VECTOR ( 'NONE', #9218, 1000.000000000000000 ) ;
#3976 = AXIS2_PLACEMENT_3D ( 'NONE', #27570, #13480, #29741 ) ;
#3977 = CARTESIAN_POINT ( 'NONE',  ( 18.80472905218952917, 2.352968372735388503, -20.19605574946481497 ) ) ;
#3978 = DIRECTION ( 'NONE',  ( -0.000000000000000000, -0.000000000000000000, 1.000000000000000000 ) ) ;
#3979 = CARTESIAN_POINT ( 'NONE',  ( 167.0152310637604387, -9.999999999999998224, -8.721423840594312082 ) ) ;
#3980 = ORIENTED_EDGE ( 'NONE', *, *, #19480, .F. ) ;
#3981 = CARTESIAN_POINT ( 'NONE',  ( 171.1922820468853672, -1.999999999999970912, -28.06379628232387446 ) ) ;
#3982 = EDGE_CURVE ( 'NONE', #11963, #12041, #13292, .T. ) ;
#3983 = CARTESIAN_POINT ( 'NONE',  ( 34.96805304670973413, -19.57645325810014114, -20.18246498508359466 ) ) ;
#3984 = CARTESIAN_POINT ( 'NONE',  ( 152.2287565553229456, -10.00000000000000178, -3.509618943233403510 ) ) ;
#3985 = VERTEX_POINT ( 'NONE', #10993 ) ;
#3986 = ADVANCED_FACE ( 'NONE', ( #22303 ), #15573, .F. ) ;
#3987 = EDGE_CURVE ( 'NONE', #8714, #30251, #13558, .T. ) ;
#3988 = CARTESIAN_POINT ( 'NONE',  ( 144.5152310637605524, -10.00000000000000355, -13.05155085951651195 ) ) ;
#3989 = EDGE_CURVE ( 'NONE', #13765, #14128, #27497, .T. ) ;
#3990 = CARTESIAN_POINT ( 'NONE',  ( 11.05541531668977662, 17.68942339022145305, -17.91796598306941135 ) ) ;
#3991 = CARTESIAN_POINT ( 'NONE',  ( -11.85189716074912880, -5.341585316273318895, 4.999999999999998224 ) ) ;
#3992 = ORIENTED_EDGE ( 'NONE', *, *, #24358, .T. ) ;
#3993 = DIRECTION ( 'NONE',  ( -2.698458740408365879E-16, 1.000000000000000000, 0.000000000000000000 ) ) ;
#3994 = CARTESIAN_POINT ( 'NONE',  ( 9.641351021852148762, 17.66889017177091503, -17.91406276888456617 ) ) ;
#3995 = DIRECTION ( 'NONE',  ( -6.938893903907227392E-16, 0.000000000000000000, -1.000000000000000000 ) ) ;
#3996 = DIRECTION ( 'NONE',  ( 2.698458740408365879E-16, -1.000000000000000000, 0.000000000000000000 ) ) ;
#3997 = VERTEX_POINT ( 'NONE', #20868 ) ;
#3998 = DIRECTION ( 'NONE',  ( -0.9510565162951536422, -2.566386769018988816E-16, -0.3090169943749472292 ) ) ;
#3999 = ORIENTED_EDGE ( 'NONE', *, *, #2447, .F. ) ;
#4000 = CARTESIAN_POINT ( 'NONE',  ( 10.35864918915110877, 16.97212501191939538, -17.91664992932186351 ) ) ;
#4001 = CARTESIAN_POINT ( 'NONE',  ( 35.48977118337261771, -17.42778619908077076, -20.26990708652652629 ) ) ;
#4002 = CARTESIAN_POINT ( 'NONE',  ( 21.42923412144385509, -1.598955984811285536, -13.33006947543598741 ) ) ;
#4003 = VECTOR ( 'NONE', #1281, 1000.000000000000000 ) ;
#4004 = DIRECTION ( 'NONE',  ( 0.000000000000000000, 0.000000000000000000, 1.000000000000000000 ) ) ;
#4005 = DIRECTION ( 'NONE',  ( -0.5877852522924731371, 0.000000000000000000, 0.8090169943749474513 ) ) ;
#4006 = DIRECTION ( 'NONE',  ( -2.698458740408365879E-16, 1.000000000000000000, 0.000000000000000000 ) ) ;
#4007 = SURFACE_STYLE_FILL_AREA ( #8425 ) ;
#4008 = CARTESIAN_POINT ( 'NONE',  ( 30.58006126958193249, -8.114715823802763239, -15.12008790671442426 ) ) ;
#4009 = CARTESIAN_POINT ( 'NONE',  ( 27.81650010061016332, -6.490163795910067535, -14.16582606047713178 ) ) ;
#4010 = VECTOR ( 'NONE', #20726, 1000.000000000000000 ) ;
#4011 = VERTEX_POINT ( 'NONE', #27352 ) ;
#4012 = LINE ( 'NONE', #13756, #9851 ) ;
#4013 = DIRECTION ( 'NONE',  ( -0.8090169943749474513, -2.183098979609982436E-16, -0.5877852522924731371 ) ) ;
#4014 = DIRECTION ( 'NONE',  ( -2.698458740408365879E-16, 1.000000000000000000, 0.000000000000000000 ) ) ;
#4015 = CARTESIAN_POINT ( 'NONE',  ( 166.1922820468853388, -9.999999999999998224, -13.59645775552055902 ) ) ;
#4016 = CARTESIAN_POINT ( 'NONE',  ( 131.1922820468854241, -10.00000000000000888, -10.74328820663507322 ) ) ;
#4017 = VECTOR ( 'NONE', #29712, 1000.000000000000000 ) ;
#4018 = ADVANCED_FACE ( 'NONE', ( #17828 ), #16158, .F. ) ;
#4019 = CARTESIAN_POINT ( 'NONE',  ( 159.5152310637604387, -1.999999999999974021, -4.391296821672111328 ) ) ;
#4020 = CARTESIAN_POINT ( 'NONE',  ( 11.22637516657937162, 9.079975409179585455, -17.24057027585384105 ) ) ;
#4021 = EDGE_CURVE ( 'NONE', #28630, #14061, #9112, .T. ) ;
#4022 = EDGE_CURVE ( 'NONE', #29656, #2898, #29959, .T. ) ;
#4023 = CARTESIAN_POINT ( 'NONE',  ( 12.71834232392635045, 8.667191563245470576, -14.95615232649864090 ) ) ;
#4024 = ADVANCED_FACE ( 'NONE', ( #24878 ), #16148, .F. ) ;
#4025 = CARTESIAN_POINT ( 'NONE',  ( 30.78125299044525320, -8.317598597646391312, -16.28273480984023891 ) ) ;
#4026 = PLANE ( 'NONE',  #9054 ) ;
#4027 = CARTESIAN_POINT ( 'NONE',  ( -20.00000000000017053, 34.64101615137744972, 0.000000000000000000 ) ) ;
#4028 = ORIENTED_EDGE ( 'NONE', *, *, #21000, .F. ) ;
#4029 = CARTESIAN_POINT ( 'NONE',  ( 9.641350810849047548, 17.66889113945805789, -21.33333333332589277 ) ) ;
#4031 = CARTESIAN_POINT ( 'NONE',  ( 158.6922820468853672, -1.999999999999974021, -17.92658477444275889 ) ) ;
#4030 = VECTOR ( 'NONE', #3049, 1000.000000000000000 ) ;
#4032 = LINE ( 'NONE', #27272, #19022 ) ;
#4033 = CARTESIAN_POINT ( 'NONE',  ( 171.1922820468853104, -1.999999999999970912, -10.74328820663507678 ) ) ;
#4035 = ORIENTED_EDGE ( 'NONE', *, *, #1035, .T. ) ;
#4034 = CARTESIAN_POINT ( 'NONE',  ( 22.34083945069921739, -4.755659482961629436, -14.12236044035638116 ) ) ;
#4036 = ORIENTED_EDGE ( 'NONE', *, *, #18299, .F. ) ;
#4037 = LINE ( 'NONE', #25394, #14432 ) ;
#4038 = CARTESIAN_POINT ( 'NONE',  ( 12.68070129083326236, 9.708587077508630259, -14.98615289428795094 ) ) ;
#4039 = CARTESIAN_POINT ( 'NONE',  ( 33.15992091288699584, -11.77879734164826786, -17.82291275646110407 ) ) ;
#4040 = FACE_OUTER_BOUND ( 'NONE', #26078, .T. ) ;
#4041 = CARTESIAN_POINT ( 'NONE',  ( 26.47511176763426377, -7.718147522161595830, -18.64721581247919602 ) ) ;
#4042 = CARTESIAN_POINT ( 'NONE',  ( 159.7287565553229172, -10.00000000000000000, -7.839745962155603820 ) ) ;
#4043 = CARTESIAN_POINT ( 'NONE',  ( 20.36893440901172170, -1.919154233093003814, -17.42624063329192552 ) ) ;
#4044 = ORIENTED_EDGE ( 'NONE', *, *, #21385, .F. ) ;
#4045 = LINE ( 'NONE', #1768, #2767 ) ;
#4046 =( NAMED_UNIT ( * ) SI_UNIT ( $, .STERADIAN. ) SOLID_ANGLE_UNIT ( ) );
#4047 = CARTESIAN_POINT ( 'NONE',  ( 13.86827785273622737, 5.312354197023893221, -16.63408457058017120 ) ) ;
#4048 = VECTOR ( 'NONE', #3051, 1000.000000000000000 ) ;
#4049 = CARTESIAN_POINT ( 'NONE',  ( 29.48152472672500579, -5.877396966218813468, -15.70213184580788379 ) ) ;
#4050 =( REPRESENTATION_RELATIONSHIP ('NONE','NONE', #5250, #18708 ) REPRESENTATION_RELATIONSHIP_WITH_TRANSFORMATION ( #5663 )SHAPE_REPRESENTATION_RELATIONSHIP( ) );
#4051 = EDGE_LOOP ( 'NONE', ( #25843, #9045, #24810, #16363 ) ) ;
#4052 = EDGE_LOOP ( 'NONE', ( #28141, #29867, #12630, #29986 ) ) ;
#4053 = CARTESIAN_POINT ( 'NONE',  ( 25.97851742199650005, -11.98992670343847244, -16.97112261376066655 ) ) ;
#4054 = VECTOR ( 'NONE', #3944, 1000.000000000000000 ) ;
#4055 = CARTESIAN_POINT ( 'NONE',  ( 131.1922820468854241, -1.999999999999981348, -28.06379628232387446 ) ) ;
#4056 = ORIENTED_EDGE ( 'NONE', *, *, #8991, .T. ) ;
#4057 = CARTESIAN_POINT ( 'NONE',  ( 162.0152310637605524, -1.999999999999971800, -32.93883019725009120 ) ) ;
#4058 = CARTESIAN_POINT ( 'NONE',  ( 174.5152310637604671, -4.999999999999970690, -30.37205893520531319 ) ) ;
#4059 = EDGE_CURVE ( 'NONE', #6652, #10981, #11553, .T. ) ;
#4060 = DIRECTION ( 'NONE',  ( 0.000000000000000000, 0.000000000000000000, -1.000000000000000000 ) ) ;
#4061 = ADVANCED_FACE ( 'NONE', ( #8526 ), #27197, .T. ) ;
#4062 = CARTESIAN_POINT ( 'NONE',  ( 9.641350810849047548, 17.66889113945805789, -17.97192418671891190 ) ) ;
#4063 = EDGE_CURVE ( 'NONE', #17748, #21455, #20471, .T. ) ;
#4064 = CARTESIAN_POINT ( 'NONE',  ( 25.84319962709097140, -7.021413190281159622, -18.98986798778381058 ) ) ;
#4065 = CARTESIAN_POINT ( 'NONE',  ( 18.12654306171327079, 0.8625984663607378922, -18.09208126113620452 ) ) ;
#4066 = CARTESIAN_POINT ( 'NONE',  ( 35.12112610261377910, -16.77165912796762726, -21.20079607051596327 ) ) ;
#4067 = LINE ( 'NONE', #13360, #11957 ) ;
#4068 = CARTESIAN_POINT ( 'NONE',  ( 12.29195110325218288, 8.516770644378290456, -15.29309475950548958 ) ) ;
#4069 = DIRECTION ( 'NONE',  ( -1.000000000000000000, -4.440892098500622217E-16, 0.000000000000000000 ) ) ;
#4070 = LINE ( 'NONE', #4216, #11971 ) ;
#4071 = CARTESIAN_POINT ( 'NONE',  ( 13.13063628947021755, 8.573956625762026107, -15.90631066800904669 ) ) ;
#4072 = CARTESIAN_POINT ( 'NONE',  ( 134.5152310637605808, -1.999999999999980460, -2.627941064794695691 ) ) ;
#4073 = EDGE_LOOP ( 'NONE', ( #23882, #2122, #15313, #3161 ) ) ;
#4074 = DIRECTION ( 'NONE',  ( 0.000000000000000000, 0.000000000000000000, 1.000000000000000000 ) ) ;
#4075 = CARTESIAN_POINT ( 'NONE',  ( 12.37169234869624646, 8.529253869913038244, -15.23127513898213081 ) ) ;
#4076 = ORIENTED_EDGE ( 'NONE', *, *, #7569, .F. ) ;
#4077 = DIRECTION ( 'NONE',  ( 1.000000000000000000, 2.698458740408365879E-16, -1.110223024625156540E-16 ) ) ;
#4078 = DIRECTION ( 'NONE',  ( -2.698458740408365879E-16, 1.000000000000000000, 0.000000000000000000 ) ) ;
#4079 = DIRECTION ( 'NONE',  ( -2.698458740408365879E-16, 1.000000000000000000, 0.000000000000000000 ) ) ;
#4080 = VECTOR ( 'NONE', #26669, 1000.000000000000000 ) ;
#4081 = VERTEX_POINT ( 'NONE', #20423 ) ;
#4082 = ORIENTED_EDGE ( 'NONE', *, *, #26433, .T. ) ;
#4083 = CARTESIAN_POINT ( 'NONE',  ( 13.37957753592864663, 7.625938299336016968, -15.70790011242621453 ) ) ;
#4084 = CARTESIAN_POINT ( 'NONE',  ( 34.40782828833705054, -13.56718989277036691, -20.98518325316450372 ) ) ;
#4085 = CARTESIAN_POINT ( 'NONE',  ( 20.33560388840259137, 1.841519175196629998, -20.14887626749220217 ) ) ;
#4086 = CARTESIAN_POINT ( 'NONE',  ( 18.55323344277375242, 5.040171350539718098, -19.22783755317104237 ) ) ;
#4087 = LINE ( 'NONE', #29785, #6288 ) ;
#4088 = DIRECTION ( 'NONE',  ( 0.5877852522924731371, 1.586114251531760728E-16, -0.8090169943749474513 ) ) ;
#4089 = CARTESIAN_POINT ( 'NONE',  ( 22.85243615162648112, -7.655412890396200432, -19.01377894019457315 ) ) ;
#4090 = EDGE_CURVE ( 'NONE', #12211, #2375, #15838, .T. ) ;
#4091 = VECTOR ( 'NONE', #4105, 1000.000000000000000 ) ;
#4092 = EDGE_LOOP ( 'NONE', ( #27708, #21953, #17341, #22837, #17500 ) ) ;
#4093 = DIRECTION ( 'NONE',  ( 1.000000000000000000, 0.000000000000000000, -1.387778780781445676E-16 ) ) ;
#4095 = ORIENTED_EDGE ( 'NONE', *, *, #21581, .F. ) ;
#4094 = LINE ( 'NONE', #17808, #20438 ) ;
#4096 = CARTESIAN_POINT ( 'NONE',  ( 13.87499999999999822, -1.353986367469417343E-16, 4.756499999999999062 ) ) ;
#4097 = DIRECTION ( 'NONE',  ( -0.8090169943749474513, -2.183098979609982436E-16, -0.5877852522924731371 ) ) ;
#4098 = VECTOR ( 'NONE', #11393, 1000.000000000000000 ) ;
#4099 = ADVANCED_FACE ( 'NONE', ( #25768 ), #12165, .F. ) ;
#4100 = CARTESIAN_POINT ( 'NONE',  ( 164.5152310637604671, -9.999999999999998224, -13.05155085951651195 ) ) ;
#4101 = CARTESIAN_POINT ( 'NONE',  ( 35.26536834604049631, -19.91213340569504808, -19.23001471935974038 ) ) ;
#4102 = CARTESIAN_POINT ( 'NONE',  ( 10.66838568802538845, 9.046021620013140918, -16.41132375377494057 ) ) ;
#4103 = ORIENTED_EDGE ( 'NONE', *, *, #20033, .F. ) ;
#4104 = CARTESIAN_POINT ( 'NONE',  ( 29.76939623719675510, -8.219725197086590995, -17.35520659559267287 ) ) ;
#4105 = DIRECTION ( 'NONE',  ( 1.000000000000000000, 2.698458740408367851E-16, 0.000000000000000000 ) ) ;
#4106 = CARTESIAN_POINT ( 'NONE',  ( 10.35864927600819740, 16.97212461358170188, -17.91506874352199574 ) ) ;
#4107 = FACE_BOUND ( 'NONE', #26154, .T. ) ;
#4108 = ORIENTED_EDGE ( 'NONE', *, *, #13246, .T. ) ;
#4109 = VERTEX_POINT ( 'NONE', #16754 ) ;
#4110 = DIRECTION ( 'NONE',  ( -2.698458740408365879E-16, 1.000000000000000000, -0.000000000000000000 ) ) ;
#4111 = EDGE_LOOP ( 'NONE', ( #28436, #8671, #25897, #23439 ) ) ;
#4112 = DIRECTION ( 'NONE',  ( -0.000000000000000000, -0.000000000000000000, 1.000000000000000000 ) ) ;
#4113 = CARTESIAN_POINT ( 'NONE',  ( -8.000000000000000000, 4.618802153517001408, -5.000000000000000888 ) ) ;
#4114 = PLANE ( 'NONE',  #7657 ) ;
#4115 = ORIENTED_EDGE ( 'NONE', *, *, #7121, .T. ) ;
#4116 = CARTESIAN_POINT ( 'NONE',  ( 13.14084490070201738, 8.578467993704791184, -15.89817422466314945 ) ) ;
#4117 = VERTEX_POINT ( 'NONE', #23627 ) ;
#4118 = CARTESIAN_POINT ( 'NONE',  ( 22.03599841643320190, -0.8527435389730096960, -19.82300248246997398 ) ) ;
#4119 = CARTESIAN_POINT ( 'NONE',  ( 17.94761415789183445, 0.5003475314714088684, -19.87472444338139965 ) ) ;
#4120 = DIRECTION ( 'NONE',  ( 0.000000000000000000, 0.000000000000000000, 1.000000000000000000 ) ) ;
#4121 = AXIS2_PLACEMENT_3D ( 'NONE', #6841, #420, #13692 ) ;
#4122 = CARTESIAN_POINT ( 'NONE',  ( -6.689127551062014732, -5.375634714784644608, -0.3173508448886681044 ) ) ;
#4123 = EDGE_CURVE ( 'NONE', #28074, #22328, #26077, .T. ) ;
#4124 = EDGE_CURVE ( 'NONE', #9369, #3213, #284, .T. ) ;
#4125 = CARTESIAN_POINT ( 'NONE',  ( 21.40051611374530793, -0.1690565882708310874, -20.18282279970310000 ) ) ;
#4126 = ORIENTED_EDGE ( 'NONE', *, *, #16829, .T. ) ;
#4127 = VECTOR ( 'NONE', #4619, 1000.000000000000000 ) ;
#4128 = LINE ( 'NONE', #17840, #13960 ) ;
#4129 = LINE ( 'NONE', #25188, #18150 ) ;
#4130 = ORIENTED_EDGE ( 'NONE', *, *, #10025, .F. ) ;
#4131 = CARTESIAN_POINT ( 'NONE',  ( 10.47008273352651564, 16.46107657294071203, -17.33567129194344858 ) ) ;
#4132 = CARTESIAN_POINT ( 'NONE',  ( 33.33926371295168423, -12.28475995124076903, -19.67523791759492013 ) ) ;
#4133 = LINE ( 'NONE', #29978, #16048 ) ;
#4134 = ORIENTED_EDGE ( 'NONE', *, *, #11212, .T. ) ;
#4135 = VERTEX_POINT ( 'NONE', #27942 ) ;
#4136 = LINE ( 'NONE', #9, #13405 ) ;
#4137 = VECTOR ( 'NONE', #1595, 1000.000000000000000 ) ;
#4138 = CARTESIAN_POINT ( 'NONE',  ( 14.34656430690936624, 9.113120221615268690, -15.03016663717492563 ) ) ;
#4139 = CARTESIAN_POINT ( 'NONE',  ( 12.24596961785936777, 9.516471373605908113, -15.33264171117454744 ) ) ;
#4140 = CARTESIAN_POINT ( 'NONE',  ( 133.6922820468854241, -4.999999999999982236, -32.39392330124607611 ) ) ;
#4141 = VERTEX_POINT ( 'NONE', #9874 ) ;
#4142 = CARTESIAN_POINT ( 'NONE',  ( 9.641350810849047548, 17.66889113945805789, -17.95086732675817132 ) ) ;
#4143 = CARTESIAN_POINT ( 'NONE',  ( 13.30044262271030142, 7.866402339252101861, -14.49220811360527605 ) ) ;
#4144 = DIRECTION ( 'NONE',  ( -0.8090169943749474513, -2.183098979609982436E-16, -0.5877852522924731371 ) ) ;
#4145 = ORIENTED_EDGE ( 'NONE', *, *, #1240, .F. ) ;
#4146 = DIRECTION ( 'NONE',  ( -0.5877852522924731371, -1.586114251531760728E-16, -0.8090169943749474513 ) ) ;
#4147 = ORIENTED_EDGE ( 'NONE', *, *, #14357, .F. ) ;
#4148 = CARTESIAN_POINT ( 'NONE',  ( 10.35864953657871190, 16.97212341857210660, -17.91436492910080247 ) ) ;
#4149 = CARTESIAN_POINT ( 'NONE',  ( 34.21937970685856101, -11.80343312934236089, -19.83772509046166732 ) ) ;
#4150 = CARTESIAN_POINT ( 'NONE',  ( 25.57370974413349884, -0.4222200280313516685, -16.88676729435558599 ) ) ;
#4151 = VERTEX_POINT ( 'NONE', #21173 ) ;
#4152 = DIRECTION ( 'NONE',  ( 0.000000000000000000, 0.000000000000000000, -1.000000000000000000 ) ) ;
#4153 = DIRECTION ( 'NONE',  ( 1.000000000000000000, 2.698458740408365879E-16, 0.000000000000000000 ) ) ;
#4154 = EDGE_CURVE ( 'NONE', #28443, #2968, #2434, .T. ) ;
#4155 = CARTESIAN_POINT ( 'NONE',  ( 28.40444427461093113, -11.06999723682266179, -18.98653349803348078 ) ) ;
#4156 = EDGE_CURVE ( 'NONE', #280, #619, #132, .T. ) ;
#4157 = CARTESIAN_POINT ( 'NONE',  ( 27.79171034377997884, -3.119812929724471662, -15.83729198868751276 ) ) ;
#4158 = CONICAL_SURFACE ( 'NONE', #26103, 4.513000000000000789, 0.2131563744996338439 ) ;
#4159 = VERTEX_POINT ( 'NONE', #13991 ) ;
#4160 = EDGE_CURVE ( 'NONE', #13649, #22275, #16289, .T. ) ;
#4161 = EDGE_LOOP ( 'NONE', ( #2882, #13992, #391, #6242, #6168 ) ) ;
#4162 = ORIENTED_EDGE ( 'NONE', *, *, #15722, .T. ) ;
#4163 = CARTESIAN_POINT ( 'NONE',  ( 25.15155720165195063, -5.000000000000010658, -77.40853353384594016 ) ) ;
#4164 = LINE ( 'NONE', #13458, #6693 ) ;
#4165 = CARTESIAN_POINT ( 'NONE',  ( 166.1922820468853672, -1.999999999999971356, -19.40354224447947828 ) ) ;
#4166 = CARTESIAN_POINT ( 'NONE',  ( 144.7287565553230309, -10.00000000000000355, -16.50000000000000355 ) ) ;
#4167 = CARTESIAN_POINT ( 'NONE',  ( 12.50396148805030627, 8.572452836447732594, -15.12701763676990119 ) ) ;
#4168 = CARTESIAN_POINT ( 'NONE',  ( 142.0152310637605524, -4.999999999999979572, -8.721423840594312082 ) ) ;
#4169 = ORIENTED_EDGE ( 'NONE', *, *, #15331, .T. ) ;
#4170 = CARTESIAN_POINT ( 'NONE',  ( 168.6922820468853388, -1.999999999999971356, -17.92658477444275889 ) ) ;
#4171 = VERTEX_POINT ( 'NONE', #588 ) ;
#4172 = AXIS2_PLACEMENT_3D ( 'NONE', #2646, #9640, #18661 ) ;
#4173 = CARTESIAN_POINT ( 'NONE',  ( 9.641350810849047548, 17.66889113945805789, -17.91664992932186351 ) ) ;
#4174 = VECTOR ( 'NONE', #22383, 1000.000000000000000 ) ;
#4175 = FACE_OUTER_BOUND ( 'NONE', #1570, .T. ) ;
#4176 = CARTESIAN_POINT ( 'NONE',  ( 17.68287507214707688, 6.939063861736925354, -15.39301800483504934 ) ) ;
#4177 = DIRECTION ( 'NONE',  ( -1.110223024625156540E-16, 0.000000000000000000, -1.000000000000000000 ) ) ;
#4178 = DIRECTION ( 'NONE',  ( 0.5877852522924731371, 1.586114251531760728E-16, -0.8090169943749474513 ) ) ;
#4180 = ORIENTED_EDGE ( 'NONE', *, *, #14324, .F. ) ;
#4179 = CARTESIAN_POINT ( 'NONE',  ( 23.63863231746517712, -2.790269051896475450, -19.68844555248840678 ) ) ;
#4181 = ORIENTED_EDGE ( 'NONE', *, *, #7200, .T. ) ;
#4182 = DIRECTION ( 'NONE',  ( -2.698458740408365879E-16, 1.000000000000000000, 0.000000000000000000 ) ) ;
#4183 = CARTESIAN_POINT ( 'NONE',  ( 12.24523086077475220, 9.516144614896692389, -15.33323053563244898 ) ) ;
#4184 = ADVANCED_FACE ( 'NONE', ( #11711 ), #18889, .F. ) ;
#4185 = CARTESIAN_POINT ( 'NONE',  ( 35.54859390953724585, -22.18451583373416014, -18.19919658220850778 ) ) ;
#4186 = LINE ( 'NONE', #6029, #12235 ) ;
#4187 = EDGE_LOOP ( 'NONE', ( #4230, #10530, #26158, #23284 ) ) ;
#4188 = CARTESIAN_POINT ( 'NONE',  ( 25.26806593431409453, -8.821542497490490575, -18.05414547114721557 ) ) ;
#4189 = CARTESIAN_POINT ( 'NONE',  ( 136.1922820468854241, -1.999999999999980460, -22.25671179336495697 ) ) ;
#4190 = CARTESIAN_POINT ( 'NONE',  ( 25.50636554463319072, -2.203555497659483553, -15.54816553724606187 ) ) ;
#4191 = ORIENTED_EDGE ( 'NONE', *, *, #13246, .F. ) ;
#4192 = FACE_OUTER_BOUND ( 'NONE', #20337, .T. ) ;
#4193 = CARTESIAN_POINT ( 'NONE',  ( 18.04976943019953239, 10.79320383120880145, -15.74583687248850161 ) ) ;
#4194 = CARTESIAN_POINT ( 'NONE',  ( 27.61097550864939265, -12.05054904645494673, -17.30446993171443637 ) ) ;
#4195 = ADVANCED_FACE ( 'NONE', ( #7594 ), #21029, .T. ) ;
#4196 = TOROIDAL_SURFACE ( 'NONE', #5144, 7.000000000000000888, 2.000000000000000000 ) ;
#4197 = ADVANCED_FACE ( 'NONE', ( #4698 ), #13680, .T. ) ;
#4198 = EDGE_CURVE ( 'NONE', #6890, #11977, #25924, .T. ) ;
#4199 = ADVANCED_FACE ( 'NONE', ( #28398 ), #26230, .T. ) ;
#4200 = ORIENTED_EDGE ( 'NONE', *, *, #9236, .F. ) ;
#4201 = CARTESIAN_POINT ( 'NONE',  ( -3.673643420401920601, -2.497823135841290565, -2.201519936624986240 ) ) ;
#4202 = AXIS2_PLACEMENT_3D ( 'NONE', #23588, #21139, #7263 ) ;
#4203 = AXIS2_PLACEMENT_3D ( 'NONE', #2838, #999, #3292 ) ;
#4204 = DIRECTION ( 'NONE',  ( 0.3090169943749472292, 8.338696094057992503E-17, -0.9510565162951536422 ) ) ;
#4205 = LINE ( 'NONE', #8327, #1471 ) ;
#4206 = LINE ( 'NONE', #25115, #6747 ) ;
#4207 = LINE ( 'NONE', #27445, #27547 ) ;
#4208 = CARTESIAN_POINT ( 'NONE',  ( 9.641350810849047548, 17.66889113945805789, -17.92454625180715766 ) ) ;
#4209 = CARTESIAN_POINT ( 'NONE',  ( 24.63339645208565543, -5.721020077635508905, -14.05062826560360278 ) ) ;
#4210 = CARTESIAN_POINT ( 'NONE',  ( 18.16551323082808267, 7.152368624112494189, -14.07085781252208712 ) ) ;
#4211 = CARTESIAN_POINT ( 'NONE',  ( 32.54894808986480115, -9.611255921941241454, -17.86757894403779900 ) ) ;
#4212 = CARTESIAN_POINT ( 'NONE',  ( 1.321505333908962632, -3.855830693249187480, -0.03421028094655551716 ) ) ;
#4213 = CARTESIAN_POINT ( 'NONE',  ( 11.48249212886396897, 9.228508165798535501, -15.85668214399537845 ) ) ;
#4214 = VECTOR ( 'NONE', #30216, 1000.000000000000000 ) ;
#4215 = DIRECTION ( 'NONE',  ( -2.698458740408365879E-16, 1.000000000000000000, 0.000000000000000000 ) ) ;
#4216 = CARTESIAN_POINT ( 'NONE',  ( 133.7287565553229456, -4.000000000000003553, 8.500000000000003553 ) ) ;
#4217 = CARTESIAN_POINT ( 'NONE',  ( 10.18658029549746935, 13.84849823568026217, -17.67057034492011525 ) ) ;
#4218 = DIRECTION ( 'NONE',  ( 0.9510565162951536422, 2.566386769018988816E-16, 0.3090169943749472292 ) ) ;
#4219 = EDGE_LOOP ( 'NONE', ( #592, #19702, #1563, #16813 ) ) ;
#4220 = LINE ( 'NONE', #29621, #18324 ) ;
#4221 = CARTESIAN_POINT ( 'NONE',  ( 12.63667343406881294, 8.631100619704961119, -15.02124387326777111 ) ) ;
#4222 = ORIENTED_EDGE ( 'NONE', *, *, #9963, .T. ) ;
#4223 = LINE ( 'NONE', #22999, #19793 ) ;
#4224 = PLANE ( 'NONE',  #18580 ) ;
#4225 = VECTOR ( 'NONE', #7313, 1000.000000000000000 ) ;
#4226 = CARTESIAN_POINT ( 'NONE',  ( 14.34656430690936624, 9.113120221615268690, -15.03016663717492563 ) ) ;
#4227 = ORIENTED_EDGE ( 'NONE', *, *, #17622, .F. ) ;
#4228 = CARTESIAN_POINT ( 'NONE',  ( 8.944584683310379702, 16.95159276115599667, -17.93331994345748726 ) ) ;
#4229 = CARTESIAN_POINT ( 'NONE',  ( 33.02439791605519304, -11.93986616049457261, -20.58189241239533374 ) ) ;
#4230 = ORIENTED_EDGE ( 'NONE', *, *, #20240, .T. ) ;
#4231 = CARTESIAN_POINT ( 'NONE',  ( 18.97422388862426601, -0.1098198481195374748, -14.77765307979439058 ) ) ;
#4232 = ADVANCED_FACE ( 'NONE', ( #25601 ), #23476, .T. ) ;
#4233 = CARTESIAN_POINT ( 'NONE',  ( 16.27660620799252911, 9.202420196601492464, -13.74949690087879439 ) ) ;
#4234 = EDGE_CURVE ( 'NONE', #2172, #2945, #12011, .T. ) ;
#4235 = CARTESIAN_POINT ( 'NONE',  ( 172.2287565553228887, -1.999999999999970024, -12.16987298107780369 ) ) ;
#4236 = ADVANCED_FACE ( 'NONE', ( #3038 ), #21326, .T. ) ;
#4237 = CARTESIAN_POINT ( 'NONE',  ( 20.76230466941008146, -3.840972149463459218, -19.45223659164069474 ) ) ;
#4238 = VECTOR ( 'NONE', #7975, 1000.000000000000000 ) ;
#4239 = ORIENTED_EDGE ( 'NONE', *, *, #18884, .T. ) ;
#4240 = LINE ( 'NONE', #21152, #14271 ) ;
#4242 = ORIENTED_EDGE ( 'NONE', *, *, #10480, .F. ) ;
#4241 = CARTESIAN_POINT ( 'NONE',  ( 172.0152310637604671, -4.999999999999970690, -26.04193191628311155 ) ) ;
#4243 = CIRCLE ( 'NONE', #21291, 3.150000000000000799 ) ;
#4244 = DIRECTION ( 'NONE',  ( -0.8090169943749474513, -2.183098979609982436E-16, -0.5877852522924731371 ) ) ;
#4246 = LINE ( 'NONE', #3948, #5558 ) ;
#4245 = VECTOR ( 'NONE', #14961, 999.9999999999998863 ) ;
#4247 = ORIENTED_EDGE ( 'NONE', *, *, #20819, .F. ) ;
#4248 = CARTESIAN_POINT ( 'NONE',  ( 149.5152310637606092, -10.00000000000000178, -28.60870317832789667 ) ) ;
#4249 = CARTESIAN_POINT ( 'NONE',  ( 34.07550722110926955, -11.19626532300822674, -18.14763417942564061 ) ) ;
#4250 = CARTESIAN_POINT ( 'NONE',  ( 10.67622114788023246, 9.011142735252827052, -16.40800301137445416 ) ) ;
#4251 = PRODUCT_DEFINITION_SHAPE ( 'NONE', 'NONE',  #15091 ) ;
#4252 = VERTEX_POINT ( 'NONE', #9263 ) ;
#4253 = CARTESIAN_POINT ( 'NONE',  ( 26.07968421886551980, -9.001936657367064498, -13.61655714643126913 ) ) ;
#4254 = DIRECTION ( 'NONE',  ( -2.698458740408365879E-16, 1.000000000000000000, 0.000000000000000000 ) ) ;
#4255 = CARTESIAN_POINT ( 'NONE',  ( 11.89844042902047505, 9.910446108148166289, -16.74492965742949835 ) ) ;
#4256 = CARTESIAN_POINT ( 'NONE',  ( 142.0152310637605808, -10.00000000000000355, -17.38167787843871182 ) ) ;
#4257 = ORIENTED_EDGE ( 'NONE', *, *, #9754, .T. ) ;
#4258 = DIRECTION ( 'NONE',  ( 0.9510565162951536422, 0.000000000000000000, -0.3090169943749475623 ) ) ;
#4259 = COLOUR_RGB ( '', 0.08235294, 0.09019608, 0.10196078) ;
#4260 = CARTESIAN_POINT ( 'NONE',  ( 12.93612603019711571, 8.763434079353435990, -14.78257486846209545 ) ) ;
#4262 = EDGE_LOOP ( 'NONE', ( #482, #26047, #14335, #26472, #19065 ) ) ;
#4261 = CARTESIAN_POINT ( 'NONE',  ( 105.8449596982085836, -4.999999999999988454, -76.90086459576200184 ) ) ;
#4263 = ORIENTED_EDGE ( 'NONE', *, *, #23252, .F. ) ;
#4264 = CARTESIAN_POINT ( 'NONE',  ( 97.96609169890469104, -4.999999999999991118, 71.17653192172720367 ) ) ;
#4265 = ORIENTED_EDGE ( 'NONE', *, *, #22032, .F. ) ;
#4266 = CARTESIAN_POINT ( 'NONE',  ( 13.66828981435543078, 8.811555337407297017, -15.47779131845255307 ) ) ;
#4267 = AXIS2_PLACEMENT_3D ( 'NONE', #7829, #24166, #5696 ) ;
#4268 = CARTESIAN_POINT ( 'NONE',  ( 23.86816030614728135, 2.079196616232401595, -15.13732202275373062 ) ) ;
#4269 = CARTESIAN_POINT ( 'NONE',  ( 22.03599841643320190, -0.8527435389730096960, -19.82300248246997398 ) ) ;
#4270 = EDGE_LOOP ( 'NONE', ( #27964, #4375, #10250, #2763 ) ) ;
#4271 = CARTESIAN_POINT ( 'NONE',  ( 18.54205238286641588, 5.219565156008159512, -20.23764637224795848 ) ) ;
#4272 = CARTESIAN_POINT ( 'NONE',  ( 166.1922820468853672, -4.999999999999972466, -28.06379628232387802 ) ) ;
#4273 = CYLINDRICAL_SURFACE ( 'NONE', #5951, 3.000000000000002665 ) ;
#4274 = EDGE_CURVE ( 'NONE', #19861, #4517, #18590, .T. ) ;
#4275 = CARTESIAN_POINT ( 'NONE',  ( 20.51249478307574847, 1.942573248051725709, -13.31196225760961838 ) ) ;
#4276 = DIRECTION ( 'NONE',  ( -0.8090169943749474513, -2.183098979609982436E-16, 0.5877852522924731371 ) ) ;
#4277 = DIRECTION ( 'NONE',  ( 0.9510565162951535312, 2.566386769018988816E-16, -0.3090169943749475623 ) ) ;
#4278 = VECTOR ( 'NONE', #20908, 1000.000000000000000 ) ;
#4279 = EDGE_LOOP ( 'NONE', ( #8590, #23241, #26425, #4448, #7928 ) ) ;
#4280 = DIRECTION ( 'NONE',  ( -2.698458740408365879E-16, 1.000000000000000000, 0.000000000000000000 ) ) ;
#4281 = DIRECTION ( 'NONE',  ( -2.698458740408365879E-16, 1.000000000000000000, 0.000000000000000000 ) ) ;
#4282 = CARTESIAN_POINT ( 'NONE',  ( 148.6922820468853672, -10.00000000000000355, 2.247092850131519715 ) ) ;
#4283 = VECTOR ( 'NONE', #20313, 1000.000000000000000 ) ;
#4284 = ORIENTED_EDGE ( 'NONE', *, *, #18689, .F. ) ;
#4285 = ORIENTED_EDGE ( 'NONE', *, *, #23334, .F. ) ;
#4286 = CARTESIAN_POINT ( 'NONE',  ( 130.7287565553229456, -4.999999999999983125, 3.500000000000003109 ) ) ;
#4287 = CARTESIAN_POINT ( 'NONE',  ( 30.87383483136289541, -10.13329766739009052, -15.36655316835725138 ) ) ;
#4288 = CARTESIAN_POINT ( 'NONE',  ( 11.05541531668977662, 17.68942339022145305, -17.92279151347708677 ) ) ;
#4289 = CARTESIAN_POINT ( 'NONE',  ( 33.57712230886461668, -13.32773824946660923, -19.76201999124979736 ) ) ;
#4290 = ADVANCED_FACE ( 'NONE', ( #5766 ), #12617, .T. ) ;
#4291 = VERTEX_POINT ( 'NONE', #17648 ) ;
#4292 = EDGE_LOOP ( 'NONE', ( #1664, #4911, #6108, #16603 ) ) ;
#4293 = VERTEX_POINT ( 'NONE', #21934 ) ;
#4294 = DIRECTION ( 'NONE',  ( -0.8090169943749474513, -2.183098979609982436E-16, -0.5877852522924731371 ) ) ;
#4295 = CARTESIAN_POINT ( 'NONE',  ( 9.641352920869014298, 17.66888146263751125, -17.91030124961049097 ) ) ;
#4296 = CARTESIAN_POINT ( 'NONE',  ( 161.1922820468853388, -9.999999999999998224, -10.74328820663507678 ) ) ;
#4297 = CARTESIAN_POINT ( 'NONE',  ( 159.5152310637604387, -1.999999999999974021, -4.391296821672111328 ) ) ;
#4298 = ORIENTED_EDGE ( 'NONE', *, *, #28149, .F. ) ;
#4299 = CARTESIAN_POINT ( 'NONE',  ( 127.7287565553229598, -1.999999999999982681, -33.50000000000000000 ) ) ;
#4300 = ORIENTED_EDGE ( 'NONE', *, *, #24180, .F. ) ;
#4301 = CARTESIAN_POINT ( 'NONE',  ( 12.86884521499632150, 9.516296226583106588, -16.11496277528728527 ) ) ;
#4302 = CARTESIAN_POINT ( 'NONE',  ( 34.91913293194685508, -14.86421081092256280, -20.09741683264573808 ) ) ;
#4303 = CARTESIAN_POINT ( 'NONE',  ( 28.09718568327657806, -5.958257988085632562, -17.17874431236187149 ) ) ;
#4304 = VECTOR ( 'NONE', #27271, 1000.000000000000000 ) ;
#4305 = CARTESIAN_POINT ( 'NONE',  ( 420.0000000000002274, 34.64101615137744972, 14.00000000000000178 ) ) ;
#4306 = DIRECTION ( 'NONE',  ( 1.000000000000000000, 0.000000000000000000, 0.000000000000000000 ) ) ;
#4307 = CARTESIAN_POINT ( 'NONE',  ( 30.07542022419311678, -8.155067017681195907, -14.09159111155252120 ) ) ;
#4308 = VECTOR ( 'NONE', #29668, 999.9999999999998863 ) ;
#4309 = CARTESIAN_POINT ( 'NONE',  ( 22.63726333831294468, -4.877931240889711972, -12.86144741616201870 ) ) ;
#4310 = VERTEX_POINT ( 'NONE', #29000 ) ;
#4311 = LINE ( 'NONE', #20928, #2577 ) ;
#4312 = DIRECTION ( 'NONE',  ( 0.000000000000000000, 0.000000000000000000, 1.000000000000000000 ) ) ;
#4313 = FACE_OUTER_BOUND ( 'NONE', #20068, .T. ) ;
#4314 = CARTESIAN_POINT ( 'NONE',  ( 163.6922820468853672, -1.999999999999972244, -26.58683881228715862 ) ) ;
#4315 = CARTESIAN_POINT ( 'NONE',  ( 12.37169234869624646, 8.529253869913038244, -15.23127513898213081 ) ) ;
#4316 = DIRECTION ( 'NONE',  ( -2.698458740408365879E-16, 1.000000000000000000, 0.000000000000000000 ) ) ;
#4317 = EDGE_CURVE ( 'NONE', #26921, #3757, #22235, .T. ) ;
#4318 = EDGE_CURVE ( 'NONE', #5150, #6558, #3479, .T. ) ;
#4319 = AXIS2_PLACEMENT_3D ( 'NONE', #7754, #17063, #26391 ) ;
#4320 = FACE_OUTER_BOUND ( 'NONE', #12707, .T. ) ;
#4321 = VERTEX_POINT ( 'NONE', #29148 ) ;
#4322 = CARTESIAN_POINT ( 'NONE',  ( 9.641350810849047548, 17.66889113945805789, -17.92279151347709032 ) ) ;
#4323 = EDGE_CURVE ( 'NONE', #17861, #8041, #5461, .T. ) ;
#4324 = CARTESIAN_POINT ( 'NONE',  ( 29.99716341122577745, -11.34936846952144585, -14.08097903537201212 ) ) ;
#4325 = LINE ( 'NONE', #23245, #3936 ) ;
#4326 = CARTESIAN_POINT ( 'NONE',  ( 98.45422169453954098, -4.999999999999990230, -71.53117912275099854 ) ) ;
#4327 = EDGE_CURVE ( 'NONE', #10549, #28746, #1347, .T. ) ;
#4329 = EDGE_LOOP ( 'NONE', ( #16127, #13012, #24777, #7957 ) ) ;
#4328 = CARTESIAN_POINT ( 'NONE',  ( 26.85315702054868936, -3.432285194908070380, -17.01323758698984889 ) ) ;
#4330 = CIRCLE ( 'NONE', #21386, 13.00000000000000178 ) ;
#4331 = VERTEX_POINT ( 'NONE', #17055 ) ;
#4332 = LINE ( 'NONE', #27278, #22744 ) ;
#4333 = CARTESIAN_POINT ( 'NONE',  ( 11.05541531668977662, 17.68942339022145305, -23.00000000000000711 ) ) ;
#4334 = VECTOR ( 'NONE', #17777, 1000.000000000000000 ) ;
#4335 = CARTESIAN_POINT ( 'NONE',  ( 35.16668739017224965, -20.46881214373840763, -20.22602438870426766 ) ) ;
#4336 = CARTESIAN_POINT ( 'NONE',  ( 137.0152310637605524, -4.999999999999980460, -1.521174642513229451E-14 ) ) ;
#4337 = CARTESIAN_POINT ( 'NONE',  ( 27.44219139316946965, -6.774709612358828181, -18.29578255718776703 ) ) ;
#4338 = FACE_OUTER_BOUND ( 'NONE', #23479, .T. ) ;
#4339 = CARTESIAN_POINT ( 'NONE',  ( 22.40466763571637543, -1.191653471825661059, -14.65485681160645548 ) ) ;
#4340 = VERTEX_POINT ( 'NONE', #6065 ) ;
#4341 = DIRECTION ( 'NONE',  ( -2.698458740408365879E-16, 1.000000000000000000, 0.000000000000000000 ) ) ;
#4342 =( NAMED_UNIT ( * ) SI_UNIT ( $, .STERADIAN. ) SOLID_ANGLE_UNIT ( ) );
#4343 = CARTESIAN_POINT ( 'NONE',  ( 17.78134717446047119, 9.288666448780150020, -20.14505390916605521 ) ) ;
#4344 = CARTESIAN_POINT ( 'NONE',  ( 29.03550452591436937, -6.934775515252377787, -18.27713033076000215 ) ) ;
#4345 = ORIENTED_EDGE ( 'NONE', *, *, #2685, .F. ) ;
#4346 = ORIENTED_EDGE ( 'NONE', *, *, #1277, .F. ) ;
#4347 = CARTESIAN_POINT ( 'NONE',  ( 169.5152310637605240, -9.999999999999994671, -28.60870317832789667 ) ) ;
#4348 = VECTOR ( 'NONE', #9477, 1000.000000000000000 ) ;
#4349 = DIRECTION ( 'NONE',  ( 0.000000000000000000, 0.000000000000000000, 1.000000000000000000 ) ) ;
#4350 = CIRCLE ( 'NONE', #3861, 9.000000000000007105 ) ;
#4351 = VERTEX_POINT ( 'NONE', #14746 ) ;
#4352 = CARTESIAN_POINT ( 'NONE',  ( 107.5362657617971820, -4.999999999999988454, -78.12967037883245780 ) ) ;
#4353 = DIRECTION ( 'NONE',  ( 0.000000000000000000, -2.775557561562890735E-17, 1.000000000000000000 ) ) ;
#4354 = DIRECTION ( 'NONE',  ( 0.000000000000000000, 0.000000000000000000, 1.000000000000000000 ) ) ;
#4355 = CARTESIAN_POINT ( 'NONE',  ( 167.0152310637604387, -1.999999999999972244, 1.702185954127501066 ) ) ;
#4356 = CARTESIAN_POINT ( 'NONE',  ( 25.25756851182965335, -6.311239348595019116, -19.54001279501058264 ) ) ;
#4357 = CARTESIAN_POINT ( 'NONE',  ( 16.37314578033188894, 3.237113944496374351, -18.86778596048347723 ) ) ;
#4358 = EDGE_CURVE ( 'NONE', #22694, #2461, #15203, .T. ) ;
#4359 = CARTESIAN_POINT ( 'NONE',  ( 34.14034160798153295, -12.36551392957089135, -20.90432844665832590 ) ) ;
#4360 = CARTESIAN_POINT ( 'NONE',  ( 11.82447321682112751, 8.672047275158794477, -15.63808403058127006 ) ) ;
#4361 = EDGE_CURVE ( 'NONE', #29222, #4117, #10634, .T. ) ;
#4362 = EDGE_CURVE ( 'NONE', #16946, #16967, #19944, .T. ) ;
#4363 = CARTESIAN_POINT ( 'NONE',  ( 15.00000000000000000, 1.387778780781445429E-16, -5.000000000000000000 ) ) ;
#4364 = PLANE ( 'NONE',  #29591 ) ;
#4365 = ADVANCED_FACE ( 'NONE', ( #15352 ), #15048, .T. ) ;
#4366 = CARTESIAN_POINT ( 'NONE',  ( 9.668188843004273281, 16.22590751635418371, -17.88494344602179709 ) ) ;
#4367 = LINE ( 'NONE', #29918, #25349 ) ;
#4368 = ORIENTED_EDGE ( 'NONE', *, *, #9964, .T. ) ;
#4369 = LINE ( 'NONE', #13670, #26633 ) ;
#4370 = CARTESIAN_POINT ( 'NONE',  ( 10.33811693838771717, 18.38618951776012267, -23.00000000000000711 ) ) ;
#4371 = VERTEX_POINT ( 'NONE', #28859 ) ;
#4372 = VECTOR ( 'NONE', #5031, 1000.000000000000000 ) ;
#4373 = DIRECTION ( 'NONE',  ( 0.9510565162951535312, 2.566386769018988816E-16, -0.3090169943749475623 ) ) ;
#4374 = LINE ( 'NONE', #24996, #18052 ) ;
#4375 = ORIENTED_EDGE ( 'NONE', *, *, #20770, .F. ) ;
#4376 = FACE_OUTER_BOUND ( 'NONE', #7178, .T. ) ;
#4377 = ORIENTED_EDGE ( 'NONE', *, *, #19365, .F. ) ;
#4378 = VECTOR ( 'NONE', #11391, 1000.000000000000000 ) ;
#4379 = ORIENTED_EDGE ( 'NONE', *, *, #24144, .T. ) ;
#4380 = CARTESIAN_POINT ( 'NONE',  ( 9.631286188771861489, 13.80229212302790920, -16.84020087884530881 ) ) ;
#4381 = CARTESIAN_POINT ( 'NONE',  ( 35.54859390953723164, -23.18451583373416014, -14.99999999999999822 ) ) ;
#4382 = CARTESIAN_POINT ( 'NONE',  ( 19.77430725462212635, 0.2453161447429414443, -14.21425550582737074 ) ) ;
#4383 = CARTESIAN_POINT ( 'NONE',  ( 14.82995595102070752, 5.192148136363496036, -18.54057990209784634 ) ) ;
#4384 = VERTEX_POINT ( 'NONE', #14894 ) ;
#4385 = DIRECTION ( 'NONE',  ( 1.000000000000000000, 4.440892098500622217E-16, 0.000000000000000000 ) ) ;
#4386 = CARTESIAN_POINT ( 'NONE',  ( 24.47917272657372223, 1.093256025350008542, -14.89707007128618699 ) ) ;
#4387 = ORIENTED_EDGE ( 'NONE', *, *, #9586, .F. ) ;
#4388 = DIRECTION ( 'NONE',  ( 0.000000000000000000, 0.000000000000000000, 1.000000000000000000 ) ) ;
#4389 = CIRCLE ( 'NONE', #7309, 8.000000000000005329 ) ;
#4391 = EDGE_LOOP ( 'NONE', ( #13774, #20993, #1262, #3346, #16201 ) ) ;
#4390 = CARTESIAN_POINT ( 'NONE',  ( -8.000000000000000000, 0.000000000000000000, 18.00000000000000000 ) ) ;
#4392 = ORIENTED_EDGE ( 'NONE', *, *, #25112, .T. ) ;
#4393 = VECTOR ( 'NONE', #13496, 1000.000000000000000 ) ;
#4394 = DIRECTION ( 'NONE',  ( -0.9510565162951536422, -2.566386769018988816E-16, -0.3090169943749472292 ) ) ;
#4395 = VECTOR ( 'NONE', #13833, 1000.000000000000000 ) ;
#4396 = CARTESIAN_POINT ( 'NONE',  ( 13.77718166750865869, 8.859676595473324312, -15.39100258941132182 ) ) ;
#4397 = ORIENTED_EDGE ( 'NONE', *, *, #2348, .F. ) ;
#4398 = CARTESIAN_POINT ( 'NONE',  ( 34.39665924806198660, -11.72086467124742981, -18.77862448471655199 ) ) ;
#4399 = CARTESIAN_POINT ( 'NONE',  ( 10.66363677402306287, 9.067800744973538940, -16.41328759676781246 ) ) ;
#4400 = EDGE_LOOP ( 'NONE', ( #4498, #8803, #25683, #21105 ) ) ;
#4401 = EDGE_CURVE ( 'NONE', #22420, #8035, #12919, .T. ) ;
#4402 = ADVANCED_FACE ( 'NONE', ( #24236 ), #23941, .T. ) ;
#4403 = CARTESIAN_POINT ( 'NONE',  ( 24.78692427941192733, -9.284778175067517125, -17.23615439686343720 ) ) ;
#4404 = DIRECTION ( 'NONE',  ( -2.698458740408365879E-16, 1.000000000000000000, 0.000000000000000000 ) ) ;
#4405 = ADVANCED_FACE ( 'NONE', ( #7895 ), #724, .T. ) ;
#4406 = CARTESIAN_POINT ( 'NONE',  ( 10.47204342302745417, 16.45208460095963687, -17.33479495221483901 ) ) ;
#4407 = LINE ( 'NONE', #27193, #3389 ) ;
#4408 = EDGE_CURVE ( 'NONE', #3548, #22258, #3336, .T. ) ;
#4409 = PLANE ( 'NONE',  #1822 ) ;
#4410 = AXIS2_PLACEMENT_3D ( 'NONE', #29847, #8853, #18167 ) ;
#4411 = ORIENTED_EDGE ( 'NONE', *, *, #24280, .F. ) ;
#4412 = VECTOR ( 'NONE', #12874, 1000.000000000000000 ) ;
#4413 = CARTESIAN_POINT ( 'NONE',  ( 139.7287565553230024, -10.00000000000000533, 0.8205080756887930260 ) ) ;
#4414 = CARTESIAN_POINT ( 'NONE',  ( 12.52778158092594474, 8.582979361647906202, -15.10803260229456946 ) ) ;
#4415 = EDGE_LOOP ( 'NONE', ( #19865, #7183, #11633, #28782 ) ) ;
#4416 = VERTEX_POINT ( 'NONE', #26691 ) ;
#4417 = CARTESIAN_POINT ( 'NONE',  ( 63.44486372867152824, 109.8897274573438096, -17.99999999999998934 ) ) ;
#4418 = VERTEX_POINT ( 'NONE', #24382 ) ;
#4419 = CARTESIAN_POINT ( 'NONE',  ( 9.663058643182488083, 16.24943526668553062, -17.89776827055807118 ) ) ;
#4420 = CARTESIAN_POINT ( 'NONE',  ( 20.92570677221209507, 1.074447142478794470, -13.03661572703551919 ) ) ;
#4421 = CARTESIAN_POINT ( 'NONE',  ( 20.98456156242603754, -1.805893270886621327, -19.41059277335735089 ) ) ;
#4422 = CARTESIAN_POINT ( 'NONE',  ( 18.97628335640213493, 0.9430780577607489334, -14.77698032187241850 ) ) ;
#4423 = DIRECTION ( 'NONE',  ( -0.06678507476159963041, 0.9947851038922184141, -0.07708664516786083165 ) ) ;
#4424 = LINE ( 'NONE', #23045, #6936 ) ;
#4425 = CARTESIAN_POINT ( 'NONE',  ( 25.45462155318426767, -0.2439708902934435431, -15.99927030562601438 ) ) ;
#4426 = DIRECTION ( 'NONE',  ( -2.698458740408365879E-16, 1.000000000000000000, 0.000000000000000000 ) ) ;
#4427 = AXIS2_PLACEMENT_3D ( 'NONE', #20098, #27758, #15665 ) ;
#4428 = DIRECTION ( 'NONE',  ( -2.698458740408366372E-16, 1.000000000000000000, 0.000000000000000000 ) ) ;
#4429 = VECTOR ( 'NONE', #12918, 1000.000000000000000 ) ;
#4430 = CARTESIAN_POINT ( 'NONE',  ( 10.35864918915110877, 16.97212501191939538, -17.91928203681695564 ) ) ;
#4431 = CARTESIAN_POINT ( 'NONE',  ( 0.000000000000000000, 0.000000000000000000, 18.00000000000000000 ) ) ;
#4432 = CARTESIAN_POINT ( 'NONE',  ( 13.00000000000001243, 55.00000000000000711, -23.00000000000000000 ) ) ;
#4433 = ORIENTED_EDGE ( 'NONE', *, *, #19029, .T. ) ;
#4434 = ORIENTED_EDGE ( 'NONE', *, *, #26971, .T. ) ;
#4435 = EDGE_CURVE ( 'NONE', #8020, #8342, #12218, .T. ) ;
#4436 = FACE_OUTER_BOUND ( 'NONE', #1501, .T. ) ;
#4437 = CARTESIAN_POINT ( 'NONE',  ( 15.78240017141095741, 4.038647184180326200, -18.77507866864583619 ) ) ;
#4438 = ADVANCED_FACE ( 'NONE', ( #19783 ), #18047, .T. ) ;
#4439 = CARTESIAN_POINT ( 'NONE',  ( 11.05544237569323762, 17.68929929418238700, -17.89823164173536441 ) ) ;
#4440 = CARTESIAN_POINT ( 'NONE',  ( 174.5152310637604387, -1.999999999999969358, -21.71180489736091346 ) ) ;
#4441 = ADVANCED_FACE ( 'NONE', ( #4376 ), #10790, .T. ) ;
#4442 = ORIENTED_EDGE ( 'NONE', *, *, #8692, .T. ) ;
#4443 = ORIENTED_EDGE ( 'NONE', *, *, #22460, .T. ) ;
#4444 = CARTESIAN_POINT ( 'NONE',  ( 9.641354186875979337, 17.66887565656821124, -17.90893343548146177 ) ) ;
#4445 = CARTESIAN_POINT ( 'NONE',  ( 12.75684812230466925, 7.626178201396932366, -14.92546252573342258 ) ) ;
#4446 = DIRECTION ( 'NONE',  ( -1.000000000000000000, 0.000000000000000000, -0.000000000000000000 ) ) ;
#4447 = LINE ( 'NONE', #18171, #22289 ) ;
#4448 = ORIENTED_EDGE ( 'NONE', *, *, #27732, .T. ) ;
#4449 = EDGE_LOOP ( 'NONE', ( #23196, #28449, #29700, #23102, #15467 ) ) ;
#4450 = DIRECTION ( 'NONE',  ( -0.5877852522924731371, -1.586114251531760728E-16, -0.8090169943749474513 ) ) ;
#4451 = EDGE_LOOP ( 'NONE', ( #14119, #19459, #2931, #19006 ) ) ;
#4452 = CARTESIAN_POINT ( 'NONE',  ( 10.35864918915110877, 16.97212501191939538, -17.97192418671891190 ) ) ;
#4453 = CIRCLE ( 'NONE', #7372, 8.000000000000005329 ) ;
#4454 = ORIENTED_EDGE ( 'NONE', *, *, #14324, .T. ) ;
#4456 = VECTOR ( 'NONE', #7861, 1000.000000000000000 ) ;
#4455 = CARTESIAN_POINT ( 'NONE',  ( 33.49783966318349115, -10.45910432307822902, -18.51641766868578287 ) ) ;
#4457 = CARTESIAN_POINT ( 'NONE',  ( 26.84970692451943819, -5.812874930055231815, -14.04107299160273037 ) ) ;
#4458 = LINE ( 'NONE', #2780, #15973 ) ;
#4459 = DIRECTION ( 'NONE',  ( -2.698458740408365879E-16, 1.000000000000000000, 0.000000000000000000 ) ) ;
#4460 = APPLICATION_PROTOCOL_DEFINITION ( 'draft international standard', 'automotive_design', 1998, #28636 ) ;
#4461 = CARTESIAN_POINT ( 'NONE',  ( 14.77364001808635585, 4.929448384924057791, -16.82930887520970131 ) ) ;
#4462 = CARTESIAN_POINT ( 'NONE',  ( 22.71651454236177514, -3.376241010138071541, -20.62701743264632270 ) ) ;
#4463 = ORIENTED_EDGE ( 'NONE', *, *, #16308, .F. ) ;
#4464 = ORIENTED_EDGE ( 'NONE', *, *, #15971, .F. ) ;
#4465 = EDGE_CURVE ( 'NONE', #9448, #1955, #8640, .T. ) ;
#4466 = DIRECTION ( 'NONE',  ( -2.698458740408365879E-16, 1.000000000000000000, 0.000000000000000000 ) ) ;
#4467 = ORIENTED_EDGE ( 'NONE', *, *, #3821, .F. ) ;
#4468 = DIRECTION ( 'NONE',  ( 0.000000000000000000, 0.000000000000000000, 1.000000000000000000 ) ) ;
#4469 = LINE ( 'NONE', #13759, #452 ) ;
#4470 = VECTOR ( 'NONE', #1873, 1000.000000000000000 ) ;
#4471 = CARTESIAN_POINT ( 'NONE',  ( 14.01590296442413397, -5.000000000000014211, -43.13651381225401593 ) ) ;
#4472 = ADVANCED_FACE ( 'NONE', ( #11380 ), #2104, .T. ) ;
#4473 = CARTESIAN_POINT ( 'NONE',  ( 10.72001338896670397, 16.63476371493014128, -15.95452473000899118 ) ) ;
#4474 = CARTESIAN_POINT ( 'NONE',  ( 26.95082352492110189, -12.40836276091286194, -17.97502949936508898 ) ) ;
#4475 = ORIENTED_EDGE ( 'NONE', *, *, #19340, .F. ) ;
#4476 = DIRECTION ( 'NONE',  ( -0.000000000000000000, -0.000000000000000000, 1.000000000000000000 ) ) ;
#4477 = ORIENTED_EDGE ( 'NONE', *, *, #6194, .F. ) ;
#4478 = CARTESIAN_POINT ( 'NONE',  ( 9.913797604922770290, 16.41941541294738727, -16.50570979788118464 ) ) ;
#4479 = CARTESIAN_POINT ( 'NONE',  ( 15.22094575638775282, 5.866722348926807662, -16.67377462076821715 ) ) ;
#4480 = CARTESIAN_POINT ( 'NONE',  ( 158.6922820468853956, -1.999999999999973133, -23.73366926340167637 ) ) ;
#4481 = DIRECTION ( 'NONE',  ( 0.9510565162951536422, 2.566386769018988816E-16, 0.3090169943749472292 ) ) ;
#4483 = EDGE_LOOP ( 'NONE', ( #18513, #16334, #16487, #12207 ) ) ;
#4482 = DIRECTION ( 'NONE',  ( -0.9510565162951536422, -2.566386769018988816E-16, -0.3090169943749472292 ) ) ;
#4484 = ORIENTED_EDGE ( 'NONE', *, *, #11831, .T. ) ;
#4485 = DIRECTION ( 'NONE',  ( -2.698458740408365879E-16, 1.000000000000000000, 0.000000000000000000 ) ) ;
#4486 = CARTESIAN_POINT ( 'NONE',  ( 12.35402573141577598, 9.564223303342972216, -15.24651908135525957 ) ) ;
#4487 = VERTEX_POINT ( 'NONE', #22698 ) ;
#4488 = CARTESIAN_POINT ( 'NONE',  ( 35.02155038278115740, -19.81678845073966500, -20.19863594638463411 ) ) ;
#4489 = CARTESIAN_POINT ( 'NONE',  ( 171.1922820468853104, -9.999999999999996447, -13.59645775552055902 ) ) ;
#4490 = CARTESIAN_POINT ( 'NONE',  ( 104.9340031866765344, -4.999999999999988454, 76.23901594897056100 ) ) ;
#4491 = VECTOR ( 'NONE', #1130, 1000.000000000000000 ) ;
#4492 = CARTESIAN_POINT ( 'NONE',  ( 22.98313442454129429, 1.505266882216666158, -15.27805348665062546 ) ) ;
#4493 = EDGE_LOOP ( 'NONE', ( #12397, #10329, #21160, #18160 ) ) ;
#4494 = CARTESIAN_POINT ( 'NONE',  ( 4.000000000000000000, -0.3902508023145602190, 3.244136187983970792E-16 ) ) ;
#4495 = SURFACE_SIDE_STYLE ('',( #18072 ) ) ;
#4496 = CARTESIAN_POINT ( 'NONE',  ( 28.19717681610909210, -11.01075670644066662, -19.96981485020118541 ) ) ;
#4497 = CARTESIAN_POINT ( 'NONE',  ( 25.16264305761801268, -10.69278474016982727, -17.18274900023375906 ) ) ;
#4498 = ORIENTED_EDGE ( 'NONE', *, *, #8284, .T. ) ;
#4499 = EDGE_CURVE ( 'NONE', #11139, #22675, #6820, .T. ) ;
#4500 = CARTESIAN_POINT ( 'NONE',  ( -24.99999999999998934, 55.00000000000000711, 29.99999999999999289 ) ) ;
#4501 = ADVANCED_FACE ( 'NONE', ( #27156 ), #6519, .T. ) ;
#4502 = DIRECTION ( 'NONE',  ( 0.9510565162951536422, 0.000000000000000000, -0.3090169943749475623 ) ) ;
#4503 = DIRECTION ( 'NONE',  ( -0.8090169943749474513, -2.183098979609982436E-16, 0.5877852522924731371 ) ) ;
#4504 = CARTESIAN_POINT ( 'NONE',  ( 164.5152310637604671, -4.999999999999973355, -1.826485974285146553E-14 ) ) ;
#4505 = CARTESIAN_POINT ( 'NONE',  ( 176.1922820468853388, -9.999999999999994671, -28.06379628232387802 ) ) ;
#4506 = VECTOR ( 'NONE', #3345, 1000.000000000000000 ) ;
#4507 = LINE ( 'NONE', #22535, #26779 ) ;
#4508 = CARTESIAN_POINT ( 'NONE',  ( 19.73758642798775753, -1.564653675968832314, -13.27997001701493041 ) ) ;
#4509 = CARTESIAN_POINT ( 'NONE',  ( 19.14470263920462401, 1.819183656627200829, -19.33730474122706866 ) ) ;
#4510 = CARTESIAN_POINT ( 'NONE',  ( 32.74140904187309786, -11.17293925747269867, -20.20304766317806866 ) ) ;
#4511 = SURFACE_STYLE_FILL_AREA ( #18392 ) ;
#4512 = CARTESIAN_POINT ( 'NONE',  ( 11.69419402147360110, 8.800013620902292999, -15.72776802682527730 ) ) ;
#4513 = CARTESIAN_POINT ( 'NONE',  ( 168.6922820468853388, -1.999999999999970912, -15.07341522555727664 ) ) ;
#4514 = DIRECTION ( 'NONE',  ( -0.5877852522924731371, -1.586114251531760728E-16, -0.8090169943749474513 ) ) ;
#4516 = ORIENTED_EDGE ( 'NONE', *, *, #20817, .T. ) ;
#4515 = CARTESIAN_POINT ( 'NONE',  ( 16.75072914628186282, 8.771658487634226731, -19.67538163746542779 ) ) ;
#4517 = VERTEX_POINT ( 'NONE', #29475 ) ;
#4518 = LINE ( 'NONE', #1793, #3721 ) ;
#4519 = CARTESIAN_POINT ( 'NONE',  ( 12.50481220565295004, 8.572828783776230921, -15.12633959982445653 ) ) ;
#4520 = ORIENTED_EDGE ( 'NONE', *, *, #10904, .T. ) ;
#4521 = FACE_BOUND ( 'NONE', #26367, .T. ) ;
#4522 = FACE_OUTER_BOUND ( 'NONE', #52, .T. ) ;
#4523 = AXIS2_PLACEMENT_3D ( 'NONE', #18153, #29674, #27513 ) ;
#4524 = CARTESIAN_POINT ( 'NONE',  ( 17.85084670134855145, 5.929878015568476712, -20.08862479909851828 ) ) ;
#4525 = ORIENTED_EDGE ( 'NONE', *, *, #913, .T. ) ;
#4526 = ORIENTED_EDGE ( 'NONE', *, *, #4631, .F. ) ;
#4527 = CARTESIAN_POINT ( 'NONE',  ( 9.113084692838755885, 16.17883023870341930, -17.05449542622726966 ) ) ;
#4528 = CARTESIAN_POINT ( 'NONE',  ( 35.54859390953724585, -23.18451583373416014, -17.99055332684694974 ) ) ;
#4529 = CARTESIAN_POINT ( 'NONE',  ( 20.44834407054411685, 8.573499863981592028, -15.78670165415130100 ) ) ;
#4530 = CARTESIAN_POINT ( 'NONE',  ( 27.39958189869922123, -12.72506959635235368, -13.65552181841346524 ) ) ;
#4531 = VECTOR ( 'NONE', #29792, 1000.000000000000000 ) ;
#4532 = LINE ( 'NONE', #5246, #23531 ) ;
#4533 = CARTESIAN_POINT ( 'NONE',  ( 21.02038916656773182, -4.531596735700774481, -13.49074533895851147 ) ) ;
#4534 = EDGE_CURVE ( 'NONE', #12234, #22051, #24997, .T. ) ;
#4535 = EDGE_CURVE ( 'NONE', #27081, #14637, #20683, .T. ) ;
#4536 = VERTEX_POINT ( 'NONE', #22852 ) ;
#4537 = EDGE_CURVE ( 'NONE', #28890, #29995, #11236, .T. ) ;
#4538 = CARTESIAN_POINT ( 'NONE',  ( 137.0152310637605808, -10.00000000000000533, 1.702185954127501066 ) ) ;
#4540 = EDGE_LOOP ( 'NONE', ( #10859, #19017, #15432, #25172 ) ) ;
#4539 = DIRECTION ( 'NONE',  ( 0.000000000000000000, 0.000000000000000000, 1.000000000000000000 ) ) ;
#4541 = CIRCLE ( 'NONE', #9384, 2.000000000000000000 ) ;
#4542 = LINE ( 'NONE', #13831, #19695 ) ;
#4543 = CARTESIAN_POINT ( 'NONE',  ( -4.000000000000010658, -2.309401076758525573, -0.3572655899081716435 ) ) ;
#4544 = CARTESIAN_POINT ( 'NONE',  ( 36.41702210941816986, -20.59343343131470050, -19.35259392719279603 ) ) ;
#4545 = CARTESIAN_POINT ( 'NONE',  ( 12.62682997171803123, 7.576475742438638861, -15.02849783152220908 ) ) ;
#4546 = ORIENTED_EDGE ( 'NONE', *, *, #11285, .F. ) ;
#4547 = VECTOR ( 'NONE', #6004, 1000.000000000000000 ) ;
#4548 = DIRECTION ( 'NONE',  ( 1.000000000000000000, 2.698458740408365879E-16, -1.110223024625156540E-16 ) ) ;
#4549 = LINE ( 'NONE', #27632, #22098 ) ;
#4550 = CARTESIAN_POINT ( 'NONE',  ( 10.49225533350670858, 16.35939020308235925, -17.32643665990597981 ) ) ;
#4551 = FACE_BOUND ( 'NONE', #21761, .T. ) ;
#4552 = ORIENTED_EDGE ( 'NONE', *, *, #26866, .T. ) ;
#4553 = LINE ( 'NONE', #9108, #1333 ) ;
#4554 = VERTEX_POINT ( 'NONE', #6669 ) ;
#4555 = PLANE ( 'NONE',  #17335 ) ;
#4556 = CARTESIAN_POINT ( 'NONE',  ( 2.500000000000000444, 1.178949249685215417, -2.042000000000002036 ) ) ;
#4557 = VERTEX_POINT ( 'NONE', #15510 ) ;
#4558 = CARTESIAN_POINT ( 'NONE',  ( 143.6922820468854525, -10.00000000000000355, -35.24709285013155835 ) ) ;
#4559 = VERTEX_POINT ( 'NONE', #22553 ) ;
#4560 = CARTESIAN_POINT ( 'NONE',  ( 9.668122305056073174, 16.22621266786625327, -17.88497096177859191 ) ) ;
#4561 = CARTESIAN_POINT ( 'NONE',  ( 22.18457322443145330, -2.050108300791262828, -13.94172724511641448 ) ) ;
#4562 = CARTESIAN_POINT ( 'NONE',  ( 21.24065112674864864, -1.570060580458334965, -19.57950003236798864 ) ) ;
#4563 = ORIENTED_EDGE ( 'NONE', *, *, #2859, .T. ) ;
#4564 = CARTESIAN_POINT ( 'NONE',  ( 16.05281274719596496, 2.901206577426825639, -17.92093306952238407 ) ) ;
#4565 = DIRECTION ( 'NONE',  ( 0.5877852522924731371, 0.000000000000000000, 0.8090169943749474513 ) ) ;
#4566 = CARTESIAN_POINT ( 'NONE',  ( 5.637851296924623057E-15, 9.237604307034036566, -0.7145311798163362926 ) ) ;
#4567 = DIRECTION ( 'NONE',  ( 1.000000000000000000, 2.891205793294675861E-16, 0.000000000000000000 ) ) ;
#4568 = CARTESIAN_POINT ( 'NONE',  ( 27.51942754507220812, -5.605608590038333006, -14.64806962472005658 ) ) ;
#4569 = ADVANCED_FACE ( 'NONE', ( #25135 ), #24842, .T. ) ;
#4570 = AXIS2_PLACEMENT_3D ( 'NONE', #25153, #8512, #6081 ) ;
#4571 = ADVANCED_FACE ( 'NONE', ( #13373 ), #1802, .T. ) ;
#4572 = EDGE_CURVE ( 'NONE', #8702, #1753, #3930, .T. ) ;
#4573 = CARTESIAN_POINT ( 'NONE',  ( 139.5152310637605808, -1.999999999999978684, -30.37205893520530964 ) ) ;
#4574 = ADVANCED_FACE ( 'NONE', ( #25434 ), #21946, .T. ) ;
#4575 = DIRECTION ( 'NONE',  ( -0.5877852522924731371, -1.586114251531760728E-16, -0.8090169943749474513 ) ) ;
#4576 = DIRECTION ( 'NONE',  ( 1.110223024625156540E-16, 2.995891024602366092E-32, 1.000000000000000000 ) ) ;
#4577 = DIRECTION ( 'NONE',  ( -0.000000000000000000, -0.000000000000000000, -1.000000000000000000 ) ) ;
#4578 = LINE ( 'NONE', #13867, #12860 ) ;
#4579 = LINE ( 'NONE', #4720, #3903 ) ;
#4580 = DIRECTION ( 'NONE',  ( -1.000000000000000000, 0.000000000000000000, -0.000000000000000000 ) ) ;
#4581 = DIRECTION ( 'NONE',  ( 0.3090169943749472292, 8.338696094057992503E-17, -0.9510565162951536422 ) ) ;
#4582 = ORIENTED_EDGE ( 'NONE', *, *, #995, .F. ) ;
#4583 = CARTESIAN_POINT ( 'NONE',  ( 11.15915788317279578, 9.388133443793682531, -17.26837529997955301 ) ) ;
#4584 = ORIENTED_EDGE ( 'NONE', *, *, #6778, .F. ) ;
#4585 = DIRECTION ( 'NONE',  ( 1.110223024625156540E-16, 2.995891024602366092E-32, 1.000000000000000000 ) ) ;
#4586 = CARTESIAN_POINT ( 'NONE',  ( 19.52227536296714305, 7.868296793410291201, -18.00468392081665669 ) ) ;
#4587 = CARTESIAN_POINT ( 'NONE',  ( 11.27564905058850719, 16.67940341329043363, -16.78475148866115774 ) ) ;
#4588 = CARTESIAN_POINT ( 'NONE',  ( 34.93238815599637803, -19.41622979634004764, -20.17168434421570922 ) ) ;
#4589 = ORIENTED_EDGE ( 'NONE', *, *, #12510, .T. ) ;
#4590 = ORIENTED_EDGE ( 'NONE', *, *, #5811, .T. ) ;
#4591 = CARTESIAN_POINT ( 'NONE',  ( 9.641350810849047548, 17.66889113945805789, -17.94384837343789485 ) ) ;
#4592 = VECTOR ( 'NONE', #17190, 1000.000000000000000 ) ;
#4593 = CARTESIAN_POINT ( 'NONE',  ( 9.641350810849047548, 17.66889113945805789, -17.95086732675817132 ) ) ;
#4594 = DIRECTION ( 'NONE',  ( -0.5877852522924731371, 0.000000000000000000, 0.8090169943749474513 ) ) ;
#4595 = CARTESIAN_POINT ( 'NONE',  ( 172.2287565553228603, -9.999999999999996447, -3.509618943233403510 ) ) ;
#4596 = VERTEX_POINT ( 'NONE', #1528 ) ;
#4597 = DIRECTION ( 'NONE',  ( -2.698458740408365879E-16, 1.000000000000000000, 0.000000000000000000 ) ) ;
#4598 = ORIENTED_EDGE ( 'NONE', *, *, #12300, .F. ) ;
#4599 = CARTESIAN_POINT ( 'NONE',  ( 10.41412541532089620, 16.71770396712979689, -17.42473314453425814 ) ) ;
#4600 = EDGE_CURVE ( 'NONE', #12211, #6477, #20119, .T. ) ;
#4601 = CARTESIAN_POINT ( 'NONE',  ( 34.39307579391925174, -12.50091474996580487, -19.93840237985029162 ) ) ;
#4602 = CARTESIAN_POINT ( 'NONE',  ( 23.77086030874127687, -7.150112426529108944, -14.59934731766091431 ) ) ;
#4603 = ORIENTED_EDGE ( 'NONE', *, *, #14358, .F. ) ;
#4604 = FACE_OUTER_BOUND ( 'NONE', #16842, .T. ) ;
#4605 = LINE ( 'NONE', #18184, #8375 ) ;
#4606 = DIRECTION ( 'NONE',  ( 1.000000000000000000, 0.000000000000000000, 0.000000000000000000 ) ) ;
#4607 = CARTESIAN_POINT ( 'NONE',  ( 19.16431125762126442, 9.782083453288988650, -17.54400000489614087 ) ) ;
#4608 = CARTESIAN_POINT ( 'NONE',  ( 27.49606495187617128, -9.167791027049197794, -14.03786016821673677 ) ) ;
#4609 = EDGE_CURVE ( 'NONE', #7377, #12234, #15831, .T. ) ;
#4610 = ADVANCED_FACE ( 'NONE', ( #26070 ), #23160, .T. ) ;
#4612 = ORIENTED_EDGE ( 'NONE', *, *, #29568, .T. ) ;
#4611 = EDGE_CURVE ( 'NONE', #29985, #2754, #16747, .T. ) ;
#4613 = DIRECTION ( 'NONE',  ( -2.698458740408365879E-16, 1.000000000000000000, 0.000000000000000000 ) ) ;
#4614 = AXIS2_PLACEMENT_3D ( 'NONE', #2267, #16431, #20700 ) ;
#4615 = DIRECTION ( 'NONE',  ( 0.5877852522924731371, 1.586114251531760728E-16, 0.8090169943749474513 ) ) ;
#4616 = DIRECTION ( 'NONE',  ( -2.698458740408365879E-16, 1.000000000000000000, 0.000000000000000000 ) ) ;
#4617 = CARTESIAN_POINT ( 'NONE',  ( 8.000000000000012434, 3.115336682267024315, -0.3193931313915156500 ) ) ;
#4618 = CARTESIAN_POINT ( 'NONE',  ( 10.34111691064986438, 18.37243126255838988, -17.67295385331717483 ) ) ;
#4619 = DIRECTION ( 'NONE',  ( -2.698458740408365879E-16, 1.000000000000000000, 0.000000000000000000 ) ) ;
#4620 = DIRECTION ( 'NONE',  ( -1.110223024625156540E-16, 0.000000000000000000, -1.000000000000000000 ) ) ;
#4621 = ORIENTED_EDGE ( 'NONE', *, *, #24776, .F. ) ;
#4622 = CARTESIAN_POINT ( 'NONE',  ( 11.45256130090833935, 9.362448956408465861, -15.86931324879919991 ) ) ;
#4623 = CARTESIAN_POINT ( 'NONE',  ( 14.03260640687251204, 7.914523597318124715, -15.18742456358547521 ) ) ;
#4624 = CARTESIAN_POINT ( 'NONE',  ( 147.2287565553230309, -1.999999999999976241, -20.83012701892220520 ) ) ;
#4625 = PRESENTATION_STYLE_ASSIGNMENT (( #7668 ) ) ;
#4627 = ORIENTED_EDGE ( 'NONE', *, *, #5634, .T. ) ;
#4626 = CARTESIAN_POINT ( 'NONE',  ( 27.76312469413510442, -10.32446017237915648, -18.80420148706337358 ) ) ;
#4628 = ORIENTED_EDGE ( 'NONE', *, *, #25839, .F. ) ;
#4629 = DIRECTION ( 'NONE',  ( 0.9510565162951536422, 2.566386769018988816E-16, 0.3090169943749472292 ) ) ;
#4630 = CARTESIAN_POINT ( 'NONE',  ( 11.28624536866114347, 16.63080734789289750, -16.78036754607827064 ) ) ;
#4631 = EDGE_CURVE ( 'NONE', #23086, #4159, #5145, .T. ) ;
#4632 = EDGE_LOOP ( 'NONE', ( #8031, #6777, #17058, #3627 ) ) ;
#4633 = CARTESIAN_POINT ( 'NONE',  ( 33.37634376253905089, -12.42895282922877342, -19.69946502924221932 ) ) ;
#4634 = PLANE ( 'NONE',  #25901 ) ;
#4635 = VECTOR ( 'NONE', #20043, 1000.000000000000000 ) ;
#4636 = DIRECTION ( 'NONE',  ( -0.9510565162951536422, -2.566386769018988816E-16, -0.3090169943749472292 ) ) ;
#4637 = CARTESIAN_POINT ( 'NONE',  ( 26.42637521690935998, -6.951663299830703302, -19.91275981816901464 ) ) ;
#4638 = ORIENTED_EDGE ( 'NONE', *, *, #25417, .T. ) ;
#4639 = CARTESIAN_POINT ( 'NONE',  ( 4.000000000000000000, -1.549102112939128917, -0.1578953385959452616 ) ) ;
#4640 = SHAPE_REPRESENTATION_RELATIONSHIP ( 'NONE' , 'NONE' ,  #19847, #16384 ) ;
#4641 = CARTESIAN_POINT ( 'NONE',  ( 19.54522145393098498, 6.247755356217567169, -19.64858106251988801 ) ) ;
#4642 = CARTESIAN_POINT ( 'NONE',  ( 25.61980203353413543, -10.24193911033393256, -18.22380977611897990 ) ) ;
#4644 = EDGE_LOOP ( 'NONE', ( #11937, #14628, #193, #8461 ) ) ;
#4643 = EDGE_CURVE ( 'NONE', #24422, #5460, #27933, .T. ) ;
#4645 = CARTESIAN_POINT ( 'NONE',  ( 172.7287565553229740, -84.33034373659253902, 0.5000000000000029976 ) ) ;
#4646 = PLANE ( 'NONE',  #11850 ) ;
#4647 = FACE_OUTER_BOUND ( 'NONE', #20785, .T. ) ;
#4648 = DIRECTION ( 'NONE',  ( -0.8090169943749474513, -2.183098979609982436E-16, 0.5877852522924731371 ) ) ;
#4649 = CIRCLE ( 'NONE', #19739, 1.499999999999996225 ) ;
#4650 = CARTESIAN_POINT ( 'NONE',  ( 9.915538251416846194, 16.41143258624473233, -16.50493629029764264 ) ) ;
#4651 = CARTESIAN_POINT ( 'NONE',  ( 27.35978538551520245, -3.059420540688277956, -14.62525642202852971 ) ) ;
#4652 = CARTESIAN_POINT ( 'NONE',  ( 22.75707610144304383, -3.504958924507949991, -13.40925247317622571 ) ) ;
#4654 = EDGE_LOOP ( 'NONE', ( #1947, #10487, #21648, #23003 ) ) ;
#4653 = CARTESIAN_POINT ( 'NONE',  ( 33.35113679096266992, -13.31250502539155534, -20.73603153870848104 ) ) ;
#4655 = CARTESIAN_POINT ( 'NONE',  ( 133.7287565553229456, -4.999999999999982236, 3.500000000000003109 ) ) ;
#4656 = DIRECTION ( 'NONE',  ( 0.3090169943749475623, 8.338696094058001131E-17, 0.9510565162951536422 ) ) ;
#4657 = CARTESIAN_POINT ( 'NONE',  ( 162.0152310637604671, -9.999999999999998224, -17.38167787843871182 ) ) ;
#4658 = CARTESIAN_POINT ( 'NONE',  ( 14.79111372287554715, 6.954724682967856175, -19.27298399620107361 ) ) ;
#4659 = CARTESIAN_POINT ( 'NONE',  ( 156.1922820468853388, -4.999999999999976019, -4.936203717676158398 ) ) ;
#4660 = CARTESIAN_POINT ( 'NONE',  ( 10.72208662246453770, 16.62525560183325624, -15.95366392025685620 ) ) ;
#4661 = VECTOR ( 'NONE', #20378, 1000.000000000000000 ) ;
#4662 = ADVANCED_FACE ( 'NONE', ( #7137, #23312 ), #23468, .F. ) ;
#4663 = ADVANCED_FACE ( 'NONE', ( #16436 ), #2277, .T. ) ;
#4664 = ORIENTED_EDGE ( 'NONE', *, *, #30029, .F. ) ;
#4665 = CARTESIAN_POINT ( 'NONE',  ( 134.5152310637605524, -10.00000000000000533, -13.05155085951650840 ) ) ;
#4666 = DIRECTION ( 'NONE',  ( 0.3090169943749472292, 8.338696094057992503E-17, -0.9510565162951536422 ) ) ;
#4667 = PRODUCT_DEFINITION ( 'UNKNOWN', '', #11199, #27855 ) ;
#4668 = AXIS2_PLACEMENT_3D ( 'NONE', #1648, #10469, #15199 ) ;
#4669 = CARTESIAN_POINT ( 'NONE',  ( 19.91209246711783010, 5.411768277715644615, -14.29674560697521457 ) ) ;
#4670 = VERTEX_POINT ( 'NONE', #14437 ) ;
#4671 = ORIENTED_EDGE ( 'NONE', *, *, #1971, .T. ) ;
#4672 = CARTESIAN_POINT ( 'NONE',  ( 35.51409509342218485, -23.02953092745895347, -19.29936871477319826 ) ) ;
#4673 = CARTESIAN_POINT ( 'NONE',  ( 24.34695368780276681, -2.542362794815061999, -14.38654857168906886 ) ) ;
#4674 = AXIS2_PLACEMENT_3D ( 'NONE', #15161, #1457, #3153 ) ;
#4675 = CARTESIAN_POINT ( 'NONE',  ( 15.13914318552241056, 5.040073780016904870, -15.86576734333453764 ) ) ;
#4676 = CARTESIAN_POINT ( 'NONE',  ( 23.88957251509086888, -3.236156964677408876, -12.29669325917074829 ) ) ;
#4677 = ORIENTED_EDGE ( 'NONE', *, *, #19141, .T. ) ;
#4678 = DIRECTION ( 'NONE',  ( -2.698458740408365879E-16, 1.000000000000000000, 0.000000000000000000 ) ) ;
#4680 = ORIENTED_EDGE ( 'NONE', *, *, #29006, .T. ) ;
#4679 = DIRECTION ( 'NONE',  ( 1.000000000000000000, 4.440892098500622217E-16, 0.000000000000000000 ) ) ;
#4681 = DIRECTION ( 'NONE',  ( -0.8090169943749474513, -2.183098979609982436E-16, -0.5877852522924731371 ) ) ;
#4682 = AXIS2_PLACEMENT_3D ( 'NONE', #22519, #24507, #24965 ) ;
#4683 = DIRECTION ( 'NONE',  ( 0.3090169943749472292, 8.338696094057992503E-17, -0.9510565162951536422 ) ) ;
#4684 = CARTESIAN_POINT ( 'NONE',  ( 36.54006368622684420, -21.14619405898047688, -18.64381572867062076 ) ) ;
#4685 = VECTOR ( 'NONE', #3695, 1000.000000000000000 ) ;
#4686 = CARTESIAN_POINT ( 'NONE',  ( 9.641350944112486943, 17.66889052829492002, -17.91441860517739215 ) ) ;
#4687 = VERTEX_POINT ( 'NONE', #6993 ) ;
#4688 = DIRECTION ( 'NONE',  ( 0.000000000000000000, 0.000000000000000000, -1.000000000000000000 ) ) ;
#4689 = PLANE ( 'NONE',  #25519 ) ;
#4690 = CARTESIAN_POINT ( 'NONE',  ( 10.47452605456472696, 16.44069893626776491, -17.33376834041267145 ) ) ;
#4691 = CARTESIAN_POINT ( 'NONE',  ( 2.500000000000000444, -2.357898499370430834, 3.469446951953614189E-15 ) ) ;
#4692 = CARTESIAN_POINT ( 'NONE',  ( 167.0152310637604671, -9.999999999999998224, -6.958068083716895558 ) ) ;
#4693 = ADVANCED_FACE ( 'NONE', ( #2714 ), #2872, .F. ) ;
#4694 = ADVANCED_FACE ( 'NONE', ( #2425 ), #11702, .T. ) ;
#4695 = ORIENTED_EDGE ( 'NONE', *, *, #28646, .T. ) ;
#4696 = CARTESIAN_POINT ( 'NONE',  ( 149.7287565553229740, -10.00000000000000178, -7.839745962155603820 ) ) ;
#4697 = EDGE_CURVE ( 'NONE', #23239, #19711, #275, .T. ) ;
#4698 = FACE_OUTER_BOUND ( 'NONE', #18606, .T. ) ;
#4699 = EDGE_CURVE ( 'NONE', #24045, #23305, #21471, .T. ) ;
#4700 = ORIENTED_EDGE ( 'NONE', *, *, #14059, .F. ) ;
#4701 = FACE_OUTER_BOUND ( 'NONE', #27171, .T. ) ;
#4702 = ORIENTED_EDGE ( 'NONE', *, *, #29927, .T. ) ;
#4703 = CARTESIAN_POINT ( 'NONE',  ( 9.667620158929956631, 16.22851557400931455, -17.88520075955172572 ) ) ;
#4704 = CARTESIAN_POINT ( 'NONE',  ( 19.89307947303188229, -2.966738011908462092, -16.73278295482091949 ) ) ;
#4705 = CARTESIAN_POINT ( 'NONE',  ( 20.12919692000023986, -2.949910412001375715, -15.69023992059449846 ) ) ;
#4706 = VERTEX_POINT ( 'NONE', #28236 ) ;
#4707 = CARTESIAN_POINT ( 'NONE',  ( 19.54522145393098498, 6.247755356217567169, -19.64858106251988801 ) ) ;
#4708 = AXIS2_PLACEMENT_3D ( 'NONE', #17140, #9953, #14831 ) ;
#4709 = CARTESIAN_POINT ( 'NONE',  ( 23.64023604348281893, -5.000000000000011546, -72.75716528596417731 ) ) ;
#4710 = CARTESIAN_POINT ( 'NONE',  ( -2.309976723937613219, 7.903938623646876493, -0.1306530452038166257 ) ) ;
#4711 = LINE ( 'NONE', #19052, #14228 ) ;
#4712 = AXIS2_PLACEMENT_3D ( 'NONE', #30144, #11897, #4597 ) ;
#4713 = CARTESIAN_POINT ( 'NONE',  ( 26.31132954256896639, -3.159408024760113509, -14.81636702655834803 ) ) ;
#4714 = EDGE_LOOP ( 'NONE', ( #6279, #5406, #28251, #28461 ) ) ;
#4715 = DIRECTION ( 'NONE',  ( -2.698458740408365879E-16, 1.000000000000000000, 0.000000000000000000 ) ) ;
#4716 = DIRECTION ( 'NONE',  ( -0.7071067811865460184, -0.7071067811865490160, -0.000000000000000000 ) ) ;
#4717 = CARTESIAN_POINT ( 'NONE',  ( 2.500000000000000444, 0.000000000000000000, 0.000000000000000000 ) ) ;
#4718 = CYLINDRICAL_SURFACE ( 'NONE', #19500, 139.8897274573438096 ) ;
#4719 = CARTESIAN_POINT ( 'NONE',  ( 138.6922820468854525, -10.00000000000000533, -9.266330736598359152 ) ) ;
#4720 = CARTESIAN_POINT ( 'NONE',  ( 2.500000000000000444, 1.178949249685215417, -2.042000000000002036 ) ) ;
#4721 = DIRECTION ( 'NONE',  ( 0.5877852522924731371, 0.000000000000000000, 0.8090169943749474513 ) ) ;
#4722 = FACE_OUTER_BOUND ( 'NONE', #2027, .T. ) ;
#4723 = VERTEX_POINT ( 'NONE', #18433 ) ;
#4724 = CARTESIAN_POINT ( 'NONE',  ( 11.18347232286468440, 9.276624323996792043, -17.25832042385608389 ) ) ;
#4725 = ORIENTED_EDGE ( 'NONE', *, *, #15479, .T. ) ;
#4726 = LINE ( 'NONE', #6430, #14374 ) ;
#4727 = VECTOR ( 'NONE', #28775, 1000.000000000000000 ) ;
#4728 = CARTESIAN_POINT ( 'NONE',  ( 19.91209246711783010, 5.411768277715644615, -14.29674560697521457 ) ) ;
#4729 = CARTESIAN_POINT ( 'NONE',  ( 11.29637638519941589, 16.58434521464408817, -16.77617801436024081 ) ) ;
#4730 = DIRECTION ( 'NONE',  ( 0.9510565162951536422, 2.566386769018988816E-16, 0.3090169943749472292 ) ) ;
#4731 = ORIENTED_EDGE ( 'NONE', *, *, #18338, .F. ) ;
#4732 = ADVANCED_FACE ( 'NONE', ( #14284 ), #7290, .T. ) ;
#4733 = ORIENTED_EDGE ( 'NONE', *, *, #17446, .F. ) ;
#4734 = VECTOR ( 'NONE', #1310, 1000.000000000000000 ) ;
#4735 = CARTESIAN_POINT ( 'NONE',  ( 9.917205744531459644, 16.40378525026516243, -16.50423678068149869 ) ) ;
#4736 = CARTESIAN_POINT ( 'NONE',  ( 151.1922820468854241, -1.999999999999975353, -19.40354224447947828 ) ) ;
#4737 = EDGE_CURVE ( 'NONE', #26487, #5681, #21316, .T. ) ;
#4738 = CARTESIAN_POINT ( 'NONE',  ( 9.917965570771830386, 16.40030059027150600, -16.50392256580263606 ) ) ;
#4739 = LINE ( 'NONE', #23069, #7843 ) ;
#4740 = LINE ( 'NONE', #23823, #13990 ) ;
#4741 = EDGE_CURVE ( 'NONE', #15488, #1679, #4453, .T. ) ;
#4742 = ORIENTED_EDGE ( 'NONE', *, *, #27938, .F. ) ;
#4743 = CARTESIAN_POINT ( 'NONE',  ( -24.99999999999999289, 60.00000000000000711, -25.00000000000000000 ) ) ;
#4744 = EDGE_LOOP ( 'NONE', ( #11353, #13537, #14566, #10646, #473 ) ) ;
#4745 = CARTESIAN_POINT ( 'NONE',  ( 10.47195275365909595, 16.45250042224058618, -17.33483252618548676 ) ) ;
#4746 = ORIENTED_EDGE ( 'NONE', *, *, #13724, .F. ) ;
#4747 = CARTESIAN_POINT ( 'NONE',  ( 36.53271160917758209, -22.11316507130252873, -18.90714217169671230 ) ) ;
#4748 = CARTESIAN_POINT ( 'NONE',  ( 23.29338531092689735, -7.078548041224526521, -17.51562821661096336 ) ) ;
#4749 = ORIENTED_EDGE ( 'NONE', *, *, #9869, .F. ) ;
#4750 = DIRECTION ( 'NONE',  ( -1.000000000000000000, -1.226925503391459091E-16, 0.000000000000000000 ) ) ;
#4751 = ORIENTED_EDGE ( 'NONE', *, *, #9754, .F. ) ;
#4752 = CARTESIAN_POINT ( 'NONE',  ( 157.0152310637604671, -4.999999999999975131, -8.721423840594312082 ) ) ;
#4753 = DIRECTION ( 'NONE',  ( 0.000000000000000000, 0.000000000000000000, -1.000000000000000000 ) ) ;
#4754 = CARTESIAN_POINT ( 'NONE',  ( 19.52759782329482263, 6.073010510103808990, -18.47256557099433394 ) ) ;
#4755 = CARTESIAN_POINT ( 'NONE',  ( 25.90061519764796572, -9.523157571424881951, -17.57609359838447816 ) ) ;
#4756 = VECTOR ( 'NONE', #10057, 1000.000000000000000 ) ;
#4757 = ORIENTED_EDGE ( 'NONE', *, *, #18036, .T. ) ;
#4758 = FACE_BOUND ( 'NONE', #25990, .T. ) ;
#4759 = AXIS2_PLACEMENT_3D ( 'NONE', #12061, #27989, #5050 ) ;
#4760 = DIRECTION ( 'NONE',  ( 1.000000000000000000, -0.000000000000000000, 0.000000000000000000 ) ) ;
#4761 = VECTOR ( 'NONE', #23688, 1000.000000000000000 ) ;
#4762 = DIRECTION ( 'NONE',  ( 0.000000000000000000, 1.000000000000000000, -1.471414886128461471E-15 ) ) ;
#4763 = DIRECTION ( 'NONE',  ( -2.698458740408365879E-16, 1.000000000000000000, 0.000000000000000000 ) ) ;
#4764 = CARTESIAN_POINT ( 'NONE',  ( 10.72132679622416696, 16.62874026182691267, -15.95397813513572061 ) ) ;
#4765 = DIRECTION ( 'NONE',  ( -0.9510565162951536422, -2.566386769018988816E-16, -0.3090169943749472292 ) ) ;
#4766 = ORIENTED_EDGE ( 'NONE', *, *, #5848, .F. ) ;
#4767 = CARTESIAN_POINT ( 'NONE',  ( -8.000000000000000000, 4.618802153517001408, -5.000000000000000888 ) ) ;
#4768 = ORIENTED_EDGE ( 'NONE', *, *, #21340, .F. ) ;
#4769 = CARTESIAN_POINT ( 'NONE',  ( 9.916637298967875935, 16.40639221407973380, -16.50447193873893781 ) ) ;
#4770 = ORIENTED_EDGE ( 'NONE', *, *, #18063, .F. ) ;
#4771 = EDGE_CURVE ( 'NONE', #20749, #25811, #19033, .T. ) ;
#4772 = ADVANCED_FACE ( 'NONE', ( #4994 ), #25457, .T. ) ;
#4773 = AXIS2_PLACEMENT_3D ( 'NONE', #8021, #15645, #24977 ) ;
#4774 = CARTESIAN_POINT ( 'NONE',  ( 27.20859382114707614, -12.49599901988731077, -15.99530080614381511 ) ) ;
#4775 = DIRECTION ( 'NONE',  ( 1.110223024625156540E-16, 2.995891024602366092E-32, 1.000000000000000000 ) ) ;
#4776 = DIRECTION ( 'NONE',  ( 1.000000000000000000, 0.000000000000000000, 0.000000000000000000 ) ) ;
#4777 = EDGE_CURVE ( 'NONE', #28404, #26171, #3327, .T. ) ;
#4778 = ORIENTED_EDGE ( 'NONE', *, *, #10769, .T. ) ;
#4779 = CARTESIAN_POINT ( 'NONE',  ( 24.62590367393082502, -9.567571807129121808, -15.85044010117769098 ) ) ;
#4780 = VERTEX_POINT ( 'NONE', #14882 ) ;
#4781 = CARTESIAN_POINT ( 'NONE',  ( 180.7287565553229456, -9.999999999999968026, 0.5000000000000029976 ) ) ;
#4782 = ADVANCED_FACE ( 'NONE', ( #15039 ), #5910, .T. ) ;
#4783 = CARTESIAN_POINT ( 'NONE',  ( 11.05542614047498873, 17.68937375096277265, -17.90480922774079175 ) ) ;
#4784 = AXIS2_PLACEMENT_3D ( 'NONE', #6748, #22623, #16038 ) ;
#4785 = CARTESIAN_POINT ( 'NONE',  ( 33.29128644620831778, -11.81988703332123691, -18.18190324972602667 ) ) ;
#4786 = CARTESIAN_POINT ( 'NONE',  ( 17.17204249742301059, 10.23148044644768362, -15.96021614775051667 ) ) ;
#4787 = CARTESIAN_POINT ( 'NONE',  ( 146.1922820468854525, -10.00000000000000178, -28.06379628232387446 ) ) ;
#4788 = CARTESIAN_POINT ( 'NONE',  ( 27.97271982581976957, -5.335442005784750918, -18.83880583778296725 ) ) ;
#4789 = ORIENTED_EDGE ( 'NONE', *, *, #24738, .F. ) ;
#4790 = CARTESIAN_POINT ( 'NONE',  ( 4.000000000000000000, -1.933795701539638534, -0.2488376576623040348 ) ) ;
#4791 = CARTESIAN_POINT ( 'NONE',  ( 22.84118038848623655, 1.850029439873439152, -18.07216660426987431 ) ) ;
#4792 = CARTESIAN_POINT ( 'NONE',  ( 18.71812633715165575, 6.658065805436550910, -18.41436643113302551 ) ) ;
#4793 = ORIENTED_EDGE ( 'NONE', *, *, #26532, .T. ) ;
#4794 = DIRECTION ( 'NONE',  ( 0.9510565162951536422, 0.000000000000000000, -0.3090169943749475623 ) ) ;
#4795 = VECTOR ( 'NONE', #3965, 1000.000000000000000 ) ;
#4796 = CARTESIAN_POINT ( 'NONE',  ( 139.5152310637605808, -4.999999999999980460, -21.71180489736090991 ) ) ;
#4797 = FACE_OUTER_BOUND ( 'NONE', #20873, .T. ) ;
#4798 = AXIS2_PLACEMENT_3D ( 'NONE', #28549, #7601, #29008 ) ;
#4799 = LINE ( 'NONE', #6390, #8802 ) ;
#4800 = CARTESIAN_POINT ( 'NONE',  ( 133.6922820468854241, -10.00000000000000711, -26.58683881228715506 ) ) ;
#4801 = CARTESIAN_POINT ( 'NONE',  ( 9.916118674515717046, 16.40877069192658055, -16.50468880802031890 ) ) ;
#4802 = VECTOR ( 'NONE', #24698, 1000.000000000000000 ) ;
#4803 = CARTESIAN_POINT ( 'NONE',  ( 27.85231147893869874, -3.451530096863186792, -17.11803778117090857 ) ) ;
#4804 = CARTESIAN_POINT ( 'NONE',  ( 18.75392633456350922, 0.8452085672475394551, -14.97946080469353447 ) ) ;
#4805 = CARTESIAN_POINT ( 'NONE',  ( 30.78206665311622459, -10.11802168058175511, -15.10569088962643036 ) ) ;
#4806 = DIRECTION ( 'NONE',  ( -0.9510565162951536422, -2.566386769018988323E-16, 0.3090169943749475623 ) ) ;
#4807 = CARTESIAN_POINT ( 'NONE',  ( 36.54859390953723874, -22.18451583373416014, -15.00000000000000000 ) ) ;
#4808 = CARTESIAN_POINT ( 'NONE',  ( 154.5152310637605240, -10.00000000000000000, -11.28819510263909542 ) ) ;
#4809 = DIRECTION ( 'NONE',  ( -1.000000000000000000, 0.000000000000000000, -0.000000000000000000 ) ) ;
#4810 = CARTESIAN_POINT ( 'NONE',  ( 14.17177033308128031, 6.273687421093853800, -17.36430109743762173 ) ) ;
#4811 = ORIENTED_EDGE ( 'NONE', *, *, #17073, .T. ) ;
#4812 = DIRECTION ( 'NONE',  ( -0.7071067811865501263, -0.7071067811865449082, 9.966407208441821704E-16 ) ) ;
#4813 = ADVANCED_FACE ( 'NONE', ( #22080 ), #1183, .F. ) ;
#4814 = CARTESIAN_POINT ( 'NONE',  ( 10.48326151898216452, 17.72053796952357985, -16.40639007392780258 ) ) ;
#4815 = ORIENTED_EDGE ( 'NONE', *, *, #14440, .F. ) ;
#4816 = DIRECTION ( 'NONE',  ( 1.000000000000000000, 2.698458740408365879E-16, -1.110223024625156540E-16 ) ) ;
#4817 = CYLINDRICAL_SURFACE ( 'NONE', #7375, 4.250000000000003553 ) ;
#4818 = CARTESIAN_POINT ( 'NONE',  ( 18.55171814111300321, 6.637122934506423988, -19.73184648383247364 ) ) ;
#4819 = ORIENTED_EDGE ( 'NONE', *, *, #18035, .T. ) ;
#4820 = CARTESIAN_POINT ( 'NONE',  ( 30.38377115645388571, -7.011354780429720712, -16.65419678813778503 ) ) ;
#4821 = ORIENTED_EDGE ( 'NONE', *, *, #25575, .F. ) ;
#4822 = CARTESIAN_POINT ( 'NONE',  ( 33.24414211882076842, -12.83183464011245967, -20.70368961610576264 ) ) ;
#4823 = VERTEX_POINT ( 'NONE', #10164 ) ;
#4824 = VECTOR ( 'NONE', #10131, 1000.000000000000000 ) ;
#4825 = CARTESIAN_POINT ( 'NONE',  ( 20.97270766892557603, 0.7925772802953747753, -14.00178974354743033 ) ) ;
#4826 = CARTESIAN_POINT ( 'NONE',  ( 20.59924605810746101, 4.422246688411098248, -17.72709849028201035 ) ) ;
#4827 = VECTOR ( 'NONE', #6875, 1000.000000000000000 ) ;
#4828 = CARTESIAN_POINT ( 'NONE',  ( 26.40217035250003974, -9.511505991202637844, -18.98702918838447573 ) ) ;
#4829 = ORIENTED_EDGE ( 'NONE', *, *, #15719, .F. ) ;
#4830 = CARTESIAN_POINT ( 'NONE',  ( -7.999999999999994671, 3.115336682267016766, -4.680606868608490956 ) ) ;
#4831 = ORIENTED_EDGE ( 'NONE', *, *, #7603, .F. ) ;
#4832 = EDGE_CURVE ( 'NONE', #17767, #27247, #22973, .T. ) ;
#4833 = CARTESIAN_POINT ( 'NONE',  ( 162.0152310637605240, -1.999999999999971800, -34.70218595412750773 ) ) ;
#4834 = ORIENTED_EDGE ( 'NONE', *, *, #16936, .T. ) ;
#4835 = CARTESIAN_POINT ( 'NONE',  ( 174.5152310637604671, -9.999999999999994671, -19.94844914048349693 ) ) ;
#4836 = PLANE ( 'NONE',  #19991 ) ;
#4837 = CARTESIAN_POINT ( 'NONE',  ( 36.29797175594614345, -20.05860325589622661, -19.47188034632657150 ) ) ;
#4838 = CONICAL_SURFACE ( 'NONE', #26791, 4.000000000000003553, 1.047197551196597853 ) ;
#4839 = CARTESIAN_POINT ( 'NONE',  ( 12.75639466810640776, 7.625977817552541005, -14.92582393630036108 ) ) ;
#4840 = EDGE_LOOP ( 'NONE', ( #13329, #13034 ) ) ;
#4841 = DIRECTION ( 'NONE',  ( -0.8090169943749474513, -2.183098979609982436E-16, -0.5877852522924731371 ) ) ;
#4842 = CARTESIAN_POINT ( 'NONE',  ( 138.6922820468854525, -10.00000000000000533, -35.24709285013155835 ) ) ;
#4843 = CARTESIAN_POINT ( 'NONE',  ( 10.47262648896379922, 16.44941058625191133, -17.33455387760982447 ) ) ;
#4844 = CARTESIAN_POINT ( 'NONE',  ( 0.000000000000000000, 0.000000000000000000, 4.999999999999998224 ) ) ;
#4845 = VECTOR ( 'NONE', #26869, 1000.000000000000000 ) ;
#4846 = CARTESIAN_POINT ( 'NONE',  ( 163.6922820468853388, -9.999999999999998224, -17.92658477444275889 ) ) ;
#4847 = ORIENTED_EDGE ( 'NONE', *, *, #2007, .F. ) ;
#4848 = FACE_OUTER_BOUND ( 'NONE', #24730, .T. ) ;
#4849 = DIRECTION ( 'NONE',  ( 0.000000000000000000, 0.000000000000000000, 1.000000000000000000 ) ) ;
#4850 = CARTESIAN_POINT ( 'NONE',  ( 0.000000000000000000, 0.000000000000000000, 2.550000000000000266 ) ) ;
#4851 = ORIENTED_EDGE ( 'NONE', *, *, #5434, .T. ) ;
#4852 = CARTESIAN_POINT ( 'NONE',  ( 9.669898452045105230, 16.21806703136846295, -17.88423646254436861 ) ) ;
#4853 = ORIENTED_EDGE ( 'NONE', *, *, #15755, .T. ) ;
#4854 = CARTESIAN_POINT ( 'NONE',  ( 25.86774690167791135, -3.337865513817628749, -16.68124922160397006 ) ) ;
#4855 = CARTESIAN_POINT ( 'NONE',  ( 16.37314578033188894, 3.237113944496374351, -18.86778596048347723 ) ) ;
#4856 = CARTESIAN_POINT ( 'NONE',  ( 151.1922820468853956, -4.999999999999976907, -10.74328820663507678 ) ) ;
#4857 = CARTESIAN_POINT ( 'NONE',  ( 177.2287565553228887, -9.999999999999994671, -20.83012701892220520 ) ) ;
#4859 = PLANE ( 'NONE',  #9835 ) ;
#4858 = AXIS2_PLACEMENT_3D ( 'NONE', #6907, #11763, #188 ) ;
#4860 = AXIS2_PLACEMENT_3D ( 'NONE', #27661, #6428, #15717 ) ;
#4861 = CARTESIAN_POINT ( 'NONE',  ( 25.97256211245905533, -8.171536508395311316, -18.54953510021574559 ) ) ;
#4862 = VECTOR ( 'NONE', #27059, 1000.000000000000000 ) ;
#4863 = DIRECTION ( 'NONE',  ( 1.110223024625156540E-16, 2.995891024602366092E-32, 1.000000000000000000 ) ) ;
#4864 = EDGE_CURVE ( 'NONE', #24083, #13474, #12757, .T. ) ;
#4865 = DIRECTION ( 'NONE',  ( -0.9510565162951536422, -2.566386769018988323E-16, 0.3090169943749475623 ) ) ;
#4866 = ADVANCED_FACE ( 'NONE', ( #21621 ), #7585, .T. ) ;
#4867 = DIRECTION ( 'NONE',  ( 1.000000000000000000, 0.000000000000000000, -0.000000000000000000 ) ) ;
#4868 = EDGE_CURVE ( 'NONE', #26851, #26883, #19477, .T. ) ;
#4869 = CARTESIAN_POINT ( 'NONE',  ( 75.00000000000000000, 0.000000000000000000, 0.000000000000000000 ) ) ;
#4870 = CARTESIAN_POINT ( 'NONE',  ( 139.7287565553230309, -1.999999999999978684, -7.839745962155603820 ) ) ;
#4871 = CARTESIAN_POINT ( 'NONE',  ( 10.47151541139924547, 16.45450612959241354, -17.33501744001014444 ) ) ;
#4872 = VECTOR ( 'NONE', #26962, 1000.000000000000000 ) ;
#4873 = CARTESIAN_POINT ( 'NONE',  ( 35.54859390954303677, -22.18451583373416014, -15.55638201429745848 ) ) ;
#4874 = CARTESIAN_POINT ( 'NONE',  ( 33.57712230886461668, -13.32773824946660923, -19.76201999124979736 ) ) ;
#4875 = VERTEX_POINT ( 'NONE', #29140 ) ;
#4876 = CARTESIAN_POINT ( 'NONE',  ( 13.65148492087865151, 7.746099194123166498, -15.49118511517110619 ) ) ;
#4877 = ORIENTED_EDGE ( 'NONE', *, *, #22315, .T. ) ;
#4878 = CARTESIAN_POINT ( 'NONE',  ( 133.6922820468854241, -1.999999999999980904, -6.413161187712875133 ) ) ;
#4879 = CARTESIAN_POINT ( 'NONE',  ( 19.50856600871340873, -1.908691058934758100, -18.90332006808282728 ) ) ;
#4880 = CARTESIAN_POINT ( 'NONE',  ( 11.27378865171844602, 16.68793543965420767, -16.78556983912737621 ) ) ;
#4881 = FACE_OUTER_BOUND ( 'NONE', #25539, .T. ) ;
#4882 = ORIENTED_EDGE ( 'NONE', *, *, #25973, .T. ) ;
#4883 = AXIS2_PLACEMENT_3D ( 'NONE', #3030, #14287, #2875 ) ;
#4884 = VERTEX_POINT ( 'NONE', #5605 ) ;
#4885 = CARTESIAN_POINT ( 'NONE',  ( 9.649959050778257108, 17.62941265384766254, -17.56860460898032628 ) ) ;
#4886 = DIRECTION ( 'NONE',  ( 1.000000000000000000, 2.698458740408365879E-16, -1.110223024625156540E-16 ) ) ;
#4887 = VECTOR ( 'NONE', #13790, 1000.000000000000000 ) ;
#4888 = CARTESIAN_POINT ( 'NONE',  ( 9.776119957569173735, 17.05082265352876547, -16.72288386497739765 ) ) ;
#4889 = DIRECTION ( 'NONE',  ( 0.5877852522924731371, 0.000000000000000000, 0.8090169943749474513 ) ) ;
#4890 = CARTESIAN_POINT ( 'NONE',  ( 0.3263565795980564732, -4.430380094434313243, -2.201519936624962259 ) ) ;
#4891 = ORIENTED_EDGE ( 'NONE', *, *, #2008, .F. ) ;
#4892 = CARTESIAN_POINT ( 'NONE',  ( 172.0152310637604955, -9.999999999999994671, -34.70218595412750773 ) ) ;
#4893 = ORIENTED_EDGE ( 'NONE', *, *, #13107, .F. ) ;
#4894 = CARTESIAN_POINT ( 'NONE',  ( 11.12037835888041393, 13.47873794165536410, -17.06668569338069830 ) ) ;
#4895 = VERTEX_POINT ( 'NONE', #8177 ) ;
#4896 = CARTESIAN_POINT ( 'NONE',  ( 33.94449656094377588, -11.59990251341361933, -20.77871222707083376 ) ) ;
#4897 = CARTESIAN_POINT ( 'NONE',  ( 15.30534275580653869, 10.60631812597827839, -15.20037037882373987 ) ) ;
#4898 = CARTESIAN_POINT ( 'NONE',  ( 24.81358459371387326, -5.676498915796258871, -18.90393244824272756 ) ) ;
#4899 = ORIENTED_EDGE ( 'NONE', *, *, #9409, .T. ) ;
#4900 = DIRECTION ( 'NONE',  ( -0.000000000000000000, 0.000000000000000000, 1.000000000000000000 ) ) ;
#4901 = CARTESIAN_POINT ( 'NONE',  ( 34.36632712588347260, -12.38074715364594347, -19.93031689919964222 ) ) ;
#4902 = AXIS2_PLACEMENT_3D ( 'NONE', #24536, #8346, #27006 ) ;
#4903 = CARTESIAN_POINT ( 'NONE',  ( 15.96850636225579656, 5.405031054132949819, -14.95518105802344344 ) ) ;
#4904 = CIRCLE ( 'NONE', #20492, 2.000000000000000000 ) ;
#4905 = CARTESIAN_POINT ( 'NONE',  ( 14.34656430690936624, 9.113120221615268690, -15.03016663717492563 ) ) ;
#4906 = ORIENTED_EDGE ( 'NONE', *, *, #20615, .T. ) ;
#4907 = DIRECTION ( 'NONE',  ( -0.5877852522924731371, -1.586114251531760235E-16, 0.8090169943749474513 ) ) ;
#4908 = EDGE_CURVE ( 'NONE', #13418, #11002, #28848, .T. ) ;
#4909 = EDGE_CURVE ( 'NONE', #27640, #17911, #17489, .T. ) ;
#4910 = ADVANCED_FACE ( 'NONE', ( #26840 ), #16889, .F. ) ;
#4911 = ORIENTED_EDGE ( 'NONE', *, *, #9408, .F. ) ;
#4912 = DIRECTION ( 'NONE',  ( 0.3090169943749475623, 8.338696094058001131E-17, 0.9510565162951536422 ) ) ;
#4913 = CARTESIAN_POINT ( 'NONE',  ( 98.87704821043671188, -4.999999999999990230, -71.83838056851863030 ) ) ;
#4914 = CARTESIAN_POINT ( 'NONE',  ( -13.00000000000000178, -2.870178842070716726E-15, 23.00000000000000000 ) ) ;
#4915 = UNCERTAINTY_MEASURE_WITH_UNIT (LENGTH_MEASURE( 1.000000000000000082E-05 ), #25066, 'distance_accuracy_value', 'NONE');
#4916 = CARTESIAN_POINT ( 'NONE',  ( 10.74108227847380448, 16.53813910199176007, -15.94580854828543437 ) ) ;
#4918 = AXIS2_PLACEMENT_3D ( 'NONE', #23936, #3027, #22224 ) ;
#4917 = CARTESIAN_POINT ( 'NONE',  ( 154.7287565553229172, -10.00000000000000178, -16.50000000000000000 ) ) ;
#4919 = ORIENTED_EDGE ( 'NONE', *, *, #13655, .T. ) ;
#4920 = CARTESIAN_POINT ( 'NONE',  ( 180.7287565553229456, -3.999999999999989786, -33.50000000000000000 ) ) ;
#4921 = ORIENTED_EDGE ( 'NONE', *, *, #12725, .T. ) ;
#4922 = AXIS2_PLACEMENT_3D ( 'NONE', #18520, #21110, #18818 ) ;
#4923 = CARTESIAN_POINT ( 'NONE',  ( 9.915973561396301150, 16.40943619918981256, -16.50475030878699556 ) ) ;
#4924 = EDGE_LOOP ( 'NONE', ( #15642, #20260, #22893, #5865 ) ) ;
#4925 = CARTESIAN_POINT ( 'NONE',  ( 9.670405002872021427, 16.21574392470601467, -17.88402698595844598 ) ) ;
#4926 = CARTESIAN_POINT ( 'NONE',  ( 18.89276694006714052, 5.271756288042509730, -14.92826338805148190 ) ) ;
#4927 = DIRECTION ( 'NONE',  ( 0.000000000000000000, 0.000000000000000000, 1.000000000000000000 ) ) ;
#4928 = DIRECTION ( 'NONE',  ( -0.000000000000000000, 0.000000000000000000, 1.000000000000000000 ) ) ;
#4929 = CARTESIAN_POINT ( 'NONE',  ( 27.01132674553606350, -11.00696853675122711, -18.49859303458091730 ) ) ;
#4930 = EDGE_LOOP ( 'NONE', ( #21403, #17413, #15713, #27252 ) ) ;
#4931 = DIRECTION ( 'NONE',  ( -0.8090169943749474513, -2.183098979609982436E-16, -0.5877852522924731371 ) ) ;
#4932 = CARTESIAN_POINT ( 'NONE',  ( 11.26126983089308098, 16.74534834773793790, -16.79273533431442900 ) ) ;
#4933 = VERTEX_POINT ( 'NONE', #10316 ) ;
#4934 = CARTESIAN_POINT ( 'NONE',  ( 35.34747194004189907, -20.28098136206135749, -19.25482875754748946 ) ) ;
#4935 = CARTESIAN_POINT ( 'NONE',  ( 2.500000000000000444, 2.357898499370430834, -3.469446951953614189E-15 ) ) ;
#4936 = PLANE ( 'NONE',  #13038 ) ;
#4937 = CARTESIAN_POINT ( 'NONE',  ( 26.79503139269368006, -8.611318205148688065, -11.94858980718629304 ) ) ;
#4938 = VERTEX_POINT ( 'NONE', #24525 ) ;
#4939 = DIRECTION ( 'NONE',  ( -0.5877852522924731371, -1.586114251531760235E-16, 0.8090169943749474513 ) ) ;
#4940 =( LENGTH_UNIT ( ) NAMED_UNIT ( * ) SI_UNIT ( .MILLI., .METRE. ) );
#4941 = CARTESIAN_POINT ( 'NONE',  ( 18.23802153489769751, 0.9697156596711644649, -18.35043786425562828 ) ) ;
#4942 = CARTESIAN_POINT ( 'NONE',  ( 16.58324305800299925, 4.586402732284541095, -18.38077023430394163 ) ) ;
#4943 = VERTEX_POINT ( 'NONE', #3618 ) ;
#4944 = ORIENTED_EDGE ( 'NONE', *, *, #5929, .F. ) ;
#4945 = CIRCLE ( 'NONE', #6854, 13.00000000000000178 ) ;
#4946 = DIRECTION ( 'NONE',  ( 0.3090169943749475623, 8.338696094058001131E-17, 0.9510565162951536422 ) ) ;
#4947 = VECTOR ( 'NONE', #27878, 999.9999999999998863 ) ;
#4948 = EDGE_CURVE ( 'NONE', #11956, #19044, #7886, .T. ) ;
#4949 = EDGE_CURVE ( 'NONE', #6425, #27841, #26219, .T. ) ;
#4950 = EDGE_CURVE ( 'NONE', #1366, #22270, #24228, .T. ) ;
#4951 = CARTESIAN_POINT ( 'NONE',  ( 136.1922820468854241, -4.999999999999980460, -4.936203717676158398 ) ) ;
#4952 = ADVANCED_FACE ( 'NONE', ( #24078 ), #3179, .T. ) ;
#4953 = LINE ( 'NONE', #18833, #25633 ) ;
#4954 = CARTESIAN_POINT ( 'NONE',  ( 156.1922820468854241, -1.999999999999974021, -30.91696583120936026 ) ) ;
#4955 = DIRECTION ( 'NONE',  ( 0.5877852522924731371, 0.000000000000000000, 0.8090169943749474513 ) ) ;
#4956 = CARTESIAN_POINT ( 'NONE',  ( 9.916953853453376766, 16.40494045485788632, -16.50434094533541085 ) ) ;
#4957 = CARTESIAN_POINT ( 'NONE',  ( 25.48002462322397577, -3.608900787083736184, -12.74538502395823691 ) ) ;
#4958 = CARTESIAN_POINT ( 'NONE',  ( 24.47846259200217034, 0.2319951948203725633, -15.89054235832688278 ) ) ;
#4960 = VERTEX_POINT ( 'NONE', #26522 ) ;
#4959 = CARTESIAN_POINT ( 'NONE',  ( 36.45689639539443050, -22.77256747621617095, -19.95163700058902734 ) ) ;
#4961 = FACE_OUTER_BOUND ( 'NONE', #17966, .T. ) ;
#4962 = CARTESIAN_POINT ( 'NONE',  ( 12.93612603019711571, 8.763434079353435990, -14.78257486846209545 ) ) ;
#4963 = DIRECTION ( 'NONE',  ( -2.698458740408365879E-16, 1.000000000000000000, 0.000000000000000000 ) ) ;
#4964 = DIRECTION ( 'NONE',  ( 0.5877852522924731371, 1.586114251531760728E-16, -0.8090169943749474513 ) ) ;
#4965 = CARTESIAN_POINT ( 'NONE',  ( 17.69365662292968366, 10.27476822432933545, -17.01437286930526227 ) ) ;
#4966 = CARTESIAN_POINT ( 'NONE',  ( 139.5152310637605808, -10.00000000000000533, -2.627941064794695691 ) ) ;
#4967 = CARTESIAN_POINT ( 'NONE',  ( 10.70471194873291410, 16.70493807032227451, -15.96226385378574264 ) ) ;
#4968 = ORIENTED_EDGE ( 'NONE', *, *, #28836, .T. ) ;
#4969 = DIRECTION ( 'NONE',  ( -2.698458740408365879E-16, 1.000000000000000000, 0.000000000000000000 ) ) ;
#4970 = CARTESIAN_POINT ( 'NONE',  ( 133.7287565553229456, -9.999999999999980460, 0.5000000000000029976 ) ) ;
#4971 = CARTESIAN_POINT ( 'NONE',  ( 16.79143122783437292, 7.330551994622505063, -14.54187356113185103 ) ) ;
#4972 = ORIENTED_EDGE ( 'NONE', *, *, #11405, .T. ) ;
#4973 = CARTESIAN_POINT ( 'NONE',  ( 13.62270618888621776, 10.12723052195839024, -14.35540206260209573 ) ) ;
#4974 = ORIENTED_EDGE ( 'NONE', *, *, #489, .T. ) ;
#4975 = CARTESIAN_POINT ( 'NONE',  ( 33.38708106686501509, -12.47399286361455850, -19.70456970583452616 ) ) ;
#4976 = CARTESIAN_POINT ( 'NONE',  ( 23.02024704684396283, -2.230829994151436679, -18.49515006079944612 ) ) ;
#4977 = AXIS2_PLACEMENT_3D ( 'NONE', #26476, #3276, #10264 ) ;
#4978 = CARTESIAN_POINT ( 'NONE',  ( 21.97327598498023704, 3.176719406474355800, -15.71098195781089046 ) ) ;
#4979 = CARTESIAN_POINT ( 'NONE',  ( 28.61171173311277016, -11.12923776720465874, -18.00325214586577971 ) ) ;
#4980 = EDGE_CURVE ( 'NONE', #9455, #314, #8027, .T. ) ;
#4981 = VECTOR ( 'NONE', #16040, 1000.000000000000000 ) ;
#4982 = ORIENTED_EDGE ( 'NONE', *, *, #4572, .T. ) ;
#4983 = EDGE_CURVE ( 'NONE', #11457, #12771, #22385, .T. ) ;
#4984 = DIRECTION ( 'NONE',  ( -0.9510565162951536422, 0.000000000000000000, -0.3090169943749472292 ) ) ;
#4985 = EDGE_CURVE ( 'NONE', #13044, #8301, #27456, .T. ) ;
#4986 = CARTESIAN_POINT ( 'NONE',  ( -20.00000000000017053, 34.64101615137744972, 4.999999999999998224 ) ) ;
#4987 = ORIENTED_EDGE ( 'NONE', *, *, #28241, .T. ) ;
#4988 = LINE ( 'NONE', #30088, #4098 ) ;
#4989 = DIRECTION ( 'NONE',  ( 0.5877852522924731371, 0.000000000000000000, 0.8090169943749474513 ) ) ;
#4990 = CARTESIAN_POINT ( 'NONE',  ( 34.47095863366522650, -11.93304594944324926, -18.87179757263150037 ) ) ;
#4991 = CARTESIAN_POINT ( 'NONE',  ( 9.641352920869014298, 17.66888146263751125, -17.91030124961049097 ) ) ;
#4992 = EDGE_LOOP ( 'NONE', ( #20045, #15327, #18477, #14680 ) ) ;
#4993 = VECTOR ( 'NONE', #2599, 1000.000000000000000 ) ;
#4994 = FACE_OUTER_BOUND ( 'NONE', #10305, .T. ) ;
#4995 = DIRECTION ( 'NONE',  ( -0.5877852522924731371, -1.586114251531760728E-16, -0.8090169943749474513 ) ) ;
#4996 = CARTESIAN_POINT ( 'NONE',  ( 12.67163634847678644, 8.538173360731750705, -16.25940050138558135 ) ) ;
#4997 = B_SPLINE_CURVE_WITH_KNOTS ( 'NONE', 3,
 ( #27875, #25092, #9037, #13331, #6930, #22807 ),
 .UNSPECIFIED., .F., .F.,
 ( 4, 2, 4 ),
 ( 0.004120275011746841846, 0.005288420935197130079, 0.006456566858647419180 ),
 .UNSPECIFIED. ) ;
#4998 = DIRECTION ( 'NONE',  ( 0.5877852522924731371, 1.586114251531760728E-16, 0.8090169943749474513 ) ) ;
#4999 = FACE_OUTER_BOUND ( 'NONE', #3079, .T. ) ;
#5000 = ORIENTED_EDGE ( 'NONE', *, *, #24560, .T. ) ;
#5001 = ORIENTED_EDGE ( 'NONE', *, *, #4358, .T. ) ;
#5002 = DIRECTION ( 'NONE',  ( 1.110223024625156540E-16, 2.995891024602366092E-32, 1.000000000000000000 ) ) ;
#5003 = VERTEX_POINT ( 'NONE', #20529 ) ;
#5004 = DIRECTION ( 'NONE',  ( -0.9510565162951536422, -2.566386769018988323E-16, 0.3090169943749475623 ) ) ;
#5005 = VECTOR ( 'NONE', #25618, 1000.000000000000000 ) ;
#5006 = ORIENTED_EDGE ( 'NONE', *, *, #4699, .T. ) ;
#5007 = DIRECTION ( 'NONE',  ( 1.908098474094866580E-16, -0.7071067811865481278, -0.7071067811865469066 ) ) ;
#5008 = VERTEX_POINT ( 'NONE', #15798 ) ;
#5009 = CARTESIAN_POINT ( 'NONE',  ( 9.670405002872021427, 16.21574392470601467, -17.88402698595844598 ) ) ;
#5010 = EDGE_CURVE ( 'NONE', #14, #22156, #29616, .T. ) ;
#5011 = CARTESIAN_POINT ( 'NONE',  ( 25.47886751038978304, -3.221426504603704277, -15.37741025701318698 ) ) ;
#5012 = CARTESIAN_POINT ( 'NONE',  ( 19.47299019774181161, -1.479546722229555744, -17.51644493673600067 ) ) ;
#5013 = CARTESIAN_POINT ( 'NONE',  ( 168.6922820468852819, -9.999999999999998224, 2.247092850131519715 ) ) ;
#5014 = DIRECTION ( 'NONE',  ( 0.000000000000000000, 0.5000000000000011102, 0.8660254037844380415 ) ) ;
#5015 = LINE ( 'NONE', #14304, #5005 ) ;
#5016 = CARTESIAN_POINT ( 'NONE',  ( 22.09544204423535874, -4.864148257255451746, -14.35781331922719772 ) ) ;
#5017 = CARTESIAN_POINT ( 'NONE',  ( 180.7287565553229740, -84.33034373659253902, 0.5000000000000029976 ) ) ;
#5018 = FACE_OUTER_BOUND ( 'NONE', #2962, .T. ) ;
#5019 = CARTESIAN_POINT ( 'NONE',  ( 153.6922820468854241, -1.999999999999974909, -26.58683881228715862 ) ) ;
#5020 = CARTESIAN_POINT ( 'NONE',  ( 0.000000000000000000, 0.000000000000000000, -2.450000000000000622 ) ) ;
#5021 = VECTOR ( 'NONE', #23927, 1000.000000000000000 ) ;
#5022 = CARTESIAN_POINT ( 'NONE',  ( 10.63408956504272140, 15.70892033759881734, -17.26778321585235787 ) ) ;
#5023 = LINE ( 'NONE', #5904, #20399 ) ;
#5024 = CARTESIAN_POINT ( 'NONE',  ( 34.39741479528305490, -17.01287786994462792, -20.00997473120332515 ) ) ;
#5025 = VERTEX_POINT ( 'NONE', #11076 ) ;
#5026 = CARTESIAN_POINT ( 'NONE',  ( 8.944586743066221146, 16.95158331485313852, -17.91159992548655566 ) ) ;
#5027 = ORIENTED_EDGE ( 'NONE', *, *, #11950, .T. ) ;
#5028 = CARTESIAN_POINT ( 'NONE',  ( 20.00000000000017053, 34.64101615137744972, 14.00000000000000178 ) ) ;
#5029 = CARTESIAN_POINT ( 'NONE',  ( 17.18819971663578272, 0.8441372818425427749, -18.45219435416397502 ) ) ;
#5030 = CARTESIAN_POINT ( 'NONE',  ( 11.34095285796786712, 16.37991182834946713, -16.75774407480071559 ) ) ;
#5031 = DIRECTION ( 'NONE',  ( -0.000000000000000000, -0.000000000000000000, 1.000000000000000000 ) ) ;
#5032 = ORIENTED_EDGE ( 'NONE', *, *, #11212, .F. ) ;
#5033 = VECTOR ( 'NONE', #18274, 1000.000000000000000 ) ;
#5034 = ORIENTED_EDGE ( 'NONE', *, *, #4741, .T. ) ;
#5035 = CARTESIAN_POINT ( 'NONE',  ( 9.641350810849047548, 17.66889113945805789, -17.93331994345748370 ) ) ;
#5036 = LINE ( 'NONE', #12345, #8685 ) ;
#5037 = CARTESIAN_POINT ( 'NONE',  ( 9.918725397012197575, 16.39681593027784956, -16.50360835092378409 ) ) ;
#5038 = CARTESIAN_POINT ( 'NONE',  ( 147.0152310637605524, -10.00000000000000178, -6.958068083716895558 ) ) ;
#5039 = ORIENTED_EDGE ( 'NONE', *, *, #2717, .T. ) ;
#5040 = DIRECTION ( 'NONE',  ( -0.8090169943749474513, -2.183098979609982436E-16, -0.5877852522924731371 ) ) ;
#5041 = ORIENTED_EDGE ( 'NONE', *, *, #20481, .T. ) ;
#5042 = CARTESIAN_POINT ( 'NONE',  ( 10.48820292689142519, 16.37797505638186735, -17.32811247259324716 ) ) ;
#5043 = EDGE_CURVE ( 'NONE', #26475, #5593, #6207, .T. ) ;
#5044 = VERTEX_POINT ( 'NONE', #13513 ) ;
#5045 = CARTESIAN_POINT ( 'NONE',  ( 33.72790161547175103, -10.96501189107364738, -20.51660325596433765 ) ) ;
#5046 = CARTESIAN_POINT ( 'NONE',  ( 26.87449084144840938, -11.88902188497427481, -13.49525739704605343 ) ) ;
#5047 = CARTESIAN_POINT ( 'NONE',  ( 13.75440121443578079, 9.907639265912045801, -15.40915901261088905 ) ) ;
#5048 = ORIENTED_EDGE ( 'NONE', *, *, #26142, .T. ) ;
#5049 = EDGE_CURVE ( 'NONE', #22761, #29150, #8483, .T. ) ;
#5050 = DIRECTION ( 'NONE',  ( 0.5877852522924731371, 0.000000000000000000, 0.8090169943749474513 ) ) ;
#5051 = AXIS2_PLACEMENT_3D ( 'NONE', #27093, #15602, #10265 ) ;
#5052 = CARTESIAN_POINT ( 'NONE',  ( 34.39307579391925174, -12.50091474996580487, -19.93840237985029162 ) ) ;
#5053 = PRODUCT_CONTEXT ( 'NONE', #10450, 'mechanical' ) ;
#5054 = CARTESIAN_POINT ( 'NONE',  ( 13.40933447586352578, 7.914523597318124715, -14.40541938456405369 ) ) ;
#5055 = CARTESIAN_POINT ( 'NONE',  ( 29.11570147443254797, -8.594497869595446815, -15.09001435577217087 ) ) ;
#5056 = ORIENTED_EDGE ( 'NONE', *, *, #9583, .T. ) ;
#5057 = ORIENTED_EDGE ( 'NONE', *, *, #30196, .T. ) ;
#5058 = FACE_BOUND ( 'NONE', #21629, .T. ) ;
#5059 = CARTESIAN_POINT ( 'NONE',  ( 151.1922820468854241, -1.999999999999976685, -19.40354224447947828 ) ) ;
#5060 = LINE ( 'NONE', #19691, #29688 ) ;
#5061 =( BOUNDED_SURFACE ( )  B_SPLINE_SURFACE ( 3, 3, ( 
 ( #25118, #10913, #1782, #29608, #4062, #6200, #15647, #13356, #11067, #4208, #13505, #11503, #83, #23577, #7253, #2833, #27893, #12118, #7548, #18695, #2673, #20818, #7408, #18539, #16709, #9673, #18995, #26179, #28353, #14246, #6955, #21434, #25719, #23272, #16243, #28500, #9515, #28198, #16852, #13796, #11959, #26030, #14094, #23122, #5104, #18837, #9364, #25555, #28040, #19142, #7096, #16396, #25876, #20974, #4650, #16553, #4801, #14394, #545, #11660, #23428, #23736, #2385, #4956, #13942, #2231, #2541, #30202, #11811, #21126, #9827, #9212, #238, #21275, #387, #24331, #10275, #3425, #10422, #24040, #14698, #21880, #12716, #17598, #8138, #3139, #10124, #26794, #5866, #15148, #14547, #12413, #24479, #29099, #12562, #17297, #17445, #19433, #10579, #3577, #12267, #19287, #12866, #29255, #28807, #14998, #21586, #22179, #9972, #1290, #1142, #19731, #5260, #19886, #5717, #28643, #8289, #17154, #21730, #7694, #23895, #992, #19584, #2992, #684, #22038, #17006, #5563, #26330, #5413, #28953, #833, #7845, #26483, #14843, #24185, #3287, #26636, #7989, #29418, #11028, #29565, #18195, #4315, #24786, #27263, #1898, #6163, #20332, #1441, #2047, #10875, #11326, #15457, #13171, #15903, #9023, #17883, #8730, #27101, #15754, #1741, #25079, #11178, #3876, #22497, #13319, #4167, #26953, #29874, #1598, #20185, #27555, #6608, #25231, #6010, #8586, #13615, #20486, #4023, #18045, #8882, #6313, #20633, #22947, #3726 ),
 ( #15608, #30013, #15297, #22789, #6462, #29721, #24629, #24941, #10734, #13023, #22643, #13463, #22339, #20046, #8439, #17741, #27411, #18501, #25526, #7369, #20782, #23389, #30168, #18659, #11464, #48, #503, #2642, #16666, #23692, #2505, #23540, #16051, #4618, #28161, #11773, #25988, #9176, #18802, #27856, #13908, #14058, #21091, #11920, #6917, #23235, #28311, #21238, #5065, #353, #16210, #9638, #28004, #25837, #18956, #14355, #4473, #2350, #7063, #25678, #11623, #16356, #2797, #12079, #7216, #4764, #21396, #18348, #23092, #20936, #2195, #16509, #9329, #27704, #200, #9479, #4916, #14211, #6761, #25379, #13763, #7659, #10083, #29058, #15111, #19548, #22000, #28918, #8096, #17408, #26443, #10387, #16965, #12230, #5377, #24442, #5219, #21545, #26754, #649, #26290, #14660, #14959, #10236, #24007, #9934, #19104, #28459, #7509, #24292, #5823, #3387, #7952, #16809, #5677, #19246, #14805, #19395, #3537, #792, #28602, #9786, #12829, #3102, #17261, #24145, #28766, #26590, #5524, #12377, #22143, #12680, #26140, #3249, #1108, #21689, #7810, #17116, #12524, #21842, #19696, #14511, #948, #23853, #2953, #20008, #1706, #29376, #29531, #10841, #15570, #6432, #24904, #20297, #3839, #22299, #26911, #12985, #15724, #11149, #25052, #27380, #18011, #4139, #15868, #10989, #13431, #29685, #20451, #29844, #17851, #1870, #8400, #3684, #27066, #25198, #5973, #1405, #8849, #10698, #17705, #6121, #22758, #8700, #15419, #24753 ),
 ( #18164, #29211, #27525, #13131, #6277, #20149, #6580, #22463, #1561, #1249, #4288, #8548, #13590, #3990, #27227, #10536, #13289, #22607, #19844, #8249, #17560, #15262, #24593, #23062, #27821, #6888, #25346, #4439, #16473, #9601, #16177, #11435, #2017, #20745, #23352, #30134, #20900, #2316, #7031, #28122, #16322, #11741, #25498, #13735, #18311, #2161, #7181, #2612, #25800, #18769, #9444, #4880, #7332, #9141, #2466, #18469, #4587, #18623, #25639, #14176, #13877, #23199, #11887, #23503, #21202, #317, #11586, #18922, #11, #164, #28275, #16630, #8993, #16021, #9298, #27971, #4729, #14023, #25950, #5030, #21059, #22914, #11296, #20600, #27667, #29983, #6730, #14769, #5341, #17230, #12194, #7772, #19072, #28425, #26719, #21652, #21964, #21510, #14626, #3359, #19660, #23974, #7477, #26257, #14321, #28888, #12645, #29025, #19362, #19515, #12045, #617, #24112, #17084, #1078, #16780, #10356, #8063, #19211, #3211, #21359, #7920, #26105, #26557, #10201, #5644, #23657, #14922, #12489, #5183, #17374, #3064, #23816, #14478, #2759, #10048, #28723, #464, #9751, #21812, #24262, #12340, #2914, #9901, #26407, #28568, #7621, #16926, #751, #5487, #910, #17822, #12949, #8214, #20120, #8370, #27346, #13400, #3653, #6090, #10956, #15229, #29500, #10500, #11115, #19972, #20418, #24564, #22262, #25021, #18126, #27033, #27192, #5944, #24871, #10812, #3960, #20266, #1371, #10663, #22426, #13258, #5791, #8669, #29343, #17677 ),
 ( #15386, #15073, #22728, #26880, #6245, #8520, #24719, #15540, #1529, #3806, #29809, #22577, #8818, #1677, #29653, #13097, #17974, #6401, #17525, #15692, #4106, #1832, #24412, #3507, #12800, #22115, #1217, #19812, #29178, #6849, #11546, #2427, #20862, #16284, #30097, #18275, #22878, #8959, #16141, #30245, #11704, #9256, #25595, #9106, #27633, #1983, #6698, #21021, #7139, #126, #23314, #13985, #9410, #11853, #15987, #27936, #25314, #13704, #23162, #18584, #18736, #4406, #23029, #16438, #28082, #25762, #4843, #2131, #14141, #27786, #4690, #23470, #2580, #13551, #20567, #25459, #4550, #11401, #13839, #21167, #277, #6995, #2279, #9561, #27492, #11264, #29950, #20709, #6544, #18435, #15833, #25164, #4255, #23619, #2718, #1040, #26223, #26524, #16749, #19181, #7888, #24230, #28686, #879, #7738, #17197, #5607, #5303, #19482, #26072, #21318, #14441, #3329, #14286, #427, #14884, #9710, #5147, #23780, #24080, #19328, #2874, #19035, #28238, #7292, #16594, #3181, #12608, #12453, #17049, #25919, #14736, #28392, #23938, #28537, #21925, #9868, #7446, #18881, #4996, #12159, #26375, #3029, #7587, #5454, #14589, #21473, #12005, #21779, #583, #12307, #10166, #16891, #21623, #719, #10013, #28850, #3923, #27309, #3620, #29142, #19626, #8179, #10781, #17491, #8338, #29619, #24375, #8633, #4071, #15194, #20090, #17338, #13220, #15041, #22544, #6209, #15501, #22689, #24832, #29466, #3468, #17934, #22226, #19771, #12761 ),
 ( #1642, #10626, #13365, #10922, #15343, #5912, #22082, #26843, #15657, #24529, #12911, #22387, #1336, #1185, #24681, #19935, #20230, #6363, #29304, #17640, #24989, #26997, #3771, #10465, #10318, #6058, #28993, #13064, #1493, #8029, #26684, #8485, #17788, #27146, #5759, #11371, #6809, #23546, #22844, #13515, #22991, #25846, #2804, #11925, #1945, #8926, #359, #9644, #18963, #1790, #11229, #28319, #21246, #2094, #27750, #7378, #18241, #14365, #16673, #8779, #23699, #6658, #5072, #20531, #4366, #20676, #29917, #2650, #25995, #11079, #4925, #9071, #20379, #27598, #25126, #29769, #15950, #18093, #27458, #25277, #6508, #15800, #13667, #30059, #18397, #4217, #16519, #14217, #15296, #29564, #2309, #6461, #15751, #25077, #4583, #4724, #1440, #20331, #29417, #6162, #15607, #29251, #8288, #17597, #13872, #27965, #23195, #29720, #26952, #11582, #20044, #24940, #8585, #25635, #10874, #8438, #19885, #7027, #10732, #8729, #4020, #20183, #18044, #6312, #15456, #14017, #27410, #23348, #13318, #20896, #17739, #24785, #3875, #22337, #27100, #7, #16317, #13170, #22495, #6009, #1597, #9293, #17882, #27262, #22641, #1740, #18618, #11027, #2462, #24628, #3724, #13021, #7177, #21355, #23971, #28564, #7618, #16922, #26252, #26405, #23498, #12191, #21195, #28272, #7474, #26101, #5338, #11883, #18918, #21649, #14623, #747, #3060, #313, #12335, #12040, #19208, #10045, #19358, #28118, #4876, #460, #19066, #9596, #9747, #28720 ),
 ( #14172, #25795, #21507, #2753, #7767, #7326, #5180, #16469, #2608, #24108, #28420, #17081, #16626, #16777, #5484, #14767, #611, #11737, #9898, #21054, #160, #14472, #9438, #25945, #5026, #14317, #18764, #23652, #23814, #2911, #14919, #10353, #19658, #8367, #3650, #29023, #24259, #6084, #12946, #1215, #29497, #6241, #7917, #5639, #17228, #22259, #24410, #15382, #1073, #26877, #26555, #3357, #15537, #10498, #10808, #8060, #3505, #22421, #8517, #1367, #24715, #10658, #1526, #20117, #19809, #3803, #17369, #12643, #26716, #17816, #28885, #21962, #27189, #5789, #15071, #12795, #17673, #19969, #22113, #29172, #12486, #21810, #908, #27030, #3208, #13094, #29340, #10199, #19511, #8211, #17521, #5941, #15225, #24558, #25016, #24868, #2273, #15687, #25310, #29945, #15829, #4399, #11260, #20414, #9252, #23023, #18581, #8955, #9102, #4102, #29805, #8814, #27342, #6397, #18430, #11542, #18121, #13396, #3956, #22723, #13700, #1828, #22871, #4250, #18271, #30093, #27628, #2126, #27486, #11107, #20262, #29647, #13546, #6845, #11397, #20704, #27781, #16134, #27928, #6540, #25455, #25159, #1979, #20561, #6694, #4545, #15982, #13835, #23158, #20857, #30241, #6990, #13254, #22573, #1674, #10954, #8664, #17970, #2424, #9402, #16590, #23615, #4839, #14282, #9864, #26067, #28534, #5142, #5300, #14585, #2711, #16887, #23466, #18731, #11848, #716, #11700, #28078, #23934, #7134, #2575, #21159, #21470, #16745, #273, #16434 ),
 ( #19177, #25756, #9556, #7583, #26217, #3026, #25591, #14137, #12302, #21619, #11999, #28388, #10009, #18877, #19324, #28683, #23309, #16279, #28234, #4686, #7287, #25915, #21314, #4991, #579, #13979, #12156, #14433, #9706, #21017, #423, #121, #19031, #7442, #23776, #2871, #21775, #26994, #26839, #12449, #7885, #14881, #6051, #10163, #12755, #19475, #19932, #876, #15340, #24075, #22222, #24677, #13061, #22079, #12908, #5451, #24227, #17488, #1181, #3768, #28847, #22384, #1489, #12605, #5909, #14732, #1332, #17193, #10623, #3616, #29299, #20087, #8335, #8176, #26520, #10778, #19623, #5602, #3326, #7732, #3465, #10462, #17045, #26372, #15191, #17638, #8026, #3178, #21922, #19767, #1034, #10315, #28989, #17334, #26680, #5756, #29138, #15038, #24371, #24523, #1787, #20672, #20227, #8776, #6505, #17931, #13664, #30056, #25274, #8923, #22839, #9067, #29613, #3919, #11368, #6360, #18237, #6654, #13217, #18394, #27595, #22541, #8630, #15654, #27747, #1639, #4213, #10918, #6806, #27306, #16098, #15498, #22988, #25423, #4512, #13512, #4360, #27142, #24986, #15947, #1942, #13801, #4068, #23128, #2238, #13361, #2091, #6206, #11508, #22686, #29463, #8481, #17782, #24829, #11074, #29914, #20376, #29766, #18090, #27454, #15796, #25123, #11226, #20528, #14555, #23902, #9678, #26036, #21133, #2999, #14401, #25884, #16401, #13948, #7101, #26186, #25726, #23435, #2680, #28046, #23279, #4962, #2547, #12126, #28506, #18700 ) ),
 .UNSPECIFIED., .T., .F., .F. ) 
 B_SPLINE_SURFACE_WITH_KNOTS ( ( 4, 3, 4 ),
 ( 4, 2, 2, 2, 2, 2, 2, 2, 2, 2, 2, 2, 2, 2, 2, 2, 2, 2, 2, 2, 2, 2, 2, 2, 2, 2, 2, 2, 2, 2, 2, 2, 2, 2, 2, 2, 2, 2, 2, 2, 2, 2, 2, 2, 2, 2, 2, 2, 2, 2, 2, 2, 2, 2, 2, 2, 2, 2, 2, 2, 2, 2, 2, 2, 2, 2, 2, 2, 2, 2, 2, 2, 2, 2, 2, 2, 2, 2, 2, 2, 2, 2, 2, 2, 2, 2, 2, 2, 2, 2, 2, 2, 4 ),
 ( 0.000000000000000000, 0.5000000000000000000, 1.000000000000000000 ),
 ( 0.000000000000000000, 0.2329478137359916323, 0.2349098735327962983, 0.2358909034311986175, 0.2363814183803997770, 0.2366266758550003568, 0.2367493045923006467, 0.2368106189609507917, 0.2368719333296009644, 0.2369056680493116240, 0.2369394027690223115, 0.2370068722084436863, 0.2371418110872863805, 0.2374116888449718243, 0.2379514443603427121, 0.2390309553910844875, 0.2411899774525679829, 0.2455080215755349737, 0.2541441098214689553, 0.2714162863133369186, 0.2886884628052048818, 0.2973245510511388634, 0.3016425951741058542, 0.3038016172355893496, 0.3048811282663310696, 0.3054208837817019573, 0.3056907615393874011, 0.3058257004182300953, 0.3058931698576514702, 0.3059269045773621576, 0.3059606392970728450, 0.3060023410584322145, 0.3060440428197915841, 0.3061274463425103787, 0.3062942533879479123, 0.3066278674788229797, 0.3072950956605731143, 0.3086295520240733836, 0.3112984647510739222, 0.3166362902050750550, 0.3273119411130772649, 0.3486632429290816293, 0.3913658465610904136, 0.4767710538251080377, 0.5621762610891256617, 0.6048788647211345015, 0.6262301665371388104, 0.6369058174451409648, 0.6422436428991420421, 0.6449125556261425807, 0.6462470119896428500, 0.6469142401713929846, 0.6472478542622681630, 0.6474146613077056411, 0.6474980648304244912, 0.6475397665917839163, 0.6475814683531432303, 0.6476196945210073164, 0.6476579206888715134, 0.6477343730245996856, 0.6478872776960560298, 0.6481930870389687183, 0.6488047057247940952, 0.6500279430964450711, 0.6524744178397468009, 0.6573673673263502604, 0.6671532662995571794, 0.6769391652727642095, 0.6867250642459712395, 0.6965109632191782696, 0.7062968621923852997, 0.7160827611655922187, 0.7209757106521956782, 0.7234221853954974080, 0.7246454227671483839, 0.7252570414529737608, 0.7255628507958864493, 0.7257157554673427935, 0.7257922078030709656, 0.7258304339709351627, 0.7258686601387992487, 0.7259088784260310234, 0.7259490967132626871, 0.7260295332877260144, 0.7261904064366526690, 0.7265121527345062002, 0.7271556453302130407, 0.7284426305216267217, 0.7310166009044543056, 0.7361645416701092515, 0.7464604232014193652, 0.7670521862640395927, 1.000000000000000000 ),
 .UNSPECIFIED. ) 
 GEOMETRIC_REPRESENTATION_ITEM ( )  RATIONAL_B_SPLINE_SURFACE ( (
 ( 1.000000000000000000, 1.000000000000000000, 1.000000000000000000, 1.000000000000000000, 1.000000000000000000, 1.000000000000000000, 1.000000000000000000, 1.000000000000000000, 1.000000000000000000, 1.000000000000000000, 1.000000000000000000, 1.000000000000000000, 1.000000000000000000, 1.000000000000000000, 1.000000000000000000, 1.000000000000000000, 1.000000000000000000, 1.000000000000000000, 1.000000000000000000, 1.000000000000000000, 1.000000000000000000, 1.000000000000000000, 1.000000000000000000, 1.000000000000000000, 1.000000000000000000, 1.000000000000000000, 1.000000000000000000, 1.000000000000000000, 1.000000000000000000, 1.000000000000000000, 1.000000000000000000, 1.000000000000000000, 1.000000000000000000, 1.000000000000000000, 1.000000000000000000, 1.000000000000000000, 1.000000000000000000, 1.000000000000000000, 1.000000000000000000, 1.000000000000000000, 1.000000000000000000, 1.000000000000000000, 1.000000000000000000, 1.000000000000000000, 1.000000000000000000, 1.000000000000000000, 1.000000000000000000, 1.000000000000000000, 1.000000000000000000, 1.000000000000000000, 1.000000000000000000, 1.000000000000000000, 1.000000000000000000, 1.000000000000000000, 1.000000000000000000, 1.000000000000000000, 1.000000000000000000, 1.000000000000000000, 1.000000000000000000, 1.000000000000000000, 1.000000000000000000, 1.000000000000000000, 1.000000000000000000, 1.000000000000000000, 1.000000000000000000, 1.000000000000000000, 1.000000000000000000, 1.000000000000000000, 1.000000000000000000, 1.000000000000000000, 1.000000000000000000, 1.000000000000000000, 1.000000000000000000, 1.000000000000000000, 1.000000000000000000, 1.000000000000000000, 1.000000000000000000, 1.000000000000000000, 1.000000000000000000, 1.000000000000000000, 1.000000000000000000, 1.000000000000000000, 1.000000000000000000, 1.000000000000000000, 1.000000000000000000, 1.000000000000000000, 1.000000000000000000, 1.000000000000000000, 1.000000000000000000, 1.000000000000000000, 1.000000000000000000, 1.000000000000000000, 1.000000000000000000, 1.000000000000000000, 1.000000000000000000, 1.000000000000000000, 1.000000000000000000, 1.000000000000000000, 1.000000000000000000, 1.000000000000000000, 1.000000000000000000, 1.000000000000000000, 1.000000000000000000, 1.000000000000000000, 1.000000000000000000, 1.000000000000000000, 1.000000000000000000, 1.000000000000000000, 1.000000000000000000, 1.000000000000000000, 1.000000000000000000, 1.000000000000000000, 1.000000000000000000, 1.000000000000000000, 1.000000000000000000, 1.000000000000000000, 1.000000000000000000, 1.000000000000000000, 1.000000000000000000, 1.000000000000000000, 1.000000000000000000, 1.000000000000000000, 1.000000000000000000, 1.000000000000000000, 1.000000000000000000, 1.000000000000000000, 1.000000000000000000, 1.000000000000000000, 1.000000000000000000, 1.000000000000000000, 1.000000000000000000, 1.000000000000000000, 1.000000000000000000, 1.000000000000000000, 1.000000000000000000, 1.000000000000000000, 1.000000000000000000, 1.000000000000000000, 1.000000000000000000, 1.000000000000000000, 1.000000000000000000, 1.000000000000000000, 1.000000000000000000, 1.000000000000000000, 1.000000000000000000, 1.000000000000000000, 1.000000000000000000, 1.000000000000000000, 1.000000000000000000, 1.000000000000000000, 1.000000000000000000, 1.000000000000000000, 1.000000000000000000, 1.000000000000000000, 1.000000000000000000, 1.000000000000000000, 1.000000000000000000, 1.000000000000000000, 1.000000000000000000, 1.000000000000000000, 1.000000000000000000, 1.000000000000000000, 1.000000000000000000, 1.000000000000000000, 1.000000000000000000, 1.000000000000000000, 1.000000000000000000, 1.000000000000000000, 1.000000000000000000, 1.000000000000000000, 1.000000000000000000, 1.000000000000000000, 1.000000000000000000, 1.000000000000000000, 1.000000000000000000, 1.000000000000000000, 1.000000000000000000, 1.000000000000000000, 1.000000000000000000, 1.000000000000000000, 1.000000000000000000, 1.000000000000000000, 1.000000000000000000, 1.000000000000000000, 1.000000000000000000, 1.000000000000000000),
 ( 0.3333333333333333703, 0.3333333333333333703, 0.3333333333333333703, 0.3333333333333333703, 0.3333333333333333703, 0.3333333333333333703, 0.3333333333333333703, 0.3333333333333333703, 0.3333333333333333703, 0.3333333333333333703, 0.3333333333333333703, 0.3333333333333333703, 0.3333333333333333703, 0.3333333333333333703, 0.3333333333333333703, 0.3333333333333333703, 0.3333333333333333703, 0.3333333333333333703, 0.3333333333333333703, 0.3333333333333333703, 0.3333333333333333703, 0.3333333333333333703, 0.3333333333333333703, 0.3333333333333333703, 0.3333333333333333703, 0.3333333333333333703, 0.3333333333333333703, 0.3333333333333333703, 0.3333333333333333703, 0.3333333333333333703, 0.3333333333333333703, 0.3333333333333333703, 0.3333333333333333703, 0.3333333333333333703, 0.3333333333333333703, 0.3333333333333333703, 0.3333333333333333703, 0.3333333333333333703, 0.3333333333333333703, 0.3333333333333333703, 0.3333333333333333703, 0.3333333333333333703, 0.3333333333333333703, 0.3333333333333333703, 0.3333333333333333703, 0.3333333333333333703, 0.3333333333333333703, 0.3333333333333333703, 0.3333333333333333703, 0.3333333333333333703, 0.3333333333333333703, 0.3333333333333333703, 0.3333333333333333703, 0.3333333333333333703, 0.3333333333333333703, 0.3333333333333333703, 0.3333333333333333703, 0.3333333333333333703, 0.3333333333333333703, 0.3333333333333333703, 0.3333333333333333703, 0.3333333333333333703, 0.3333333333333333703, 0.3333333333333333703, 0.3333333333333333703, 0.3333333333333333703, 0.3333333333333333703, 0.3333333333333333703, 0.3333333333333333703, 0.3333333333333333703, 0.3333333333333333703, 0.3333333333333333703, 0.3333333333333333703, 0.3333333333333333703, 0.3333333333333333703, 0.3333333333333333703, 0.3333333333333333703, 0.3333333333333333703, 0.3333333333333333703, 0.3333333333333333703, 0.3333333333333333703, 0.3333333333333333703, 0.3333333333333333703, 0.3333333333333333703, 0.3333333333333333703, 0.3333333333333333703, 0.3333333333333333703, 0.3333333333333333703, 0.3333333333333333703, 0.3333333333333333703, 0.3333333333333333703, 0.3333333333333333703, 0.3333333333333333703, 0.3333333333333333703, 0.3333333333333333703, 0.3333333333333333703, 0.3333333333333333703, 0.3333333333333333703, 0.3333333333333333703, 0.3333333333333333703, 0.3333333333333333703, 0.3333333333333333703, 0.3333333333333333703, 0.3333333333333333703, 0.3333333333333333703, 0.3333333333333333703, 0.3333333333333333703, 0.3333333333333333703, 0.3333333333333333703, 0.3333333333333333703, 0.3333333333333333703, 0.3333333333333333703, 0.3333333333333333703, 0.3333333333333333703, 0.3333333333333333703, 0.3333333333333333703, 0.3333333333333333703, 0.3333333333333333703, 0.3333333333333333703, 0.3333333333333333703, 0.3333333333333333703, 0.3333333333333333703, 0.3333333333333333703, 0.3333333333333333703, 0.3333333333333333703, 0.3333333333333333703, 0.3333333333333333703, 0.3333333333333333703, 0.3333333333333333703, 0.3333333333333333703, 0.3333333333333333703, 0.3333333333333333703, 0.3333333333333333703, 0.3333333333333333703, 0.3333333333333333703, 0.3333333333333333703, 0.3333333333333333703, 0.3333333333333333703, 0.3333333333333333703, 0.3333333333333333703, 0.3333333333333333703, 0.3333333333333333703, 0.3333333333333333703, 0.3333333333333333703, 0.3333333333333333703, 0.3333333333333333703, 0.3333333333333333703, 0.3333333333333333703, 0.3333333333333333703, 0.3333333333333333703, 0.3333333333333333703, 0.3333333333333333703, 0.3333333333333333703, 0.3333333333333333703, 0.3333333333333333703, 0.3333333333333333703, 0.3333333333333333703, 0.3333333333333333703, 0.3333333333333333703, 0.3333333333333333703, 0.3333333333333333703, 0.3333333333333333703, 0.3333333333333333703, 0.3333333333333333703, 0.3333333333333333703, 0.3333333333333333703, 0.3333333333333333703, 0.3333333333333333703, 0.3333333333333333703, 0.3333333333333333703, 0.3333333333333333703, 0.3333333333333333703, 0.3333333333333333703, 0.3333333333333333703, 0.3333333333333333703, 0.3333333333333333703, 0.3333333333333333703, 0.3333333333333333703, 0.3333333333333333703, 0.3333333333333333703, 0.3333333333333333703, 0.3333333333333333703, 0.3333333333333333703, 0.3333333333333333703, 0.3333333333333333703, 0.3333333333333333703),
 ( 0.3333333333333333703, 0.3333333333333333703, 0.3333333333333333703, 0.3333333333333333703, 0.3333333333333333703, 0.3333333333333333703, 0.3333333333333333703, 0.3333333333333333703, 0.3333333333333333703, 0.3333333333333333703, 0.3333333333333333703, 0.3333333333333333703, 0.3333333333333333703, 0.3333333333333333703, 0.3333333333333333703, 0.3333333333333333703, 0.3333333333333333703, 0.3333333333333333703, 0.3333333333333333703, 0.3333333333333333703, 0.3333333333333333703, 0.3333333333333333703, 0.3333333333333333703, 0.3333333333333333703, 0.3333333333333333703, 0.3333333333333333703, 0.3333333333333333703, 0.3333333333333333703, 0.3333333333333333703, 0.3333333333333333703, 0.3333333333333333703, 0.3333333333333333703, 0.3333333333333333703, 0.3333333333333333703, 0.3333333333333333703, 0.3333333333333333703, 0.3333333333333333703, 0.3333333333333333703, 0.3333333333333333703, 0.3333333333333333703, 0.3333333333333333703, 0.3333333333333333703, 0.3333333333333333703, 0.3333333333333333703, 0.3333333333333333703, 0.3333333333333333703, 0.3333333333333333703, 0.3333333333333333703, 0.3333333333333333703, 0.3333333333333333703, 0.3333333333333333703, 0.3333333333333333703, 0.3333333333333333703, 0.3333333333333333703, 0.3333333333333333703, 0.3333333333333333703, 0.3333333333333333703, 0.3333333333333333703, 0.3333333333333333703, 0.3333333333333333703, 0.3333333333333333703, 0.3333333333333333703, 0.3333333333333333703, 0.3333333333333333703, 0.3333333333333333703, 0.3333333333333333703, 0.3333333333333333703, 0.3333333333333333703, 0.3333333333333333703, 0.3333333333333333703, 0.3333333333333333703, 0.3333333333333333703, 0.3333333333333333703, 0.3333333333333333703, 0.3333333333333333703, 0.3333333333333333703, 0.3333333333333333703, 0.3333333333333333703, 0.3333333333333333703, 0.3333333333333333703, 0.3333333333333333703, 0.3333333333333333703, 0.3333333333333333703, 0.3333333333333333703, 0.3333333333333333703, 0.3333333333333333703, 0.3333333333333333703, 0.3333333333333333703, 0.3333333333333333703, 0.3333333333333333703, 0.3333333333333333703, 0.3333333333333333703, 0.3333333333333333703, 0.3333333333333333703, 0.3333333333333333703, 0.3333333333333333703, 0.3333333333333333703, 0.3333333333333333703, 0.3333333333333333703, 0.3333333333333333703, 0.3333333333333333703, 0.3333333333333333703, 0.3333333333333333703, 0.3333333333333333703, 0.3333333333333333703, 0.3333333333333333703, 0.3333333333333333703, 0.3333333333333333703, 0.3333333333333333703, 0.3333333333333333703, 0.3333333333333333703, 0.3333333333333333703, 0.3333333333333333703, 0.3333333333333333703, 0.3333333333333333703, 0.3333333333333333703, 0.3333333333333333703, 0.3333333333333333703, 0.3333333333333333703, 0.3333333333333333703, 0.3333333333333333703, 0.3333333333333333703, 0.3333333333333333703, 0.3333333333333333703, 0.3333333333333333703, 0.3333333333333333703, 0.3333333333333333703, 0.3333333333333333703, 0.3333333333333333703, 0.3333333333333333703, 0.3333333333333333703, 0.3333333333333333703, 0.3333333333333333703, 0.3333333333333333703, 0.3333333333333333703, 0.3333333333333333703, 0.3333333333333333703, 0.3333333333333333703, 0.3333333333333333703, 0.3333333333333333703, 0.3333333333333333703, 0.3333333333333333703, 0.3333333333333333703, 0.3333333333333333703, 0.3333333333333333703, 0.3333333333333333703, 0.3333333333333333703, 0.3333333333333333703, 0.3333333333333333703, 0.3333333333333333703, 0.3333333333333333703, 0.3333333333333333703, 0.3333333333333333703, 0.3333333333333333703, 0.3333333333333333703, 0.3333333333333333703, 0.3333333333333333703, 0.3333333333333333703, 0.3333333333333333703, 0.3333333333333333703, 0.3333333333333333703, 0.3333333333333333703, 0.3333333333333333703, 0.3333333333333333703, 0.3333333333333333703, 0.3333333333333333703, 0.3333333333333333703, 0.3333333333333333703, 0.3333333333333333703, 0.3333333333333333703, 0.3333333333333333703, 0.3333333333333333703, 0.3333333333333333703, 0.3333333333333333703, 0.3333333333333333703, 0.3333333333333333703, 0.3333333333333333703, 0.3333333333333333703, 0.3333333333333333703, 0.3333333333333333703, 0.3333333333333333703, 0.3333333333333333703, 0.3333333333333333703, 0.3333333333333333703, 0.3333333333333333703, 0.3333333333333333703),
 ( 1.000000000000000000, 1.000000000000000000, 1.000000000000000000, 1.000000000000000000, 1.000000000000000000, 1.000000000000000000, 1.000000000000000000, 1.000000000000000000, 1.000000000000000000, 1.000000000000000000, 1.000000000000000000, 1.000000000000000000, 1.000000000000000000, 1.000000000000000000, 1.000000000000000000, 1.000000000000000000, 1.000000000000000000, 1.000000000000000000, 1.000000000000000000, 1.000000000000000000, 1.000000000000000000, 1.000000000000000000, 1.000000000000000000, 1.000000000000000000, 1.000000000000000000, 1.000000000000000000, 1.000000000000000000, 1.000000000000000000, 1.000000000000000000, 1.000000000000000000, 1.000000000000000000, 1.000000000000000000, 1.000000000000000000, 1.000000000000000000, 1.000000000000000000, 1.000000000000000000, 1.000000000000000000, 1.000000000000000000, 1.000000000000000000, 1.000000000000000000, 1.000000000000000000, 1.000000000000000000, 1.000000000000000000, 1.000000000000000000, 1.000000000000000000, 1.000000000000000000, 1.000000000000000000, 1.000000000000000000, 1.000000000000000000, 1.000000000000000000, 1.000000000000000000, 1.000000000000000000, 1.000000000000000000, 1.000000000000000000, 1.000000000000000000, 1.000000000000000000, 1.000000000000000000, 1.000000000000000000, 1.000000000000000000, 1.000000000000000000, 1.000000000000000000, 1.000000000000000000, 1.000000000000000000, 1.000000000000000000, 1.000000000000000000, 1.000000000000000000, 1.000000000000000000, 1.000000000000000000, 1.000000000000000000, 1.000000000000000000, 1.000000000000000000, 1.000000000000000000, 1.000000000000000000, 1.000000000000000000, 1.000000000000000000, 1.000000000000000000, 1.000000000000000000, 1.000000000000000000, 1.000000000000000000, 1.000000000000000000, 1.000000000000000000, 1.000000000000000000, 1.000000000000000000, 1.000000000000000000, 1.000000000000000000, 1.000000000000000000, 1.000000000000000000, 1.000000000000000000, 1.000000000000000000, 1.000000000000000000, 1.000000000000000000, 1.000000000000000000, 1.000000000000000000, 1.000000000000000000, 1.000000000000000000, 1.000000000000000000, 1.000000000000000000, 1.000000000000000000, 1.000000000000000000, 1.000000000000000000, 1.000000000000000000, 1.000000000000000000, 1.000000000000000000, 1.000000000000000000, 1.000000000000000000, 1.000000000000000000, 1.000000000000000000, 1.000000000000000000, 1.000000000000000000, 1.000000000000000000, 1.000000000000000000, 1.000000000000000000, 1.000000000000000000, 1.000000000000000000, 1.000000000000000000, 1.000000000000000000, 1.000000000000000000, 1.000000000000000000, 1.000000000000000000, 1.000000000000000000, 1.000000000000000000, 1.000000000000000000, 1.000000000000000000, 1.000000000000000000, 1.000000000000000000, 1.000000000000000000, 1.000000000000000000, 1.000000000000000000, 1.000000000000000000, 1.000000000000000000, 1.000000000000000000, 1.000000000000000000, 1.000000000000000000, 1.000000000000000000, 1.000000000000000000, 1.000000000000000000, 1.000000000000000000, 1.000000000000000000, 1.000000000000000000, 1.000000000000000000, 1.000000000000000000, 1.000000000000000000, 1.000000000000000000, 1.000000000000000000, 1.000000000000000000, 1.000000000000000000, 1.000000000000000000, 1.000000000000000000, 1.000000000000000000, 1.000000000000000000, 1.000000000000000000, 1.000000000000000000, 1.000000000000000000, 1.000000000000000000, 1.000000000000000000, 1.000000000000000000, 1.000000000000000000, 1.000000000000000000, 1.000000000000000000, 1.000000000000000000, 1.000000000000000000, 1.000000000000000000, 1.000000000000000000, 1.000000000000000000, 1.000000000000000000, 1.000000000000000000, 1.000000000000000000, 1.000000000000000000, 1.000000000000000000, 1.000000000000000000, 1.000000000000000000, 1.000000000000000000, 1.000000000000000000, 1.000000000000000000, 1.000000000000000000, 1.000000000000000000, 1.000000000000000000, 1.000000000000000000, 1.000000000000000000, 1.000000000000000000, 1.000000000000000000, 1.000000000000000000, 1.000000000000000000, 1.000000000000000000, 1.000000000000000000, 1.000000000000000000),
 ( 0.3333333333333333703, 0.3333333333333333703, 0.3333333333333333703, 0.3333333333333333703, 0.3333333333333333703, 0.3333333333333333703, 0.3333333333333333703, 0.3333333333333333703, 0.3333333333333333703, 0.3333333333333333703, 0.3333333333333333703, 0.3333333333333333703, 0.3333333333333333703, 0.3333333333333333703, 0.3333333333333333703, 0.3333333333333333703, 0.3333333333333333703, 0.3333333333333333703, 0.3333333333333333703, 0.3333333333333333703, 0.3333333333333333703, 0.3333333333333333703, 0.3333333333333333703, 0.3333333333333333703, 0.3333333333333333703, 0.3333333333333333703, 0.3333333333333333703, 0.3333333333333333703, 0.3333333333333333703, 0.3333333333333333703, 0.3333333333333333703, 0.3333333333333333703, 0.3333333333333333703, 0.3333333333333333703, 0.3333333333333333703, 0.3333333333333333703, 0.3333333333333333703, 0.3333333333333333703, 0.3333333333333333703, 0.3333333333333333703, 0.3333333333333333703, 0.3333333333333333703, 0.3333333333333333703, 0.3333333333333333703, 0.3333333333333333703, 0.3333333333333333703, 0.3333333333333333703, 0.3333333333333333703, 0.3333333333333333703, 0.3333333333333333703, 0.3333333333333333703, 0.3333333333333333703, 0.3333333333333333703, 0.3333333333333333703, 0.3333333333333333703, 0.3333333333333333703, 0.3333333333333333703, 0.3333333333333333703, 0.3333333333333333703, 0.3333333333333333703, 0.3333333333333333703, 0.3333333333333333703, 0.3333333333333333703, 0.3333333333333333703, 0.3333333333333333703, 0.3333333333333333703, 0.3333333333333333703, 0.3333333333333333703, 0.3333333333333333703, 0.3333333333333333703, 0.3333333333333333703, 0.3333333333333333703, 0.3333333333333333703, 0.3333333333333333703, 0.3333333333333333703, 0.3333333333333333703, 0.3333333333333333703, 0.3333333333333333703, 0.3333333333333333703, 0.3333333333333333703, 0.3333333333333333703, 0.3333333333333333703, 0.3333333333333333703, 0.3333333333333333703, 0.3333333333333333703, 0.3333333333333333703, 0.3333333333333333703, 0.3333333333333333703, 0.3333333333333333703, 0.3333333333333333703, 0.3333333333333333703, 0.3333333333333333703, 0.3333333333333333703, 0.3333333333333333703, 0.3333333333333333703, 0.3333333333333333703, 0.3333333333333333703, 0.3333333333333333703, 0.3333333333333333703, 0.3333333333333333703, 0.3333333333333333703, 0.3333333333333333703, 0.3333333333333333703, 0.3333333333333333703, 0.3333333333333333703, 0.3333333333333333703, 0.3333333333333333703, 0.3333333333333333703, 0.3333333333333333703, 0.3333333333333333703, 0.3333333333333333703, 0.3333333333333333703, 0.3333333333333333703, 0.3333333333333333703, 0.3333333333333333703, 0.3333333333333333703, 0.3333333333333333703, 0.3333333333333333703, 0.3333333333333333703, 0.3333333333333333703, 0.3333333333333333703, 0.3333333333333333703, 0.3333333333333333703, 0.3333333333333333703, 0.3333333333333333703, 0.3333333333333333703, 0.3333333333333333703, 0.3333333333333333703, 0.3333333333333333703, 0.3333333333333333703, 0.3333333333333333703, 0.3333333333333333703, 0.3333333333333333703, 0.3333333333333333703, 0.3333333333333333703, 0.3333333333333333703, 0.3333333333333333703, 0.3333333333333333703, 0.3333333333333333703, 0.3333333333333333703, 0.3333333333333333703, 0.3333333333333333703, 0.3333333333333333703, 0.3333333333333333703, 0.3333333333333333703, 0.3333333333333333703, 0.3333333333333333703, 0.3333333333333333703, 0.3333333333333333703, 0.3333333333333333703, 0.3333333333333333703, 0.3333333333333333703, 0.3333333333333333703, 0.3333333333333333703, 0.3333333333333333703, 0.3333333333333333703, 0.3333333333333333703, 0.3333333333333333703, 0.3333333333333333703, 0.3333333333333333703, 0.3333333333333333703, 0.3333333333333333703, 0.3333333333333333703, 0.3333333333333333703, 0.3333333333333333703, 0.3333333333333333703, 0.3333333333333333703, 0.3333333333333333703, 0.3333333333333333703, 0.3333333333333333703, 0.3333333333333333703, 0.3333333333333333703, 0.3333333333333333703, 0.3333333333333333703, 0.3333333333333333703, 0.3333333333333333703, 0.3333333333333333703, 0.3333333333333333703, 0.3333333333333333703, 0.3333333333333333703, 0.3333333333333333703, 0.3333333333333333703, 0.3333333333333333703, 0.3333333333333333703, 0.3333333333333333703, 0.3333333333333333703),
 ( 0.3333333333333333703, 0.3333333333333333703, 0.3333333333333333703, 0.3333333333333333703, 0.3333333333333333703, 0.3333333333333333703, 0.3333333333333333703, 0.3333333333333333703, 0.3333333333333333703, 0.3333333333333333703, 0.3333333333333333703, 0.3333333333333333703, 0.3333333333333333703, 0.3333333333333333703, 0.3333333333333333703, 0.3333333333333333703, 0.3333333333333333703, 0.3333333333333333703, 0.3333333333333333703, 0.3333333333333333703, 0.3333333333333333703, 0.3333333333333333703, 0.3333333333333333703, 0.3333333333333333703, 0.3333333333333333703, 0.3333333333333333703, 0.3333333333333333703, 0.3333333333333333703, 0.3333333333333333703, 0.3333333333333333703, 0.3333333333333333703, 0.3333333333333333703, 0.3333333333333333703, 0.3333333333333333703, 0.3333333333333333703, 0.3333333333333333703, 0.3333333333333333703, 0.3333333333333333703, 0.3333333333333333703, 0.3333333333333333703, 0.3333333333333333703, 0.3333333333333333703, 0.3333333333333333703, 0.3333333333333333703, 0.3333333333333333703, 0.3333333333333333703, 0.3333333333333333703, 0.3333333333333333703, 0.3333333333333333703, 0.3333333333333333703, 0.3333333333333333703, 0.3333333333333333703, 0.3333333333333333703, 0.3333333333333333703, 0.3333333333333333703, 0.3333333333333333703, 0.3333333333333333703, 0.3333333333333333703, 0.3333333333333333703, 0.3333333333333333703, 0.3333333333333333703, 0.3333333333333333703, 0.3333333333333333703, 0.3333333333333333703, 0.3333333333333333703, 0.3333333333333333703, 0.3333333333333333703, 0.3333333333333333703, 0.3333333333333333703, 0.3333333333333333703, 0.3333333333333333703, 0.3333333333333333703, 0.3333333333333333703, 0.3333333333333333703, 0.3333333333333333703, 0.3333333333333333703, 0.3333333333333333703, 0.3333333333333333703, 0.3333333333333333703, 0.3333333333333333703, 0.3333333333333333703, 0.3333333333333333703, 0.3333333333333333703, 0.3333333333333333703, 0.3333333333333333703, 0.3333333333333333703, 0.3333333333333333703, 0.3333333333333333703, 0.3333333333333333703, 0.3333333333333333703, 0.3333333333333333703, 0.3333333333333333703, 0.3333333333333333703, 0.3333333333333333703, 0.3333333333333333703, 0.3333333333333333703, 0.3333333333333333703, 0.3333333333333333703, 0.3333333333333333703, 0.3333333333333333703, 0.3333333333333333703, 0.3333333333333333703, 0.3333333333333333703, 0.3333333333333333703, 0.3333333333333333703, 0.3333333333333333703, 0.3333333333333333703, 0.3333333333333333703, 0.3333333333333333703, 0.3333333333333333703, 0.3333333333333333703, 0.3333333333333333703, 0.3333333333333333703, 0.3333333333333333703, 0.3333333333333333703, 0.3333333333333333703, 0.3333333333333333703, 0.3333333333333333703, 0.3333333333333333703, 0.3333333333333333703, 0.3333333333333333703, 0.3333333333333333703, 0.3333333333333333703, 0.3333333333333333703, 0.3333333333333333703, 0.3333333333333333703, 0.3333333333333333703, 0.3333333333333333703, 0.3333333333333333703, 0.3333333333333333703, 0.3333333333333333703, 0.3333333333333333703, 0.3333333333333333703, 0.3333333333333333703, 0.3333333333333333703, 0.3333333333333333703, 0.3333333333333333703, 0.3333333333333333703, 0.3333333333333333703, 0.3333333333333333703, 0.3333333333333333703, 0.3333333333333333703, 0.3333333333333333703, 0.3333333333333333703, 0.3333333333333333703, 0.3333333333333333703, 0.3333333333333333703, 0.3333333333333333703, 0.3333333333333333703, 0.3333333333333333703, 0.3333333333333333703, 0.3333333333333333703, 0.3333333333333333703, 0.3333333333333333703, 0.3333333333333333703, 0.3333333333333333703, 0.3333333333333333703, 0.3333333333333333703, 0.3333333333333333703, 0.3333333333333333703, 0.3333333333333333703, 0.3333333333333333703, 0.3333333333333333703, 0.3333333333333333703, 0.3333333333333333703, 0.3333333333333333703, 0.3333333333333333703, 0.3333333333333333703, 0.3333333333333333703, 0.3333333333333333703, 0.3333333333333333703, 0.3333333333333333703, 0.3333333333333333703, 0.3333333333333333703, 0.3333333333333333703, 0.3333333333333333703, 0.3333333333333333703, 0.3333333333333333703, 0.3333333333333333703, 0.3333333333333333703, 0.3333333333333333703, 0.3333333333333333703, 0.3333333333333333703, 0.3333333333333333703, 0.3333333333333333703, 0.3333333333333333703),
 ( 1.000000000000000000, 1.000000000000000000, 1.000000000000000000, 1.000000000000000000, 1.000000000000000000, 1.000000000000000000, 1.000000000000000000, 1.000000000000000000, 1.000000000000000000, 1.000000000000000000, 1.000000000000000000, 1.000000000000000000, 1.000000000000000000, 1.000000000000000000, 1.000000000000000000, 1.000000000000000000, 1.000000000000000000, 1.000000000000000000, 1.000000000000000000, 1.000000000000000000, 1.000000000000000000, 1.000000000000000000, 1.000000000000000000, 1.000000000000000000, 1.000000000000000000, 1.000000000000000000, 1.000000000000000000, 1.000000000000000000, 1.000000000000000000, 1.000000000000000000, 1.000000000000000000, 1.000000000000000000, 1.000000000000000000, 1.000000000000000000, 1.000000000000000000, 1.000000000000000000, 1.000000000000000000, 1.000000000000000000, 1.000000000000000000, 1.000000000000000000, 1.000000000000000000, 1.000000000000000000, 1.000000000000000000, 1.000000000000000000, 1.000000000000000000, 1.000000000000000000, 1.000000000000000000, 1.000000000000000000, 1.000000000000000000, 1.000000000000000000, 1.000000000000000000, 1.000000000000000000, 1.000000000000000000, 1.000000000000000000, 1.000000000000000000, 1.000000000000000000, 1.000000000000000000, 1.000000000000000000, 1.000000000000000000, 1.000000000000000000, 1.000000000000000000, 1.000000000000000000, 1.000000000000000000, 1.000000000000000000, 1.000000000000000000, 1.000000000000000000, 1.000000000000000000, 1.000000000000000000, 1.000000000000000000, 1.000000000000000000, 1.000000000000000000, 1.000000000000000000, 1.000000000000000000, 1.000000000000000000, 1.000000000000000000, 1.000000000000000000, 1.000000000000000000, 1.000000000000000000, 1.000000000000000000, 1.000000000000000000, 1.000000000000000000, 1.000000000000000000, 1.000000000000000000, 1.000000000000000000, 1.000000000000000000, 1.000000000000000000, 1.000000000000000000, 1.000000000000000000, 1.000000000000000000, 1.000000000000000000, 1.000000000000000000, 1.000000000000000000, 1.000000000000000000, 1.000000000000000000, 1.000000000000000000, 1.000000000000000000, 1.000000000000000000, 1.000000000000000000, 1.000000000000000000, 1.000000000000000000, 1.000000000000000000, 1.000000000000000000, 1.000000000000000000, 1.000000000000000000, 1.000000000000000000, 1.000000000000000000, 1.000000000000000000, 1.000000000000000000, 1.000000000000000000, 1.000000000000000000, 1.000000000000000000, 1.000000000000000000, 1.000000000000000000, 1.000000000000000000, 1.000000000000000000, 1.000000000000000000, 1.000000000000000000, 1.000000000000000000, 1.000000000000000000, 1.000000000000000000, 1.000000000000000000, 1.000000000000000000, 1.000000000000000000, 1.000000000000000000, 1.000000000000000000, 1.000000000000000000, 1.000000000000000000, 1.000000000000000000, 1.000000000000000000, 1.000000000000000000, 1.000000000000000000, 1.000000000000000000, 1.000000000000000000, 1.000000000000000000, 1.000000000000000000, 1.000000000000000000, 1.000000000000000000, 1.000000000000000000, 1.000000000000000000, 1.000000000000000000, 1.000000000000000000, 1.000000000000000000, 1.000000000000000000, 1.000000000000000000, 1.000000000000000000, 1.000000000000000000, 1.000000000000000000, 1.000000000000000000, 1.000000000000000000, 1.000000000000000000, 1.000000000000000000, 1.000000000000000000, 1.000000000000000000, 1.000000000000000000, 1.000000000000000000, 1.000000000000000000, 1.000000000000000000, 1.000000000000000000, 1.000000000000000000, 1.000000000000000000, 1.000000000000000000, 1.000000000000000000, 1.000000000000000000, 1.000000000000000000, 1.000000000000000000, 1.000000000000000000, 1.000000000000000000, 1.000000000000000000, 1.000000000000000000, 1.000000000000000000, 1.000000000000000000, 1.000000000000000000, 1.000000000000000000, 1.000000000000000000, 1.000000000000000000, 1.000000000000000000, 1.000000000000000000, 1.000000000000000000, 1.000000000000000000, 1.000000000000000000, 1.000000000000000000, 1.000000000000000000, 1.000000000000000000, 1.000000000000000000, 1.000000000000000000, 1.000000000000000000) ) ) 
 REPRESENTATION_ITEM ( '' )  SURFACE ( )  );
#5062 = CARTESIAN_POINT ( 'NONE',  ( 157.0152310637604671, -1.999999999999974465, -8.721423840594312082 ) ) ;
#5063 = CARTESIAN_POINT ( 'NONE',  ( -12.69484042717385464, 39.89788248176327556, 4.999999999999998224 ) ) ;
#5064 = VECTOR ( 'NONE', #2457, 1000.000000000000000 ) ;
#5065 = CARTESIAN_POINT ( 'NONE',  ( 10.70792791965113544, 16.69018921775036546, -15.96040338026158523 ) ) ;
#5066 = LINE ( 'NONE', #7371, #17270 ) ;
#5067 = ORIENTED_EDGE ( 'NONE', *, *, #24358, .F. ) ;
#5068 = CARTESIAN_POINT ( 'NONE',  ( 156.1922820468853388, -4.999999999999976019, -2.083034168790677043 ) ) ;
#5069 = ORIENTED_EDGE ( 'NONE', *, *, #29993, .T. ) ;
#5070 = CARTESIAN_POINT ( 'NONE',  ( 10.07879545831710999, 15.66271422494645904, -16.43741374977755143 ) ) ;
#5071 = ORIENTED_EDGE ( 'NONE', *, *, #17582, .F. ) ;
#5072 = CARTESIAN_POINT ( 'NONE',  ( 9.668002105539015290, 16.22676391817335784, -17.88502066855795292 ) ) ;
#5073 = CARTESIAN_POINT ( 'NONE',  ( 21.92347772697934261, 3.537472258236324052, -14.28107661384214211 ) ) ;
#5074 = DIRECTION ( 'NONE',  ( 0.9510565162951536422, 2.566386769018988816E-16, 0.3090169943749472292 ) ) ;
#5075 = SURFACE_SIDE_STYLE ('',( #28611 ) ) ;
#5076 = CARTESIAN_POINT ( 'NONE',  ( 28.47856004806874353, -11.16640101040803401, -12.66155532224275149 ) ) ;
#5077 = ORIENTED_EDGE ( 'NONE', *, *, #27482, .F. ) ;
#5078 = DIRECTION ( 'NONE',  ( 0.3090169943749472292, 8.338696094057992503E-17, -0.9510565162951536422 ) ) ;
#5079 = CARTESIAN_POINT ( 'NONE',  ( 11.27643094638968613, 16.67581753947769130, -16.78442615493024803 ) ) ;
#5080 = ADVANCED_FACE ( 'NONE', ( #29767 ), #17784, .T. ) ;
#5081 = EDGE_LOOP ( 'NONE', ( #2441, #27057, #21294, #23293 ) ) ;
#5082 = EDGE_CURVE ( 'NONE', #16768, #26056, #11726, .T. ) ;
#5083 = B_SPLINE_CURVE_WITH_KNOTS ( 'NONE', 3,
 ( #10917, #8628, #4212, #8480, #18089, #3766 ),
 .UNSPECIFIED., .F., .F.,
 ( 4, 2, 4 ),
 ( 0.002336974151641508721, 0.003500975885716453660, 0.004664977619791398598 ),
 .UNSPECIFIED. ) ;
#5084 = CARTESIAN_POINT ( 'NONE',  ( 33.69611315462438483, -12.86230108826256924, -18.75566652118837752 ) ) ;
#5085 = CARTESIAN_POINT ( 'NONE',  ( 17.63704213852533442, 9.806822523219006271, -18.50018230520716145 ) ) ;
#5086 = EDGE_CURVE ( 'NONE', #5568, #27071, #29464, .T. ) ;
#5087 = CARTESIAN_POINT ( 'NONE',  ( 148.6922820468853672, -1.999999999999977573, -0.6060766987539614181 ) ) ;
#5088 = CARTESIAN_POINT ( 'NONE',  ( 9.760963200462100531, 13.20757681744125911, -16.78657487285272509 ) ) ;
#5089 = EDGE_CURVE ( 'NONE', #4291, #20426, #24830, .T. ) ;
#5090 = CARTESIAN_POINT ( 'NONE',  ( 25.30932029414111284, -7.960302465696846852, -19.79224777486898645 ) ) ;
#5091 = ORIENTED_EDGE ( 'NONE', *, *, #27098, .T. ) ;
#5092 = CYLINDRICAL_SURFACE ( 'NONE', #15418, 3.000000000000002665 ) ;
#5093 = CARTESIAN_POINT ( 'NONE',  ( 19.85388831290292799, 7.668379621071204078, -15.62993620635094061 ) ) ;
#5094 = CARTESIAN_POINT ( 'NONE',  ( 17.11242430243909141, 7.828829022555451544, -19.39938683153768295 ) ) ;
#5095 = VECTOR ( 'NONE', #23427, 1000.000000000000000 ) ;
#5096 = DIRECTION ( 'NONE',  ( 0.000000000000000000, 0.000000000000000000, 1.000000000000000000 ) ) ;
#5097 = VERTEX_POINT ( 'NONE', #27596 ) ;
#5098 = ORIENTED_EDGE ( 'NONE', *, *, #20511, .T. ) ;
#5099 = CARTESIAN_POINT ( 'NONE',  ( 0.000000000000000000, 0.000000000000000000, 0.000000000000000000 ) ) ;
#5100 = FACE_OUTER_BOUND ( 'NONE', #29736, .T. ) ;
#5101 = CARTESIAN_POINT ( 'NONE',  ( -20.00000000000017053, 34.64101615137744972, -10.00000000000000000 ) ) ;
#5102 = DIRECTION ( 'NONE',  ( 0.5877852522924731371, 1.586114251531760728E-16, 0.8090169943749474513 ) ) ;
#5103 = CARTESIAN_POINT ( 'NONE',  ( 13.87499999999999822, 0.000000000000000000, 0.000000000000000000 ) ) ;
#5104 = CARTESIAN_POINT ( 'NONE',  ( 9.879812780108833792, 16.57527415160161510, -16.52987074417163527 ) ) ;
#5105 = CARTESIAN_POINT ( 'NONE',  ( 27.04162508513615393, -6.753966733322825711, -13.61186222264828771 ) ) ;
#5106 = CARTESIAN_POINT ( 'NONE',  ( 20.59283418570449697, -4.290598171560842111, -16.90930062131523215 ) ) ;
#5108 = ORIENTED_EDGE ( 'NONE', *, *, #28150, .T. ) ;
#5107 = CARTESIAN_POINT ( 'NONE',  ( 36.54859390953723874, -23.18451583373416014, -14.99999999999999822 ) ) ;
#5109 = CARTESIAN_POINT ( 'NONE',  ( 174.5152310637604955, -9.999999999999994671, -28.60870317832789667 ) ) ;
#5110 = PLANE ( 'NONE',  #21390 ) ;
#5111 = AXIS2_PLACEMENT_3D ( 'NONE', #25524, #8881, #18193 ) ;
#5112 = CARTESIAN_POINT ( 'NONE',  ( 22.20786350129493059, -5.000000000000011546, -68.34877589377062179 ) ) ;
#5113 = DIRECTION ( 'NONE',  ( 0.9510565162951536422, 2.566386769018988816E-16, 0.3090169943749472292 ) ) ;
#5114 = CARTESIAN_POINT ( 'NONE',  ( 15.39489021548154568, 6.697694061803245447, -14.95590323207311734 ) ) ;
#5115 = DIRECTION ( 'NONE',  ( 0.5877852522924731371, 1.586114251531760728E-16, -0.8090169943749474513 ) ) ;
#5116 = CARTESIAN_POINT ( 'NONE',  ( 10.33811693838771717, 18.38618951776012267, -17.91796598306941135 ) ) ;
#5117 = DIRECTION ( 'NONE',  ( -1.000000000000000000, 0.000000000000000000, 0.000000000000000000 ) ) ;
#5118 = CARTESIAN_POINT ( 'NONE',  ( 157.0152310637605524, -9.999999999999998224, -24.27857615940569502 ) ) ;
#5119 = EDGE_CURVE ( 'NONE', #7935, #29938, #6901, .T. ) ;
#5120 = CARTESIAN_POINT ( 'NONE',  ( 14.29829396236512729, 6.476847147513518088, -18.28004444394726491 ) ) ;
#5121 = EDGE_CURVE ( 'NONE', #14937, #4331, #2507, .T. ) ;
#5122 = EDGE_CURVE ( 'NONE', #14810, #5097, #1334, .T. ) ;
#5123 = CARTESIAN_POINT ( 'NONE',  ( 14.70433163182692482, 6.391443753141328621, -13.74806202935933541 ) ) ;
#5124 = ORIENTED_EDGE ( 'NONE', *, *, #10865, .T. ) ;
#5125 = EDGE_CURVE ( 'NONE', #28553, #12786, #21496, .T. ) ;
#5126 = CARTESIAN_POINT ( 'NONE',  ( 33.57712230886461668, -13.32773824946660923, -19.76201999124979736 ) ) ;
#5127 = VECTOR ( 'NONE', #19327, 1000.000000000000000 ) ;
#5128 = CARTESIAN_POINT ( 'NONE',  ( 22.26732294003774015, -3.469656073077215463, -14.71322089325822624 ) ) ;
#5129 = VERTEX_POINT ( 'NONE', #27144 ) ;
#5130 = CARTESIAN_POINT ( 'NONE',  ( 22.34502977332646978, 2.679400364154326919, -18.33342593408658061 ) ) ;
#5131 = CARTESIAN_POINT ( 'NONE',  ( 27.40270966038060152, -12.25096941946872953, -16.90735844088681006 ) ) ;
#5132 = ORIENTED_EDGE ( 'NONE', *, *, #16484, .F. ) ;
#5133 = VECTOR ( 'NONE', #27522, 999.9999999999998863 ) ;
#5134 = EDGE_LOOP ( 'NONE', ( #28756, #26610, #7566, #11979 ) ) ;
#5135 = DIRECTION ( 'NONE',  ( 0.3090169943749472292, 8.338696094057992503E-17, -0.9510565162951536422 ) ) ;
#5137 = ORIENTED_EDGE ( 'NONE', *, *, #4021, .T. ) ;
#5136 = LINE ( 'NONE', #4833, #23865 ) ;
#5138 = LINE ( 'NONE', #12443, #2190 ) ;
#5139 = FACE_OUTER_BOUND ( 'NONE', #11007, .T. ) ;
#5140 = AXIS2_PLACEMENT_3D ( 'NONE', #11668, #8632, #17933 ) ;
#5141 = CARTESIAN_POINT ( 'NONE',  ( 34.56382110058589774, -12.26799042007339757, -18.94768870749412315 ) ) ;
#5142 = CARTESIAN_POINT ( 'NONE',  ( 12.75938622741416140, 7.627299838292535661, -14.92343961094405103 ) ) ;
#5143 = ORIENTED_EDGE ( 'NONE', *, *, #5010, .T. ) ;
#5144 = AXIS2_PLACEMENT_3D ( 'NONE', #16753, #26076, #26228 ) ;
#5145 = LINE ( 'NONE', #425, #34 ) ;
#5146 = LINE ( 'NONE', #7291, #28098 ) ;
#5147 = CARTESIAN_POINT ( 'NONE',  ( 12.02859841272590735, 9.313533661810568631, -16.69110409223909741 ) ) ;
#5148 = DIRECTION ( 'NONE',  ( 0.000000000000000000, 0.8660254037844390407, 0.4999999999999993339 ) ) ;
#5149 = DIRECTION ( 'NONE',  ( -2.698458740408365879E-16, 1.000000000000000000, 0.000000000000000000 ) ) ;
#5150 = VERTEX_POINT ( 'NONE', #29301 ) ;
#5151 = VECTOR ( 'NONE', #13987, 1000.000000000000000 ) ;
#5152 = LINE ( 'NONE', #14890, #19280 ) ;
#5153 = ORIENTED_EDGE ( 'NONE', *, *, #7399, .F. ) ;
#5154 = EDGE_CURVE ( 'NONE', #5542, #19491, #24430, .T. ) ;
#5155 = EDGE_CURVE ( 'NONE', #6477, #10414, #17639, .T. ) ;
#5156 = CARTESIAN_POINT ( 'NONE',  ( 176.1922820468852819, -9.999999999999994671, -10.74328820663507678 ) ) ;
#5157 = VERTEX_POINT ( 'NONE', #22542 ) ;
#5158 = EDGE_CURVE ( 'NONE', #8151, #28202, #1640, .T. ) ;
#5159 = DIRECTION ( 'NONE',  ( -0.9510565162951536422, -2.566386769018988816E-16, -0.3090169943749472292 ) ) ;
#5160 = EDGE_LOOP ( 'NONE', ( #8266, #9035, #468, #28301 ) ) ;
#5161 = ADVANCED_FACE ( 'NONE', ( #17932 ), #27307, .T. ) ;
#5162 = CARTESIAN_POINT ( 'NONE',  ( 12.27065153619900961, 7.644304191818388716, -16.55295716654172722 ) ) ;
#5163 = CARTESIAN_POINT ( 'NONE',  ( 23.69966960967911973, -9.104540460734687812, -16.16703237251472558 ) ) ;
#5164 = CARTESIAN_POINT ( 'NONE',  ( 26.20148740379470453, -2.166401353139026487, -14.75472287570676322 ) ) ;
#5165 = LINE ( 'NONE', #18748, #26250 ) ;
#5166 = LINE ( 'NONE', #14457, #12598 ) ;
#5167 = DIRECTION ( 'NONE',  ( -0.5877852522924731371, 0.000000000000000000, 0.8090169943749474513 ) ) ;
#5168 = VECTOR ( 'NONE', #30067, 1000.000000000000000 ) ;
#5169 = ORIENTED_EDGE ( 'NONE', *, *, #2649, .T. ) ;
#5170 = LINE ( 'NONE', #21495, #10354 ) ;
#5171 = CARTESIAN_POINT ( 'NONE',  ( 141.1922820468854525, -4.999999999999979572, -10.74328820663507678 ) ) ;
#5172 = DIRECTION ( 'NONE',  ( 0.000000000000000000, -0.5000000000000012212, -0.8660254037844380415 ) ) ;
#5173 = DIRECTION ( 'NONE',  ( 0.5877852522924731371, 1.586114251531760728E-16, 0.8090169943749474513 ) ) ;
#5175 = CARTESIAN_POINT ( 'NONE',  ( 172.2287565553228887, -9.999999999999996447, -12.16987298107780369 ) ) ;
#5174 = STYLED_ITEM ( 'NONE', ( #10528 ), #21737 ) ;
#5176 = CARTESIAN_POINT ( 'NONE',  ( 12.02748425217687789, 9.318634685891279190, -16.69156549717016702 ) ) ;
#5177 = CARTESIAN_POINT ( 'NONE',  ( 147.2287565553230024, -10.00000000000000355, -12.16987298107780369 ) ) ;
#5178 = CARTESIAN_POINT ( 'NONE',  ( 35.09336438560361415, -20.13941072448723801, -20.22035334018532637 ) ) ;
#5179 = ORIENTED_EDGE ( 'NONE', *, *, #8988, .T. ) ;
#5180 = CARTESIAN_POINT ( 'NONE',  ( 8.944584683310379702, 16.95159276115599667, -17.94384837343789130 ) ) ;
#5181 = DIRECTION ( 'NONE',  ( 0.000000000000000000, 0.000000000000000000, 1.000000000000000000 ) ) ;
#5182 = CARTESIAN_POINT ( 'NONE',  ( 16.94076125623460527, 0.4124075662712927692, -16.40086227390004936 ) ) ;
#5183 = CARTESIAN_POINT ( 'NONE',  ( 12.83348778413740376, 9.536125428572121976, -16.14043921975381934 ) ) ;
#5184 = CARTESIAN_POINT ( 'NONE',  ( 133.7287565553229172, -1.999999999999980904, -39.49999999999997158 ) ) ;
#5185 = ORIENTED_EDGE ( 'NONE', *, *, #3646, .T. ) ;
#5186 = CARTESIAN_POINT ( 'NONE',  ( 11.58682163191119230, 8.958038730125363003, -15.79767441425272345 ) ) ;
#5187 = DIRECTION ( 'NONE',  ( 0.000000000000000000, 0.000000000000000000, 1.000000000000000000 ) ) ;
#5188 = AXIS2_PLACEMENT_3D ( 'NONE', #11973, #21292, #19599 ) ;
#5189 = CARTESIAN_POINT ( 'NONE',  ( 11.14863080475985591, 10.75631295387255548, -15.99499920034263489 ) ) ;
#5190 = CARTESIAN_POINT ( 'NONE',  ( 136.1922820468854241, -1.999999999999980460, -22.25671179336495697 ) ) ;
#5191 = VERTEX_POINT ( 'NONE', #1788 ) ;
#5192 = EDGE_CURVE ( 'NONE', #27841, #4723, #20039, .T. ) ;
#5193 = CARTESIAN_POINT ( 'NONE',  ( 6.689127551062008514, 5.375634714784629509, -4.682649155111342942 ) ) ;
#5194 = ORIENTED_EDGE ( 'NONE', *, *, #27653, .T. ) ;
#5195 = ADVANCED_FACE ( 'NONE', ( #23436 ), #13950, .T. ) ;
#5196 = CARTESIAN_POINT ( 'NONE',  ( 12.02805304935487563, 9.316025821727821565, -16.69133030147860453 ) ) ;
#5197 = ORIENTED_EDGE ( 'NONE', *, *, #21304, .T. ) ;
#5199 = CARTESIAN_POINT ( 'NONE',  ( 36.02474454408307736, -19.83113812547715682, -20.43161669954002591 ) ) ;
#5198 = VECTOR ( 'NONE', #17273, 1000.000000000000000 ) ;
#5200 = CARTESIAN_POINT ( 'NONE',  ( 16.07247723200118372, 10.90037199175087324, -15.55898442674143745 ) ) ;
#5201 = CARTESIAN_POINT ( 'NONE',  ( 27.01132674553606350, -11.00696853675122711, -18.49859303458091730 ) ) ;
#5202 = ORIENTED_EDGE ( 'NONE', *, *, #6602, .T. ) ;
#5203 = ORIENTED_EDGE ( 'NONE', *, *, #9761, .F. ) ;
#5204 = AXIS2_PLACEMENT_3D ( 'NONE', #24791, #4476, #24945 ) ;
#5205 = CARTESIAN_POINT ( 'NONE',  ( 13.00000000000001243, 55.00000000000000711, 23.00000000000000000 ) ) ;
#5206 = ORIENTED_EDGE ( 'NONE', *, *, #29448, .T. ) ;
#5207 = CARTESIAN_POINT ( 'NONE',  ( 34.06228043176686526, -11.34293828116054037, -19.64761387034043949 ) ) ;
#5208 = CARTESIAN_POINT ( 'NONE',  ( 22.34502977332646978, 2.679400364154326919, -18.33342593408658061 ) ) ;
#5209 = CARTESIAN_POINT ( 'NONE',  ( 27.28761988882141765, -9.265112451392095494, -14.04413049427448001 ) ) ;
#5210 = DIRECTION ( 'NONE',  ( 1.110223024625156540E-16, 2.995891024602366092E-32, 1.000000000000000000 ) ) ;
#5211 = DIRECTION ( 'NONE',  ( 0.9510565162951535312, 2.566386769018988816E-16, -0.3090169943749475623 ) ) ;
#5212 = EDGE_CURVE ( 'NONE', #22963, #28478, #28206, .T. ) ;
#5213 = DIRECTION ( 'NONE',  ( -0.5877852522924731371, 0.000000000000000000, 0.8090169943749474513 ) ) ;
#5214 = LINE ( 'NONE', #12227, #16942 ) ;
#5215 = DIRECTION ( 'NONE',  ( -1.110223024625156540E-16, 0.000000000000000000, -1.000000000000000000 ) ) ;
#5216 = VECTOR ( 'NONE', #15582, 999.9999999999998863 ) ;
#5217 = DIRECTION ( 'NONE',  ( -2.207829878515935943E-16, 1.000000000000000000, 0.000000000000000000 ) ) ;
#5218 = VECTOR ( 'NONE', #19848, 999.9999999999998863 ) ;
#5219 = CARTESIAN_POINT ( 'NONE',  ( 12.24452513275510235, 9.643158527868859409, -15.32408204131529317 ) ) ;
#5220 = CARTESIAN_POINT ( 'NONE',  ( 166.1922820468853388, -1.999999999999972244, -13.59645775552055902 ) ) ;
#5221 = CARTESIAN_POINT ( 'NONE',  ( 129.5152310637605808, -1.999999999999982236, -19.94844914048349338 ) ) ;
#5222 = ORIENTED_EDGE ( 'NONE', *, *, #28393, .T. ) ;
#5223 = CARTESIAN_POINT ( 'NONE',  ( 12.50906579366657390, 8.574708520419219937, -15.12294941509656354 ) ) ;
#5224 = ORIENTED_EDGE ( 'NONE', *, *, #11440, .F. ) ;
#5225 = CARTESIAN_POINT ( 'NONE',  ( 16.80134558234102471, 1.491865220098682387, -17.16076555717535257 ) ) ;
#5226 = PLANE ( 'NONE',  #22450 ) ;
#5227 = DIRECTION ( 'NONE',  ( 1.000000000000000000, 0.000000000000000000, -0.000000000000000000 ) ) ;
#5228 = CARTESIAN_POINT ( 'NONE',  ( 168.6922820468853672, -1.999999999999971356, -32.39392330124607611 ) ) ;
#5229 = ORIENTED_EDGE ( 'NONE', *, *, #13147, .F. ) ;
#5230 = CARTESIAN_POINT ( 'NONE',  ( 141.1922820468854525, -1.999999999999978684, -30.91696583120935671 ) ) ;
#5231 = CARTESIAN_POINT ( 'NONE',  ( 11.27599706080618525, 16.67780739407118062, -16.78460567626121502 ) ) ;
#5232 = ORIENTED_EDGE ( 'NONE', *, *, #6569, .T. ) ;
#5233 = CARTESIAN_POINT ( 'NONE',  ( 35.35024494905714221, -20.29343902266242239, -19.25407150246939736 ) ) ;
#5234 = CARTESIAN_POINT ( 'NONE',  ( 16.89369580670022941, 0.5033910033923695293, -17.32063897790030893 ) ) ;
#5235 = ORIENTED_EDGE ( 'NONE', *, *, #4983, .T. ) ;
#5236 = VECTOR ( 'NONE', #15579, 999.9999999999998863 ) ;
#5237 = DIRECTION ( 'NONE',  ( -0.5877852522924731371, 0.000000000000000000, 0.8090169943749474513 ) ) ;
#5238 = CARTESIAN_POINT ( 'NONE',  ( 9.117643650280985668, 16.15792227874146292, -17.05261013695411165 ) ) ;
#5239 = CARTESIAN_POINT ( 'NONE',  ( 23.25962485557060688, -10.00107805802020167, -16.29084171305886386 ) ) ;
#5240 = EDGE_LOOP ( 'NONE', ( #26853, #27752, #16114, #5838 ) ) ;
#5241 = FACE_OUTER_BOUND ( 'NONE', #19291, .T. ) ;
#5242 = CARTESIAN_POINT ( 'NONE',  ( 17.94193213664724951, 0.5400182743772068417, -16.55803501089447849 ) ) ;
#5243 = VECTOR ( 'NONE', #11939, 1000.000000000000000 ) ;
#5244 = CARTESIAN_POINT ( 'NONE',  ( 18.17852402710872894, 9.427450501112501158, -16.79750701094832266 ) ) ;
#5245 = ORIENTED_EDGE ( 'NONE', *, *, #31, .F. ) ;
#5246 = CARTESIAN_POINT ( 'NONE',  ( 129.5152310637605808, -1.999999999999982236, -28.60870317832789311 ) ) ;
#5247 = VERTEX_POINT ( 'NONE', #18395 ) ;
#5248 = EDGE_LOOP ( 'NONE', ( #12189, #9231, #17662, #329 ) ) ;
#5249 = CARTESIAN_POINT ( 'NONE',  ( 129.5152310637605808, -10.00000000000000888, -19.94844914048349338 ) ) ;
#5250 = SHAPE_REPRESENTATION ( 'BR-593', ( #19982, #5369, #16075, #4858, #9730, #22435, #9243, #17534, #24883, #6354, #11691, #6835 ), #15597 ) ;
#5251 = FACE_OUTER_BOUND ( 'NONE', #13545, .T. ) ;
#5252 = ADVANCED_FACE ( 'NONE', ( #16101 ), #25424, .T. ) ;
#5253 = ADVANCED_FACE ( 'NONE', ( #7260 ), #90, .T. ) ;
#5254 = CARTESIAN_POINT ( 'NONE',  ( 169.7287565553230024, -4.999999999999971578, -33.82050807568879947 ) ) ;
#5255 = DIRECTION ( 'NONE',  ( 1.000000000000000000, -1.840388255087189623E-16, 0.000000000000000000 ) ) ;
#5256 = EDGE_CURVE ( 'NONE', #7473, #26028, #7416, .T. ) ;
#5257 = DIRECTION ( 'NONE',  ( -1.000000000000000000, -2.698458740408365879E-16, 1.779203565104417375E-16 ) ) ;
#5258 = AXIS2_PLACEMENT_3D ( 'NONE', #27198, #22887, #6251 ) ;
#5259 = EDGE_CURVE ( 'NONE', #22420, #7083, #9373, .T. ) ;
#5260 = CARTESIAN_POINT ( 'NONE',  ( 11.47276097331165623, 9.269810413962238371, -15.86095999428340697 ) ) ;
#5261 = CARTESIAN_POINT ( 'NONE',  ( 27.97039215263694345, -10.38370070276099710, -17.82092013489567606 ) ) ;
#5262 = CARTESIAN_POINT ( 'NONE',  ( 24.70156281743647142, 0.04986695427254615731, -17.03102378627558977 ) ) ;
#5264 = ORIENTED_EDGE ( 'NONE', *, *, #18755, .F. ) ;
#5263 = CARTESIAN_POINT ( 'NONE',  ( 31.15806985163746390, -10.82494328065958911, -14.16671120874331358 ) ) ;
#5265 = DIRECTION ( 'NONE',  ( 1.000000000000000000, 2.698458740408366372E-16, 0.000000000000000000 ) ) ;
#5266 = VECTOR ( 'NONE', #22020, 1000.000000000000000 ) ;
#5267 = DIRECTION ( 'NONE',  ( -0.000000000000000000, -1.000000000000000000, -0.000000000000000000 ) ) ;
#5268 = CARTESIAN_POINT ( 'NONE',  ( 158.6922820468853956, -9.999999999999998224, -23.73366926340167637 ) ) ;
#5269 = CARTESIAN_POINT ( 'NONE',  ( 172.0152310637604955, -4.999999999999971578, -24.27857615940569502 ) ) ;
#5270 = CARTESIAN_POINT ( 'NONE',  ( 154.5152310637605240, -1.999999999999974909, -11.28819510263909542 ) ) ;
#5271 = CARTESIAN_POINT ( 'NONE',  ( 21.41025690189560748, 5.821651141963339882, -16.00656683556521998 ) ) ;
#5272 = ORIENTED_EDGE ( 'NONE', *, *, #9408, .T. ) ;
#5273 = LINE ( 'NONE', #28511, #13445 ) ;
#5274 = CARTESIAN_POINT ( 'NONE',  ( 10.66955227599643408, 16.86618481130757630, -15.98952479117537173 ) ) ;
#5275 = PLANE ( 'NONE',  #5188 ) ;
#5276 = LINE ( 'NONE', #14863, #17595 ) ;
#5277 = CARTESIAN_POINT ( 'NONE',  ( 20.51249478307574847, 1.942573248051725709, -13.31196225760961838 ) ) ;
#5278 = CARTESIAN_POINT ( 'NONE',  ( 17.55932102202221046, 11.64018535857498193, -15.95102284318303276 ) ) ;
#5279 = ORIENTED_EDGE ( 'NONE', *, *, #16236, .T. ) ;
#5280 = CARTESIAN_POINT ( 'NONE',  ( 32.52799721746220740, -11.03300674309804386, -18.03857687357939099 ) ) ;
#5281 = CARTESIAN_POINT ( 'NONE',  ( 20.39818463913025681, -2.063888138892570723, -16.18016139629216354 ) ) ;
#5282 = CARTESIAN_POINT ( 'NONE',  ( 19.90313213008900206, 2.415960287222779890, -14.54935787103550560 ) ) ;
#5283 = VECTOR ( 'NONE', #2789, 1000.000000000000114 ) ;
#5284 = ORIENTED_EDGE ( 'NONE', *, *, #14359, .F. ) ;
#5285 = CARTESIAN_POINT ( 'NONE',  ( 29.44447141382201139, -6.373630389881236091, -17.32815070419105297 ) ) ;
#5286 = VECTOR ( 'NONE', #16455, 1000.000000000000000 ) ;
#5287 = EDGE_LOOP ( 'NONE', ( #25747, #27176, #5955, #9495 ) ) ;
#5288 = PLANE ( 'NONE',  #13769 ) ;
#5289 = VECTOR ( 'NONE', #9423, 1000.000000000000000 ) ;
#5290 = EDGE_CURVE ( 'NONE', #24650, #30115, #11510, .T. ) ;
#5291 = VECTOR ( 'NONE', #28598, 1000.000000000000000 ) ;
#5293 = ORIENTED_EDGE ( 'NONE', *, *, #26892, .T. ) ;
#5292 = CARTESIAN_POINT ( 'NONE',  ( 139.7287565553230309, -4.999999999999980460, -33.82050807568879947 ) ) ;
#5294 = EDGE_CURVE ( 'NONE', #27047, #24269, #9679, .T. ) ;
#5295 = EDGE_CURVE ( 'NONE', #2569, #1403, #13802, .T. ) ;
#5296 = LINE ( 'NONE', #7882, #225 ) ;
#5297 = EDGE_CURVE ( 'NONE', #28729, #17627, #18546, .T. ) ;
#5298 = CARTESIAN_POINT ( 'NONE',  ( 174.7287565553228887, -9.999999999999994671, -16.50000000000000355 ) ) ;
#5299 = CARTESIAN_POINT ( 'NONE',  ( 35.97124720801268438, -19.59080293283771823, -20.41544573823858144 ) ) ;
#5300 = CARTESIAN_POINT ( 'NONE',  ( 12.76023694501680517, 7.627675785621035764, -14.92276157399860281 ) ) ;
#5301 = CARTESIAN_POINT ( 'NONE',  ( 37.54859390953724585, -22.18451583373416014, -36.50100000000000477 ) ) ;
#5302 = CARTESIAN_POINT ( 'NONE',  ( 134.5152310637605808, -1.999999999999980460, -11.28819510263909187 ) ) ;
#5303 = CARTESIAN_POINT ( 'NONE',  ( 12.02748425217687789, 9.318634685891279190, -16.69156549717016702 ) ) ;
#5304 = PLANE ( 'NONE',  #4883 ) ;
#5305 = CARTESIAN_POINT ( 'NONE',  ( 5.200000000000002842, 0.000000000000000000, 2.500000000000000888 ) ) ;
#5306 = ORIENTED_EDGE ( 'NONE', *, *, #13528, .F. ) ;
#5307 = VECTOR ( 'NONE', #22043, 1000.000000000000000 ) ;
#5308 = DIRECTION ( 'NONE',  ( 1.110223024625156540E-16, 2.995891024602366092E-32, 1.000000000000000000 ) ) ;
#5309 = DIRECTION ( 'NONE',  ( -2.698458740408365879E-16, 1.000000000000000000, 0.000000000000000000 ) ) ;
#5310 = ORIENTED_EDGE ( 'NONE', *, *, #17546, .T. ) ;
#5311 = EDGE_LOOP ( 'NONE', ( #6369, #9791, #18350 ) ) ;
#5312 = AXIS2_PLACEMENT_3D ( 'NONE', #9738, #19056, #28412 ) ;
#5313 = ORIENTED_EDGE ( 'NONE', *, *, #20289, .F. ) ;
#5314 = CARTESIAN_POINT ( 'NONE',  ( 11.22387317355479475, 9.091340879052031809, -17.24161325043666082 ) ) ;
#5315 = CARTESIAN_POINT ( 'NONE',  ( 25.84319962709097140, -7.021413190281159622, -18.98986798778381058 ) ) ;
#5316 = CARTESIAN_POINT ( 'NONE',  ( 23.07678757892180244, -0.1267571646896241688, -14.23703129728563965 ) ) ;
#5317 = DIRECTION ( 'NONE',  ( 1.000000000000000000, 0.000000000000000000, 0.000000000000000000 ) ) ;
#5318 = PLANE ( 'NONE',  #29735 ) ;
#5319 = DIRECTION ( 'NONE',  ( 2.908569913943825554E-16, -1.000000000000000000, 0.000000000000000000 ) ) ;
#5320 = EDGE_CURVE ( 'NONE', #15263, #11825, #11819, .T. ) ;
#5321 = ORIENTED_EDGE ( 'NONE', *, *, #21642, .T. ) ;
#5322 = LINE ( 'NONE', #14612, #23547 ) ;
#5323 = CARTESIAN_POINT ( 'NONE',  ( 108.6946756682487774, -4.999999999999987566, -78.97130444073225419 ) ) ;
#5324 = AXIS2_PLACEMENT_3D ( 'NONE', #26751, #19841, #13127 ) ;
#5326 = ORIENTED_EDGE ( 'NONE', *, *, #8582, .F. ) ;
#5325 = CARTESIAN_POINT ( 'NONE',  ( 133.7287565553229456, -4.999999999999982236, 3.500000000000003109 ) ) ;
#5327 = EDGE_CURVE ( 'NONE', #5386, #4109, #21284, .T. ) ;
#5328 = EDGE_CURVE ( 'NONE', #26561, #10839, #11667, .T. ) ;
#5329 = PLANE ( 'NONE',  #12197 ) ;
#5330 = DIRECTION ( 'NONE',  ( 1.110223024625156540E-16, 2.995891024602366092E-32, 1.000000000000000000 ) ) ;
#5331 = EDGE_CURVE ( 'NONE', #5737, #28689, #6961, .T. ) ;
#5332 = VECTOR ( 'NONE', #16739, 1000.000000000000000 ) ;
#5333 = EDGE_CURVE ( 'NONE', #4933, #13070, #18701, .T. ) ;
#5334 = CARTESIAN_POINT ( 'NONE',  ( 12.02805304935487563, 9.316025821727821565, -16.69133030147860453 ) ) ;
#5335 = FACE_OUTER_BOUND ( 'NONE', #20108, .T. ) ;
#5336 = CARTESIAN_POINT ( 'NONE',  ( 32.68951927270060764, -11.07419627511998605, -18.48540492261787449 ) ) ;
#5337 = EDGE_LOOP ( 'NONE', ( #17433, #15477, #14331, #20210 ) ) ;
#5338 = CARTESIAN_POINT ( 'NONE',  ( 13.38138208201938895, 7.626735917299793499, -15.70646184538344770 ) ) ;
#5339 = DIRECTION ( 'NONE',  ( 0.000000000000000000, 0.000000000000000000, -1.000000000000000000 ) ) ;
#5340 = CARTESIAN_POINT ( 'NONE',  ( 25.73595588610537277, -4.826321120321507507, -18.84379041344559269 ) ) ;
#5341 = CARTESIAN_POINT ( 'NONE',  ( 12.31353044564305499, 11.91954703646417713, -16.35554902986205761 ) ) ;
#5342 = DIRECTION ( 'NONE',  ( 8.163404592832029035E-16, 2.202861047501738386E-31, 1.000000000000000000 ) ) ;
#5343 = VERTEX_POINT ( 'NONE', #14102 ) ;
#5344 = CARTESIAN_POINT ( 'NONE',  ( 11.34314632229486364, 9.864239995495806212, -15.91456019135469013 ) ) ;
#5345 = DIRECTION ( 'NONE',  ( -2.698458740408365879E-16, 1.000000000000000000, 0.000000000000000000 ) ) ;
#5346 = CARTESIAN_POINT ( 'NONE',  ( 9.917332382238186028, 16.40320447359955125, -16.50418441153501448 ) ) ;
#5347 = CARTESIAN_POINT ( 'NONE',  ( 154.5152310637605524, -10.00000000000000000, -19.94844914048349693 ) ) ;
#5348 = ORIENTED_EDGE ( 'NONE', *, *, #19315, .F. ) ;
#5349 = CARTESIAN_POINT ( 'NONE',  ( 143.6922820468854241, -10.00000000000000355, -9.266330736598359152 ) ) ;
#5350 = EDGE_LOOP ( 'NONE', ( #16424, #10741, #20017, #21684, #1618 ) ) ;
#5351 = CARTESIAN_POINT ( 'NONE',  ( 12.02710433905669341, 9.320377015888107408, -16.69172260460959478 ) ) ;
#5352 = VERTEX_POINT ( 'NONE', #246 ) ;
#5353 = VECTOR ( 'NONE', #28123, 1000.000000000000000 ) ;
#5354 = CARTESIAN_POINT ( 'NONE',  ( 34.13391181137448882, -12.33661648534566524, -20.90239171999057888 ) ) ;
#5355 = CARTESIAN_POINT ( 'NONE',  ( 15.47706244943930010, 8.830671366982906889, -20.22835218371243471 ) ) ;
#5356 = CARTESIAN_POINT ( 'NONE',  ( 17.20878921875063838, 11.12208594754616975, -17.23123872766219833 ) ) ;
#5357 = ORIENTED_EDGE ( 'NONE', *, *, #5434, .F. ) ;
#5358 = VECTOR ( 'NONE', #6315, 1000.000000000000114 ) ;
#5359 = LINE ( 'NONE', #19381, #5749 ) ;
#5360 = VECTOR ( 'NONE', #25155, 1000.000000000000000 ) ;
#5361 = CIRCLE ( 'NONE', #2453, 5.000000000000000000 ) ;
#5362 = LINE ( 'NONE', #21533, #25442 ) ;
#5363 = ITEM_DEFINED_TRANSFORMATION ( 'NONE', 'NONE', #22435,  #13190 ) ;
#5364 = CARTESIAN_POINT ( 'NONE',  ( 17.81405000127377747, 1.596365152898254980, -17.08637312321770096 ) ) ;
#5365 = CARTESIAN_POINT ( 'NONE',  ( 15.70491959545049987, 3.570626008024105680, -15.63470537622339229 ) ) ;
#5366 = PLANE ( 'NONE',  #305 ) ;
#5367 = FACE_BOUND ( 'NONE', #18828, .T. ) ;
#5368 = EDGE_CURVE ( 'NONE', #280, #25774, #9522, .T. ) ;
#5369 = AXIS2_PLACEMENT_3D ( 'NONE', #7204, #30153, #12064 ) ;
#5370 = EDGE_CURVE ( 'NONE', #1829, #18677, #11369, .T. ) ;
#5371 = DIRECTION ( 'NONE',  ( -0.8090169943749474513, -2.183098979609982436E-16, 0.5877852522924731371 ) ) ;
#5372 = CARTESIAN_POINT ( 'NONE',  ( 167.0152310637605240, -1.999999999999970468, -34.70218595412750773 ) ) ;
#5373 = AXIS2_PLACEMENT_3D ( 'NONE', #16405, #13952, #92 ) ;
#5374 = LINE ( 'NONE', #644, #17496 ) ;
#5375 = LINE ( 'NONE', #5063, #29555 ) ;
#5376 = VECTOR ( 'NONE', #10117, 1000.000000000000000 ) ;
#5377 = CARTESIAN_POINT ( 'NONE',  ( 12.21210587983259366, 9.791837354264822935, -15.33748854281299323 ) ) ;
#5378 = LINE ( 'NONE', #5678, #26551 ) ;
#5379 = CARTESIAN_POINT ( 'NONE',  ( 129.5152310637605524, -10.00000000000000888, -13.05155085951650840 ) ) ;
#5380 = ORIENTED_EDGE ( 'NONE', *, *, #685, .T. ) ;
#5381 = CARTESIAN_POINT ( 'NONE',  ( 11.50832337395308436, 9.139936167900076569, -15.84372008594036885 ) ) ;
#5382 = CARTESIAN_POINT ( 'NONE',  ( 16.25879716139461095, 4.256374150336979412, -17.55500201710977137 ) ) ;
#5383 = CARTESIAN_POINT ( 'NONE',  ( 149.5152310637605524, -10.00000000000000178, -21.71180489736091346 ) ) ;
#5384 = CARTESIAN_POINT ( 'NONE',  ( 171.1922820468853672, -1.999999999999970024, -30.91696583120936026 ) ) ;
#5385 = DIRECTION ( 'NONE',  ( 0.3090169943749472292, 8.338696094057992503E-17, -0.9510565162951536422 ) ) ;
#5386 = VERTEX_POINT ( 'NONE', #9069 ) ;
#5387 = DIRECTION ( 'NONE',  ( -0.8090169943749474513, -2.183098979609982436E-16, -0.5877852522924731371 ) ) ;
#5388 = CARTESIAN_POINT ( 'NONE',  ( 12.83223741744420288, 9.540690758033102625, -16.14104544935691976 ) ) ;
#5389 = ORIENTED_EDGE ( 'NONE', *, *, #5929, .T. ) ;
#5391 = VECTOR ( 'NONE', #17269, 1000.000000000000000 ) ;
#5390 = CARTESIAN_POINT ( 'NONE',  ( 35.32370156268159178, -20.17419364810216109, -19.24765216636316723 ) ) ;
#5392 = CARTESIAN_POINT ( 'NONE',  ( 17.66155849027303049, 7.702290371990539342, -14.74052880078125760 ) ) ;
#5393 = ORIENTED_EDGE ( 'NONE', *, *, #19857, .F. ) ;
#5394 = CARTESIAN_POINT ( 'NONE',  ( 130.7287565553229456, -9.999999999999982236, 0.5000000000000052180 ) ) ;
#5395 = CARTESIAN_POINT ( 'NONE',  ( 14.50439321891314925, 5.533609182599570353, -15.17065254761420512 ) ) ;
#5396 = ORIENTED_EDGE ( 'NONE', *, *, #17148, .T. ) ;
#5397 = CARTESIAN_POINT ( 'NONE',  ( 130.7287565553229456, -9.999999999999982236, 3.500000000000003109 ) ) ;
#5398 = EDGE_CURVE ( 'NONE', #18781, #22599, #28816, .T. ) ;
#5399 = AXIS2_PLACEMENT_3D ( 'NONE', #22865, #4244, #24709 ) ;
#5400 = CARTESIAN_POINT ( 'NONE',  ( 20.49605984403359216, -1.259233478192978373, -14.44550164344372511 ) ) ;
#5401 = CARTESIAN_POINT ( 'NONE',  ( 18.26505246421942275, 9.297698622231314047, -17.43849025199569169 ) ) ;
#5402 = CARTESIAN_POINT ( 'NONE',  ( 166.1922820468853388, -9.999999999999998224, -10.74328820663507678 ) ) ;
#5403 = ORIENTED_EDGE ( 'NONE', *, *, #9926, .T. ) ;
#5404 = ORIENTED_EDGE ( 'NONE', *, *, #24061, .T. ) ;
#5405 = CARTESIAN_POINT ( 'NONE',  ( 169.5152310637604103, -9.999999999999996447, -4.391296821672111328 ) ) ;
#5406 = ORIENTED_EDGE ( 'NONE', *, *, #2234, .F. ) ;
#5407 = CARTESIAN_POINT ( 'NONE',  ( 5.637851296924623057E-15, 9.237604307034036566, -0.7145311798163362926 ) ) ;
#5408 = VECTOR ( 'NONE', #24087, 1000.000000000000000 ) ;
#5409 = CARTESIAN_POINT ( 'NONE',  ( 138.6922820468854525, -1.999999999999979572, -35.24709285013155835 ) ) ;
#5410 = LINE ( 'NONE', #21726, #24307 ) ;
#5411 = VECTOR ( 'NONE', #8491, 1000.000000000000000 ) ;
#5412 = CARTESIAN_POINT ( 'NONE',  ( 104.9993066664142702, -4.999999999999988454, -76.28646170422676676 ) ) ;
#5413 = CARTESIAN_POINT ( 'NONE',  ( 11.50832337395308436, 9.139936167900076569, -15.84372008594036885 ) ) ;
#5414 = CARTESIAN_POINT ( 'NONE',  ( 25.59095072769168766, -7.385909681514642777, -13.40699837787023618 ) ) ;
#5415 = CARTESIAN_POINT ( 'NONE',  ( 30.27313844582349489, -8.115497507854934511, -14.41531361995715876 ) ) ;
#5417 = ORIENTED_EDGE ( 'NONE', *, *, #17404, .F. ) ;
#5416 = CARTESIAN_POINT ( 'NONE',  ( 35.54859390953724585, -23.18451583373416014, -16.94733705004010105 ) ) ;
#5418 = DIRECTION ( 'NONE',  ( 0.000000000000000000, -2.775557561562890735E-17, 1.000000000000000000 ) ) ;
#5419 = CARTESIAN_POINT ( 'NONE',  ( 133.6922820468854241, -10.00000000000000711, -32.39392330124607611 ) ) ;
#5420 = CARTESIAN_POINT ( 'NONE',  ( 147.0152310637604955, -4.999999999999977796, -0.06116980274991495881 ) ) ;
#5421 = DIRECTION ( 'NONE',  ( 0.9510565162951536422, 0.000000000000000000, -0.3090169943749475623 ) ) ;
#5422 = CYLINDRICAL_SURFACE ( 'NONE', #1062, 4.000000000000000000 ) ;
#5423 = DIRECTION ( 'NONE',  ( 0.9510565162951535312, 2.566386769018988816E-16, -0.3090169943749475623 ) ) ;
#5424 = CARTESIAN_POINT ( 'NONE',  ( 17.36512755686010934, 0.5347363583120325892, -15.24149349723765390 ) ) ;
#5425 = CARTESIAN_POINT ( 'NONE',  ( 146.1922820468853956, -10.00000000000000355, -4.936203717676158398 ) ) ;
#5426 = CARTESIAN_POINT ( 'NONE',  ( 12.27567800861033120, 9.500287468128719937, -15.31119923128196625 ) ) ;
#5427 = DIRECTION ( 'NONE',  ( 0.9510565162951536422, 2.566386769018988816E-16, 0.3090169943749472292 ) ) ;
#5428 = CARTESIAN_POINT ( 'NONE',  ( 147.2287565553230024, -4.999999999999977796, -12.16987298107780013 ) ) ;
#5429 = CARTESIAN_POINT ( 'NONE',  ( 17.18819971663578272, 0.8441372818425427749, -18.45219435416397502 ) ) ;
#5430 = CARTESIAN_POINT ( 'NONE',  ( 13.23210690081759111, 9.952263081781872245, -14.54667289943505004 ) ) ;
#5431 = ORIENTED_EDGE ( 'NONE', *, *, #9761, .T. ) ;
#5433 = VECTOR ( 'NONE', #10011, 1000.000000000000000 ) ;
#5432 = CARTESIAN_POINT ( 'NONE',  ( 33.47012763672258728, -12.84706786418751534, -19.72967806864707541 ) ) ;
#5434 = EDGE_CURVE ( 'NONE', #12418, #13408, #28507, .T. ) ;
#5435 = CARTESIAN_POINT ( 'NONE',  ( 0.000000000000000000, 0.000000000000000000, 0.000000000000000000 ) ) ;
#5436 = CARTESIAN_POINT ( 'NONE',  ( 24.24063474714532873, -9.755679120534059834, -13.19378374426895206 ) ) ;
#5437 = VECTOR ( 'NONE', #6781, 1000.000000000000000 ) ;
#5438 = EDGE_CURVE ( 'NONE', #8637, #3882, #14708, .T. ) ;
#5439 = CARTESIAN_POINT ( 'NONE',  ( 17.06466135374324011, 3.680263393506696179, -18.28590298471088005 ) ) ;
#5440 = ORIENTED_EDGE ( 'NONE', *, *, #12648, .F. ) ;
#5441 = ORIENTED_EDGE ( 'NONE', *, *, #2251, .T. ) ;
#5442 = B_SPLINE_CURVE_WITH_KNOTS ( 'NONE', 3,
 ( #20566, #13838, #15986, #20708, #16139, #11545 ),
 .UNSPECIFIED., .F., .F.,
 ( 4, 2, 4 ),
 ( 0.002336974151641585049, 0.003500975885716457129, 0.004664977619791329209 ),
 .UNSPECIFIED. ) ;
#5443 = CARTESIAN_POINT ( 'NONE',  ( 167.0152310637604955, -4.999999999999972466, -15.61832212156129707 ) ) ;
#5444 = EDGE_LOOP ( 'NONE', ( #22931, #25946, #40, #17730 ) ) ;
#5446 = ORIENTED_EDGE ( 'NONE', *, *, #26971, .F. ) ;
#5445 = DIRECTION ( 'NONE',  ( 1.000000000000000000, 0.000000000000000000, 0.000000000000000000 ) ) ;
#5447 = DIRECTION ( 'NONE',  ( 0.000000000000000000, 0.000000000000000000, -1.000000000000000000 ) ) ;
#5448 = DIRECTION ( 'NONE',  ( -2.698458740408365879E-16, 1.000000000000000000, 0.000000000000000000 ) ) ;
#5449 = PLANE ( 'NONE',  #1973 ) ;
#5450 = CARTESIAN_POINT ( 'NONE',  ( 36.30362226317071617, -21.08398799169651738, -20.22680612736627026 ) ) ;
#5451 = CARTESIAN_POINT ( 'NONE',  ( 9.915973561396301150, 16.40943619918981256, -16.50475030878699556 ) ) ;
#5452 = DIRECTION ( 'NONE',  ( -0.000000000000000000, -0.000000000000000000, 1.000000000000000000 ) ) ;
#5453 = DIRECTION ( 'NONE',  ( 0.5877852522924731371, 1.586114251531760728E-16, -0.8090169943749474513 ) ) ;
#5454 = CARTESIAN_POINT ( 'NONE',  ( 13.01452397926061089, 8.532813591658360508, -15.99807864679971026 ) ) ;
#5455 = CARTESIAN_POINT ( 'NONE',  ( 9.884967449281287344, -8.443187699361503817, -15.00000000000000000 ) ) ;
#5456 = CARTESIAN_POINT ( 'NONE',  ( 157.0152310637604955, -10.00000000000000000, -17.38167787843871182 ) ) ;
#5457 = ORIENTED_EDGE ( 'NONE', *, *, #5545, .F. ) ;
#5458 = CARTESIAN_POINT ( 'NONE',  ( 0.000000000000000000, 0.000000000000000000, 1.700000000000000178 ) ) ;
#5459 = DIRECTION ( 'NONE',  ( 0.9510565162951535312, 2.566386769018988816E-16, -0.3090169943749475623 ) ) ;
#5460 = VERTEX_POINT ( 'NONE', #3434 ) ;
#5461 = LINE ( 'NONE', #3626, #21476 ) ;
#5462 = ORIENTED_EDGE ( 'NONE', *, *, #4535, .T. ) ;
#5463 = ORIENTED_EDGE ( 'NONE', *, *, #11516, .T. ) ;
#5464 = CARTESIAN_POINT ( 'NONE',  ( 13.31307029362551475, 7.598550302509940124, -15.76075481184169647 ) ) ;
#5465 = EDGE_LOOP ( 'NONE', ( #2451, #5137, #11933, #27372 ) ) ;
#5466 = ADVANCED_FACE ( 'NONE', ( #29108 ), #5422, .F. ) ;
#5467 = CARTESIAN_POINT ( 'NONE',  ( 15.41555982967951444, 8.269517134526982005, -21.14450021912286104 ) ) ;
#5468 = EDGE_CURVE ( 'NONE', #10339, #21691, #22048, .T. ) ;
#5469 = CARTESIAN_POINT ( 'NONE',  ( 26.68716238812262631, -2.792712658874448639, -18.04699283665395981 ) ) ;
#5470 = DIRECTION ( 'NONE',  ( -2.698458740408365879E-16, 1.000000000000000000, 0.000000000000000000 ) ) ;
#5471 = DIRECTION ( 'NONE',  ( -0.5877852522924731371, -1.586114251531760235E-16, 0.8090169943749474513 ) ) ;
#5472 = VECTOR ( 'NONE', #26276, 1000.000000000000000 ) ;
#5473 = ADVANCED_FACE ( 'NONE', ( #17163 ), #12726, .T. ) ;
#5474 = CARTESIAN_POINT ( 'NONE',  ( 144.7287565553229740, -4.999999999999978684, 0.8205080756888000204 ) ) ;
#5475 = DIRECTION ( 'NONE',  ( -0.8090169943749474513, -2.183098979609982436E-16, 0.5877852522924731371 ) ) ;
#5476 = DIRECTION ( 'NONE',  ( 0.5877852522924731371, 1.586114251531760728E-16, 0.8090169943749474513 ) ) ;
#5477 = DIRECTION ( 'NONE',  ( 0.3090169943749475623, 8.338696094058001131E-17, 0.9510565162951536422 ) ) ;
#5478 = CIRCLE ( 'NONE', #16208, 12.50000000000000000 ) ;
#5479 = FACE_OUTER_BOUND ( 'NONE', #28221, .T. ) ;
#5480 = DIRECTION ( 'NONE',  ( 1.000000000000000000, 0.000000000000000000, 0.000000000000000000 ) ) ;
#5481 = CARTESIAN_POINT ( 'NONE',  ( 10.47212132250356120, 16.45172734403231729, -17.33476278219207956 ) ) ;
#5482 = CARTESIAN_POINT ( 'NONE',  ( 35.54502023521215648, -22.16846120802060938, -18.59538644662325524 ) ) ;
#5483 = ORIENTED_EDGE ( 'NONE', *, *, #10564, .T. ) ;
#5484 = CARTESIAN_POINT ( 'NONE',  ( 8.944584683310379702, 16.95159276115599667, -17.91752729848688830 ) ) ;
#5485 = VECTOR ( 'NONE', #8648, 1000.000000000000000 ) ;
#5486 = CARTESIAN_POINT ( 'NONE',  ( 26.87257363757477435, -3.324124212371978082, -16.68573618535388547 ) ) ;
#5487 = CARTESIAN_POINT ( 'NONE',  ( 12.86785267122296794, 9.515866005961482799, -16.11575320936711364 ) ) ;
#5488 = FACE_BOUND ( 'NONE', #11156, .T. ) ;
#5489 = EDGE_CURVE ( 'NONE', #22161, #24130, #28872, .T. ) ;
#5490 = VERTEX_POINT ( 'NONE', #19740 ) ;
#5491 = CARTESIAN_POINT ( 'NONE',  ( 11.47288049726737214, 9.269262779257836371, -15.86091052746238184 ) ) ;
#5492 = LINE ( 'NONE', #14775, #20387 ) ;
#5493 = CARTESIAN_POINT ( 'NONE',  ( 12.43696608443014284, 8.546664718661613591, -15.18012293544581226 ) ) ;
#5494 = DIRECTION ( 'NONE',  ( -2.698458740408365879E-16, 1.000000000000000000, 0.000000000000000000 ) ) ;
#5495 = EDGE_LOOP ( 'NONE', ( #17701, #11171, #16511 ) ) ;
#5496 = CARTESIAN_POINT ( 'NONE',  ( 164.7287565553228887, -9.999999999999998224, -7.839745962155603820 ) ) ;
#5497 = ORIENTED_EDGE ( 'NONE', *, *, #25324, .F. ) ;
#5498 = CARTESIAN_POINT ( 'NONE',  ( 12.02859841272590735, 9.313533661810568631, -16.69110409223909741 ) ) ;
#5499 = VERTEX_POINT ( 'NONE', #1150 ) ;
#5500 = EDGE_CURVE ( 'NONE', #29186, #16077, #4945, .T. ) ;
#5501 = CARTESIAN_POINT ( 'NONE',  ( 36.40320260674921116, -22.53134972621836241, -20.30234751949853589 ) ) ;
#5502 = CARTESIAN_POINT ( 'NONE',  ( 29.66490191837812773, -8.365349891895018430, -17.62461620872172574 ) ) ;
#5503 = CARTESIAN_POINT ( 'NONE',  ( 15.47706244943930010, 8.830671366982906889, -20.22835218371243471 ) ) ;
#5504 = VECTOR ( 'NONE', #24251, 1000.000000000000000 ) ;
#5505 = EDGE_CURVE ( 'NONE', #12263, #18517, #843, .T. ) ;
#5506 = CARTESIAN_POINT ( 'NONE',  ( 7.497985849899103883, -5.000000000000015987, 23.07642761220746053 ) ) ;
#5507 = VERTEX_POINT ( 'NONE', #26645 ) ;
#5508 = EDGE_CURVE ( 'NONE', #16977, #7341, #12572, .T. ) ;
#5509 = ORIENTED_EDGE ( 'NONE', *, *, #4362, .F. ) ;
#5510 = EDGE_CURVE ( 'NONE', #20748, #22102, #17455, .T. ) ;
#5511 = EDGE_CURVE ( 'NONE', #7152, #24650, #23744, .T. ) ;
#5512 = CARTESIAN_POINT ( 'NONE',  ( 157.0152310637605240, -1.999999999999973577, -26.04193191628311155 ) ) ;
#5513 = CONTEXT_DEPENDENT_SHAPE_REPRESENTATION ( #19229, #15437 ) ;
#5514 = EDGE_LOOP ( 'NONE', ( #3897, #25611, #20574, #6740 ) ) ;
#5515 = CARTESIAN_POINT ( 'NONE',  ( 21.26848695057635297, 1.468789200266592099, -19.53654423682621299 ) ) ;
#5516 = CARTESIAN_POINT ( 'NONE',  ( 17.78594395145776019, 10.14170102421038422, -17.68001733040774681 ) ) ;
#5517 = VECTOR ( 'NONE', #20251, 1000.000000000000000 ) ;
#5518 = CARTESIAN_POINT ( 'NONE',  ( 158.6922820468853672, -1.999999999999974021, -17.92658477444275889 ) ) ;
#5519 = FACE_BOUND ( 'NONE', #29648, .T. ) ;
#5520 = PLANE ( 'NONE',  #8187 ) ;
#5521 = CARTESIAN_POINT ( 'NONE',  ( 167.0152310637604955, -9.999999999999996447, -26.04193191628311155 ) ) ;
#5522 = CARTESIAN_POINT ( 'NONE',  ( 2.500000000000000444, 1.178949249685215417, -2.042000000000002036 ) ) ;
#5523 = CARTESIAN_POINT ( 'NONE',  ( 169.5152310637604103, -4.999999999999971578, -4.391296821672111328 ) ) ;
#5524 = CARTESIAN_POINT ( 'NONE',  ( 12.27630411038995106, 9.497004473356668086, -15.31097170929839812 ) ) ;
#5525 = CARTESIAN_POINT ( 'NONE',  ( 138.6922820468854525, -1.999999999999979572, -23.73366926340167282 ) ) ;
#5526 = DIRECTION ( 'NONE',  ( 0.3090169943749475623, 8.338696094058001131E-17, 0.9510565162951536422 ) ) ;
#5527 = VERTEX_POINT ( 'NONE', #12127 ) ;
#5528 = CARTESIAN_POINT ( 'NONE',  ( 12.52778158092594474, 8.582979361647906202, -15.10803260229456946 ) ) ;
#5529 = ORIENTED_EDGE ( 'NONE', *, *, #29253, .F. ) ;
#5530 = VECTOR ( 'NONE', #12749, 1000.000000000000000 ) ;
#5531 = CARTESIAN_POINT ( 'NONE',  ( 17.18298215709098287, 1.908350159885260799, -18.42911670940388902 ) ) ;
#5532 = CARTESIAN_POINT ( 'NONE',  ( -20.00000000000017053, 34.64101615137744972, -10.00000000000000000 ) ) ;
#5533 = LINE ( 'NONE', #5384, #12043 ) ;
#5535 = ORIENTED_EDGE ( 'NONE', *, *, #3478, .F. ) ;
#5534 = DIRECTION ( 'NONE',  ( 0.9510565162951536422, 2.566386769018988816E-16, 0.3090169943749472292 ) ) ;
#5536 = VERTEX_POINT ( 'NONE', #5269 ) ;
#5537 = DIRECTION ( 'NONE',  ( 1.000000000000000000, 0.000000000000000000, 0.000000000000000000 ) ) ;
#5538 = EDGE_LOOP ( 'NONE', ( #1050, #25690, #2554, #15574 ) ) ;
#5539 = CARTESIAN_POINT ( 'NONE',  ( 12.83236877538120524, 9.540106609504201529, -16.14098973436422568 ) ) ;
#5540 = CARTESIAN_POINT ( 'NONE',  ( 34.75280465199809043, -13.11698595563971459, -19.00481823564506101 ) ) ;
#5541 = CARTESIAN_POINT ( 'NONE',  ( 15.94478687392618355, 4.193953704849600506, -19.05305658475056063 ) ) ;
#5542 = VERTEX_POINT ( 'NONE', #14556 ) ;
#5543 = ORIENTED_EDGE ( 'NONE', *, *, #17232, .T. ) ;
#5544 = ORIENTED_EDGE ( 'NONE', *, *, #18205, .F. ) ;
#5545 = EDGE_CURVE ( 'NONE', #17674, #7452, #19593, .T. ) ;
#5546 = ORIENTED_EDGE ( 'NONE', *, *, #24561, .T. ) ;
#5547 = LINE ( 'NONE', #12699, #3810 ) ;
#5548 = CARTESIAN_POINT ( 'NONE',  ( 17.27944038698359464, 10.59897317215052226, -14.78577975581568360 ) ) ;
#5549 = ADVANCED_FACE ( 'NONE', ( #17306 ), #19296, .F. ) ;
#5550 = ORIENTED_EDGE ( 'NONE', *, *, #7162, .T. ) ;
#5551 = EDGE_CURVE ( 'NONE', #3893, #2706, #7325, .T. ) ;
#5552 = CYLINDRICAL_SURFACE ( 'NONE', #4708, 12.50000000000000000 ) ;
#5553 = ORIENTED_EDGE ( 'NONE', *, *, #19314, .T. ) ;
#5554 = CARTESIAN_POINT ( 'NONE',  ( 26.84208138670940968, -2.489200896322508516, -17.35162900556907317 ) ) ;
#5555 = CARTESIAN_POINT ( 'NONE',  ( 18.23559491442917135, -2.176271773050306724, -15.57877364869929515 ) ) ;
#5556 = EDGE_LOOP ( 'NONE', ( #3191, #25186, #25550, #16516 ) ) ;
#5557 = CARTESIAN_POINT ( 'NONE',  ( 100.8158076689448990, -4.999999999999990230, 73.24697176669747023 ) ) ;
#5558 = VECTOR ( 'NONE', #15373, 1000.000000000000000 ) ;
#5559 = PLANE ( 'NONE',  #20139 ) ;
#5560 = CARTESIAN_POINT ( 'NONE',  ( 177.2287565553228603, -9.999999999999994671, -12.16987298107780369 ) ) ;
#5561 = DIRECTION ( 'NONE',  ( -2.698458740408365879E-16, 1.000000000000000000, 0.000000000000000000 ) ) ;
#5562 = DIRECTION ( 'NONE',  ( 0.000000000000000000, 0.000000000000000000, 1.000000000000000000 ) ) ;
#5563 = CARTESIAN_POINT ( 'NONE',  ( 11.48890098693651396, 9.204103201752445784, -15.85365151319587440 ) ) ;
#5564 = CARTESIAN_POINT ( 'NONE',  ( 28.68006932781580076, -6.484681432979621185, -16.07205306641353104 ) ) ;
#5565 = CARTESIAN_POINT ( 'NONE',  ( 28.56280713547801398, -4.978584871567802494, -14.74258920993753641 ) ) ;
#5566 = ADVANCED_FACE ( 'NONE', ( #7706 ), #12277, .T. ) ;
#5568 = VERTEX_POINT ( 'NONE', #19446 ) ;
#5567 = CARTESIAN_POINT ( 'NONE',  ( 34.99076264053043417, -20.67847543353016349, -21.19169145379677488 ) ) ;
#5569 = DIRECTION ( 'NONE',  ( -2.698458740408365879E-16, 1.000000000000000000, 0.000000000000000000 ) ) ;
#5570 = CARTESIAN_POINT ( 'NONE',  ( 25.00000000000001066, 60.00000000000000711, 24.99999999999998579 ) ) ;
#5571 = DIRECTION ( 'NONE',  ( -0.000000000000000000, -0.000000000000000000, -1.000000000000000000 ) ) ;
#5572 = CARTESIAN_POINT ( 'NONE',  ( -4.680456609903995258, -6.535341423375610859, -4.983111142572218100 ) ) ;
#5573 = CARTESIAN_POINT ( 'NONE',  ( 172.7287565553229456, -1.999999999999970468, -39.49999999999997868 ) ) ;
#5574 = DIRECTION ( 'NONE',  ( 0.9510565162951535312, 2.566386769018988816E-16, -0.3090169943749475623 ) ) ;
#5575 = CARTESIAN_POINT ( 'NONE',  ( 21.63873165585565417, 2.424707942738766331, -13.54651715722292060 ) ) ;
#5576 = ORIENTED_EDGE ( 'NONE', *, *, #10661, .T. ) ;
#5577 = CARTESIAN_POINT ( 'NONE',  ( 420.0000000000002274, 34.64101615137744972, 14.00000000000000178 ) ) ;
#5578 = CARTESIAN_POINT ( 'NONE',  ( 12.26883957244698387, 9.531649408071682927, -15.31402716519172635 ) ) ;
#5579 = CARTESIAN_POINT ( 'NONE',  ( 32.89062095351589932, -11.25267498498577723, -18.96775996542842435 ) ) ;
#5580 = DIRECTION ( 'NONE',  ( 0.3090169943749475623, 8.338696094058001131E-17, 0.9510565162951536422 ) ) ;
#5581 = CARTESIAN_POINT ( 'NONE',  ( 25.45462155318426767, -0.2439708902934435431, -15.99927030562601438 ) ) ;
#5582 = AXIS2_PLACEMENT_3D ( 'NONE', #19319, #28986, #19172 ) ;
#5583 = CARTESIAN_POINT ( 'NONE',  ( 22.15888525254269581, 3.701285330253634154, -19.09944157575669621 ) ) ;
#5584 = ORIENTED_EDGE ( 'NONE', *, *, #20407, .F. ) ;
#5585 = ADVANCED_FACE ( 'NONE', ( #25087 ), #24637, .T. ) ;
#5586 = CARTESIAN_POINT ( 'NONE',  ( 33.37634376253905089, -12.42895282922877342, -19.69946502924221932 ) ) ;
#5587 = SURFACE_STYLE_FILL_AREA ( #26505 ) ;
#5588 = CARTESIAN_POINT ( 'NONE',  ( 25.30932029414111284, -7.960302465696846852, -19.79224777486898645 ) ) ;
#5589 = CARTESIAN_POINT ( 'NONE',  ( 23.51547714073238282, 0.8170344765809651744, -13.87895193235286051 ) ) ;
#5590 = CARTESIAN_POINT ( 'NONE',  ( 24.52797215547132836, -1.897736678990579184, -19.26084780660264073 ) ) ;
#5591 = ORIENTED_EDGE ( 'NONE', *, *, #11689, .F. ) ;
#5592 = DIRECTION ( 'NONE',  ( 0.000000000000000000, 0.5000000000000012212, 0.8660254037844380415 ) ) ;
#5593 = VERTEX_POINT ( 'NONE', #11186 ) ;
#5594 = CARTESIAN_POINT ( 'NONE',  ( 156.1922820468853388, -1.999999999999975353, -4.936203717676158398 ) ) ;
#5595 = LINE ( 'NONE', #28985, #15984 ) ;
#5596 = DIRECTION ( 'NONE',  ( -0.9510565162951536422, 0.000000000000000000, -0.3090169943749472292 ) ) ;
#5597 = AXIS2_PLACEMENT_3D ( 'NONE', #2672, #16707, #19432 ) ;
#5598 = CARTESIAN_POINT ( 'NONE',  ( 176.1922820468853388, -1.999999999999968914, -30.91696583120936026 ) ) ;
#5599 = EDGE_CURVE ( 'NONE', #28522, #13253, #11039, .T. ) ;
#5600 = EDGE_CURVE ( 'NONE', #28929, #16735, #15156, .T. ) ;
#5601 = CARTESIAN_POINT ( 'NONE',  ( 34.31936231504242585, -12.17391896401218609, -19.91370162440023250 ) ) ;
#5602 = CARTESIAN_POINT ( 'NONE',  ( 9.949118446627077006, 16.25742953053141804, -16.49103975576934644 ) ) ;
#5603 = EDGE_CURVE ( 'NONE', #9294, #12464, #6322, .T. ) ;
#5604 =( REPRESENTATION_RELATIONSHIP ('NONE','NONE', #5250, #23798 ) REPRESENTATION_RELATIONSHIP_WITH_TRANSFORMATION ( #27210 )SHAPE_REPRESENTATION_RELATIONSHIP( ) );
#5605 = CARTESIAN_POINT ( 'NONE',  ( 172.7287565553229456, -4.999999999999971578, -36.50000000000000711 ) ) ;
#5606 = CARTESIAN_POINT ( 'NONE',  ( 3.318518101603024295, 7.321656987762882984, -4.999999999999998224 ) ) ;
#5607 = CARTESIAN_POINT ( 'NONE',  ( 12.02710433905669341, 9.320377015888107408, -16.69172260460959478 ) ) ;
#5608 = CARTESIAN_POINT ( 'NONE',  ( 139.5152310637605808, -4.999999999999980460, -30.37205893520530964 ) ) ;
#5609 = PLANE ( 'NONE',  #19830 ) ;
#5610 = ORIENTED_EDGE ( 'NONE', *, *, #23733, .F. ) ;
#5611 = LINE ( 'NONE', #17053, #9020 ) ;
#5612 = LINE ( 'NONE', #17498, #11729 ) ;
#5613 = CARTESIAN_POINT ( 'NONE',  ( 172.0152310637605240, -9.999999999999994671, -32.93883019725009120 ) ) ;
#5614 = ORIENTED_EDGE ( 'NONE', *, *, #6819, .F. ) ;
#5615 = EDGE_LOOP ( 'NONE', ( #18841, #13481, #20447, #14888 ) ) ;
#5616 = VERTEX_POINT ( 'NONE', #20341 ) ;
#5617 = CARTESIAN_POINT ( 'NONE',  ( 11.19157713609530269, 9.239454617397717229, -17.25496879848155629 ) ) ;
#5618 = VERTEX_POINT ( 'NONE', #22506 ) ;
#5619 = CARTESIAN_POINT ( 'NONE',  ( 28.46611200899306127, -11.40119892829609327, -11.67154496650716666 ) ) ;
#5620 = CARTESIAN_POINT ( 'NONE',  ( 19.60850488237918654, -1.635242255716521820, -15.65509664672261003 ) ) ;
#5621 = DIRECTION ( 'NONE',  ( 1.000000000000000000, 2.698458740408365879E-16, -1.110223024625156540E-16 ) ) ;
#5622 = CARTESIAN_POINT ( 'NONE',  ( 147.0152310637605808, -4.999999999999977796, -1.632196944975745421E-14 ) ) ;
#5623 = VECTOR ( 'NONE', #7029, 1000.000000000000000 ) ;
#5624 = DIRECTION ( 'NONE',  ( 1.000000000000000000, 2.698458740408367851E-16, 0.000000000000000000 ) ) ;
#5625 = VERTEX_POINT ( 'NONE', #29881 ) ;
#5626 = LINE ( 'NONE', #17218, #18154 ) ;
#5627 = ORIENTED_EDGE ( 'NONE', *, *, #131, .F. ) ;
#5628 = CARTESIAN_POINT ( 'NONE',  ( 20.00000000000017053, 25.64101615137744616, 12.00000000000000178 ) ) ;
#5629 = DIRECTION ( 'NONE',  ( -0.9510565162951536422, 0.000000000000000000, -0.3090169943749472292 ) ) ;
#5630 = ORIENTED_EDGE ( 'NONE', *, *, #25616, .T. ) ;
#5631 = CARTESIAN_POINT ( 'NONE',  ( 138.6922820468854525, -10.00000000000000533, -15.07341522555727309 ) ) ;
#5632 = DIRECTION ( 'NONE',  ( -0.5877852522924731371, -1.586114251531760728E-16, -0.8090169943749474513 ) ) ;
#5633 = CARTESIAN_POINT ( 'NONE',  ( 13.13063628947021755, 8.573956625762026107, -15.90631066800904669 ) ) ;
#5634 = EDGE_CURVE ( 'NONE', #6899, #13842, #10312, .T. ) ;
#5635 = EDGE_CURVE ( 'NONE', #29774, #16222, #22650, .T. ) ;
#5636 = ORIENTED_EDGE ( 'NONE', *, *, #11075, .T. ) ;
#5637 = CARTESIAN_POINT ( 'NONE',  ( 33.29128644620831778, -11.81988703332123691, -18.18190324972602667 ) ) ;
#5638 = ORIENTED_EDGE ( 'NONE', *, *, #21711, .F. ) ;
#5639 = CARTESIAN_POINT ( 'NONE',  ( 9.084523633786250940, 16.30981489620654301, -17.07623073379102507 ) ) ;
#5640 = ADVANCED_FACE ( 'NONE', ( #13030 ), #8446, .T. ) ;
#5641 = VECTOR ( 'NONE', #27305, 1000.000000000000000 ) ;
#5642 = ADVANCED_FACE ( 'NONE', ( #15304 ), #18203, .T. ) ;
#5643 = CARTESIAN_POINT ( 'NONE',  ( 24.36497833745277930, -6.082191617938494055, -18.74521747929614435 ) ) ;
#5644 = CARTESIAN_POINT ( 'NONE',  ( 12.83250652484248633, 9.539529735957493983, -16.14092858578357337 ) ) ;
#5645 = FACE_BOUND ( 'NONE', #6825, .T. ) ;
#5646 = ORIENTED_EDGE ( 'NONE', *, *, #30084, .T. ) ;
#5647 = ORIENTED_EDGE ( 'NONE', *, *, #26563, .F. ) ;
#5648 = DIRECTION ( 'NONE',  ( -0.5877852522924731371, -1.586114251531760728E-16, -0.8090169943749474513 ) ) ;
#5649 = CARTESIAN_POINT ( 'NONE',  ( 11.82447321682112751, 8.672047275158794477, -15.63808403058127006 ) ) ;
#5650 = CARTESIAN_POINT ( 'NONE',  ( 13.00000000000000178, -2.870178842070716726E-15, -23.00000000000000000 ) ) ;
#5651 = ORIENTED_EDGE ( 'NONE', *, *, #12787, .F. ) ;
#5652 = FACE_OUTER_BOUND ( 'NONE', #9794, .T. ) ;
#5653 = ORIENTED_EDGE ( 'NONE', *, *, #13100, .F. ) ;
#5654 = CARTESIAN_POINT ( 'NONE',  ( 12.02835731808789355, 9.314632867394664117, -16.69120428796748357 ) ) ;
#5655 = VECTOR ( 'NONE', #14438, 1000.000000000000000 ) ;
#5656 = ORIENTED_EDGE ( 'NONE', *, *, #21765, .F. ) ;
#5657 = CARTESIAN_POINT ( 'NONE',  ( 14.45328171724474231, 7.053988074037379263, -14.59236433646538522 ) ) ;
#5658 = CARTESIAN_POINT ( 'NONE',  ( 13.93547621865856634, 6.828337171336619882, -15.16703734247451507 ) ) ;
#5659 = VECTOR ( 'NONE', #22086, 1000.000000000000000 ) ;
#5660 = DIRECTION ( 'NONE',  ( 0.5877852522924731371, 1.586114251531760728E-16, 0.8090169943749474513 ) ) ;
#5661 = ORIENTED_EDGE ( 'NONE', *, *, #8903, .T. ) ;
#5662 = CARTESIAN_POINT ( 'NONE',  ( 36.54859390954303677, -22.18451583373416014, -15.55638201429745848 ) ) ;
#5663 = ITEM_DEFINED_TRANSFORMATION ( 'NONE', 'NONE', #17534,  #13190 ) ;
#5664 = CARTESIAN_POINT ( 'NONE',  ( 19.31105547890425100, 3.022890346832332042, -18.89353813576326857 ) ) ;
#5665 = CARTESIAN_POINT ( 'NONE',  ( 14.29829396236512729, 6.476847147513518088, -18.28004444394726491 ) ) ;
#5666 = CIRCLE ( 'NONE', #9540, 8.000000000000000000 ) ;
#5667 = DIRECTION ( 'NONE',  ( 1.000000000000000000, 2.698458740408365879E-16, -1.110223024625156540E-16 ) ) ;
#5668 = FACE_BOUND ( 'NONE', #14783, .T. ) ;
#5669 = DIRECTION ( 'NONE',  ( 1.000000000000000000, 4.440892098500622217E-16, 0.000000000000000000 ) ) ;
#5670 = EDGE_CURVE ( 'NONE', #4933, #28698, #19894, .T. ) ;
#5671 = CARTESIAN_POINT ( 'NONE',  ( 159.5152310637605524, -9.999999999999998224, -28.60870317832789667 ) ) ;
#5672 = CARTESIAN_POINT ( 'NONE',  ( 13.52175692454036415, 9.804829592035652297, -15.59458061810998331 ) ) ;
#5673 = ADVANCED_FACE ( 'NONE', ( #10744 ), #13471, .T. ) ;
#5674 = LINE ( 'NONE', #8094, #2230 ) ;
#5675 = VECTOR ( 'NONE', #24995, 1000.000000000000000 ) ;
#5676 = EDGE_CURVE ( 'NONE', #14294, #15364, #22801, .T. ) ;
#5677 = CARTESIAN_POINT ( 'NONE',  ( 12.27693553943969818, 9.494520259125854622, -15.31067919898749352 ) ) ;
#5678 = CARTESIAN_POINT ( 'NONE',  ( 169.5152310637604103, -1.999999999999971356, -4.391296821672111328 ) ) ;
#5679 = ORIENTED_EDGE ( 'NONE', *, *, #26474, .F. ) ;
#5680 = CARTESIAN_POINT ( 'NONE',  ( 31.81434894052502571, -10.04473835610349397, -15.03854332269495764 ) ) ;
#5681 = VERTEX_POINT ( 'NONE', #24491 ) ;
#5682 = AXIS2_PLACEMENT_3D ( 'NONE', #24761, #3849, #27534 ) ;
#5683 = CARTESIAN_POINT ( 'NONE',  ( 11.65548303173490652, 8.849831895876286936, -15.75351705932409985 ) ) ;
#5684 = EDGE_LOOP ( 'NONE', ( #15353, #5529, #7970 ) ) ;
#5685 = CARTESIAN_POINT ( 'NONE',  ( 11.89457502915311160, 7.563359933683480918, -15.58843798323820096 ) ) ;
#5686 = CARTESIAN_POINT ( 'NONE',  ( 163.6922820468852819, -4.999999999999973355, 2.247092850131519715 ) ) ;
#5687 = DIRECTION ( 'NONE',  ( 1.000000000000000000, 2.698458740408365879E-16, -1.110223024625156540E-16 ) ) ;
#5688 = CARTESIAN_POINT ( 'NONE',  ( 169.5152310637604955, -9.999999999999996447, -19.94844914048349693 ) ) ;
#5689 = VERTEX_POINT ( 'NONE', #17751 ) ;
#5690 = CARTESIAN_POINT ( 'NONE',  ( 146.1922820468854525, -4.999999999999977796, -28.06379628232387446 ) ) ;
#5691 = EDGE_LOOP ( 'NONE', ( #25456, #20125, #14195, #24805, #29229, #4475, #29846, #20602, #11377, #17139, #25592, #13367, #27041, #366, #14238, #12342, #22997, #1733, #21799, #20684, #7129, #10058, #8788, #7596, #22296, #19648, #9789, #18188, #22749, #5704, #955, #1348, #16477, #18743, #3400, #16144, #30212, #3947, #13630, #17564, #14278, #2418, #24597, #17325 ) ) ;
#5692 = CARTESIAN_POINT ( 'NONE',  ( 12.83250652484248633, 9.539529735957493983, -16.14092858578357337 ) ) ;
#5693 = CARTESIAN_POINT ( 'NONE',  ( 33.85795792134603488, -11.10969635406632072, -17.56389463281766439 ) ) ;
#5694 = CARTESIAN_POINT ( 'NONE',  ( 15.78240017141095741, 4.038647184180326200, -18.77507866864583619 ) ) ;
#5695 = ORIENTED_EDGE ( 'NONE', *, *, #14261, .T. ) ;
#5696 = DIRECTION ( 'NONE',  ( 0.5877852522924731371, 0.000000000000000000, 0.8090169943749474513 ) ) ;
#5697 = CARTESIAN_POINT ( 'NONE',  ( 20.01918758985507196, 7.682949113293006782, -15.97060347488303123 ) ) ;
#5698 = CARTESIAN_POINT ( 'NONE',  ( 131.1922820468854241, -10.00000000000000888, -19.40354224447947473 ) ) ;
#5699 = FACE_OUTER_BOUND ( 'NONE', #6897, .T. ) ;
#5700 = CARTESIAN_POINT ( 'NONE',  ( 24.59824444495380646, -5.013944910511990649, -19.70109713935865514 ) ) ;
#5701 = CARTESIAN_POINT ( 'NONE',  ( 18.38621934312857320, -2.136830130942094730, -15.12482301043797683 ) ) ;
#5702 = VECTOR ( 'NONE', #3707, 1000.000000000000000 ) ;
#5703 = ORIENTED_EDGE ( 'NONE', *, *, #19196, .F. ) ;
#5704 = ORIENTED_EDGE ( 'NONE', *, *, #1661, .F. ) ;
#5705 = DIRECTION ( 'NONE',  ( 0.000000000000000000, 0.000000000000000000, -1.000000000000000000 ) ) ;
#5706 = VECTOR ( 'NONE', #21523, 1000.000000000000000 ) ;
#5707 = ORIENTED_EDGE ( 'NONE', *, *, #9572, .T. ) ;
#5708 = AXIS2_PLACEMENT_3D ( 'NONE', #27635, #6700, #2133 ) ;
#5709 = LINE ( 'NONE', #3420, #655 ) ;
#5710 = LINE ( 'NONE', #21582, #830 ) ;
#5711 = VECTOR ( 'NONE', #20482, 1000.000000000000000 ) ;
#5712 = DIRECTION ( 'NONE',  ( 1.000000000000000000, 4.440892098500622217E-16, 0.000000000000000000 ) ) ;
#5713 = EDGE_CURVE ( 'NONE', #15063, #11701, #3584, .T. ) ;
#5714 = EDGE_CURVE ( 'NONE', #29328, #8506, #9261, .T. ) ;
#5715 = DIRECTION ( 'NONE',  ( 0.9510565162951536422, 0.000000000000000000, -0.3090169943749475623 ) ) ;
#5716 = ADVANCED_FACE ( 'NONE', ( #29264 ), #20193, .F. ) ;
#5717 = CARTESIAN_POINT ( 'NONE',  ( 11.47293561586387867, 9.269010148984008879, -15.86088772249501666 ) ) ;
#5718 = EDGE_CURVE ( 'NONE', #22368, #4371, #4032, .T. ) ;
#5719 = CARTESIAN_POINT ( 'NONE',  ( 28.47173825316771101, -6.366402965996883268, -15.18523185298700007 ) ) ;
#5720 = CARTESIAN_POINT ( 'NONE',  ( 28.73289915209718615, -4.972737245092835323, -15.12275039236161689 ) ) ;
#5721 = DIRECTION ( 'NONE',  ( -2.698458740408365879E-16, 1.000000000000000000, 0.000000000000000000 ) ) ;
#5722 = DIRECTION ( 'NONE',  ( 0.000000000000000000, 0.000000000000000000, 1.000000000000000000 ) ) ;
#5723 = DIRECTION ( 'NONE',  ( -2.698458740408365879E-16, 1.000000000000000000, 0.000000000000000000 ) ) ;
#5724 = DIRECTION ( 'NONE',  ( -2.698458740408365879E-16, 1.000000000000000000, 0.000000000000000000 ) ) ;
#5725 = VECTOR ( 'NONE', #14670, 1000.000000000000000 ) ;
#5726 = DIRECTION ( 'NONE',  ( 0.9510565162951535312, 2.566386769018988816E-16, -0.3090169943749475623 ) ) ;
#5727 = CARTESIAN_POINT ( 'NONE',  ( 19.12501085131992085, -2.578449613843157184, -15.80510918775627438 ) ) ;
#5728 = VERTEX_POINT ( 'NONE', #23397 ) ;
#5729 = CARTESIAN_POINT ( 'NONE',  ( 172.0152310637604103, -1.999999999999970912, 1.702185954127501066 ) ) ;
#5730 = CARTESIAN_POINT ( 'NONE',  ( 12.27669453124947552, 9.495625565821059766, -15.31077886340536942 ) ) ;
#5731 = AXIS2_PLACEMENT_3D ( 'NONE', #4787, #12249, #5237 ) ;
#5732 = CARTESIAN_POINT ( 'NONE',  ( 175.7287565553229456, -9.999999999999971578, 3.500000000000003109 ) ) ;
#5733 = LINE ( 'NONE', #29115, #25409 ) ;
#5734 = CARTESIAN_POINT ( 'NONE',  ( 23.76365953361780470, 2.837943588559999508, -16.54419024451982168 ) ) ;
#5735 = CARTESIAN_POINT ( 'NONE',  ( 20.00000000000017053, 34.64101615137744972, 10.00000000000000178 ) ) ;
#5736 = CARTESIAN_POINT ( 'NONE',  ( 16.03284225665507279, 2.387151393075086059, -14.54955438622115338 ) ) ;
#5737 = VERTEX_POINT ( 'NONE', #6616 ) ;
#5738 = LINE ( 'NONE', #28975, #9575 ) ;
#5739 = CARTESIAN_POINT ( 'NONE',  ( 31.24625831705917278, -7.622123577322120980, -17.00257116200763008 ) ) ;
#5740 = CARTESIAN_POINT ( 'NONE',  ( 21.92900763033978251, 0.1816185532145172810, -13.27135403042708717 ) ) ;
#5741 = ORIENTED_EDGE ( 'NONE', *, *, #7539, .F. ) ;
#5742 = EDGE_CURVE ( 'NONE', #26944, #29723, #6925, .T. ) ;
#5743 = CARTESIAN_POINT ( 'NONE',  ( 29.30346499805017757, -7.722527705200430859, -14.56292402596598556 ) ) ;
#5744 = VECTOR ( 'NONE', #26266, 1000.000000000000000 ) ;
#5745 = CARTESIAN_POINT ( 'NONE',  ( 133.7287565553229456, -4.000000000000003553, 8.500000000000007105 ) ) ;
#5746 = ORIENTED_EDGE ( 'NONE', *, *, #20653, .F. ) ;
#5747 = ORIENTED_EDGE ( 'NONE', *, *, #13351, .T. ) ;
#5748 = FILL_AREA_STYLE_COLOUR ( '', #26845 ) ;
#5749 = VECTOR ( 'NONE', #3228, 999.9999999999998863 ) ;
#5750 = CARTESIAN_POINT ( 'NONE',  ( 3.839988787535719261, -5.000000000000016875, 11.81827027433623734 ) ) ;
#5751 = DIRECTION ( 'NONE',  ( 0.5877852522924731371, 1.586114251531760728E-16, -0.8090169943749474513 ) ) ;
#5752 = ADVANCED_FACE ( 'NONE', ( #14067 ), #25532, .T. ) ;
#5753 = EDGE_CURVE ( 'NONE', #22950, #14986, #22937, .T. ) ;
#5754 = CARTESIAN_POINT ( 'NONE',  ( 14.59671049609067950, 6.266606045730605423, -20.00302036566705155 ) ) ;
#5755 = CARTESIAN_POINT ( 'NONE',  ( 35.77509030908504428, -18.70957389315904962, -20.35615221346758474 ) ) ;
#5756 = CARTESIAN_POINT ( 'NONE',  ( 11.43229926783177497, 9.455373222906182207, -15.87769231223556332 ) ) ;
#5757 = DIRECTION ( 'NONE',  ( -1.000000000000000000, 1.840388255087189623E-16, 0.000000000000000000 ) ) ;
#5758 = CARTESIAN_POINT ( 'NONE',  ( 144.5152310637605808, -1.999999999999977573, -11.28819510263909542 ) ) ;
#5759 = CARTESIAN_POINT ( 'NONE',  ( 9.661958148507006072, 16.25448227554711167, -17.91102859374088752 ) ) ;
#5760 = LINE ( 'NONE', #8030, #12677 ) ;
#5761 = CARTESIAN_POINT ( 'NONE',  ( 172.0152310637603819, -9.999999999999996447, -0.06116980274991495881 ) ) ;
#5762 = ORIENTED_EDGE ( 'NONE', *, *, #19383, .F. ) ;
#5763 = LINE ( 'NONE', #1190, #25645 ) ;
#5764 = CARTESIAN_POINT ( 'NONE',  ( 5.000000000000000888, 0.000000000000000000, 0.000000000000000000 ) ) ;
#5765 = VECTOR ( 'NONE', #15786, 1000.000000000000000 ) ;
#5766 = FACE_OUTER_BOUND ( 'NONE', #4493, .T. ) ;
#5767 = ORIENTED_EDGE ( 'NONE', *, *, #25832, .T. ) ;
#5768 = ORIENTED_EDGE ( 'NONE', *, *, #25320, .F. ) ;
#5769 = EDGE_LOOP ( 'NONE', ( #24998, #8551, #27947, #23201 ) ) ;
#5770 = CARTESIAN_POINT ( 'NONE',  ( 13.36280753930113363, 7.618652675320872980, -15.72125653641924892 ) ) ;
#5771 = CONICAL_SURFACE ( 'NONE', #1888, 4.000000000000003553, 1.047197551196597853 ) ;
#5772 = CARTESIAN_POINT ( 'NONE',  ( 30.27995308908331751, -6.828448725465094959, -15.78586218199752622 ) ) ;
#5773 = CARTESIAN_POINT ( 'NONE',  ( 29.02390443993225588, -5.138988301204332920, -16.36505798003706857 ) ) ;
#5774 = PLANE ( 'NONE',  #4798 ) ;
#5775 = LINE ( 'NONE', #26542, #27276 ) ;
#5776 = DIRECTION ( 'NONE',  ( 0.000000000000000000, 0.000000000000000000, 1.000000000000000000 ) ) ;
#5777 = EDGE_CURVE ( 'NONE', #25730, #17843, #21102, .T. ) ;
#5778 = ORIENTED_EDGE ( 'NONE', *, *, #16959, .T. ) ;
#5779 = LINE ( 'NONE', #19348, #14724 ) ;
#5780 = DIRECTION ( 'NONE',  ( 0.3090169943749472292, 8.338696094057992503E-17, -0.9510565162951536422 ) ) ;
#5781 = ORIENTED_EDGE ( 'NONE', *, *, #28760, .T. ) ;
#5782 = CARTESIAN_POINT ( 'NONE',  ( 162.0152310637604671, -9.999999999999998224, -6.958068083716895558 ) ) ;
#5783 = CARTESIAN_POINT ( 'NONE',  ( 0.000000000000000000, 0.000000000000000000, 18.00000000000000000 ) ) ;
#5784 = EDGE_CURVE ( 'NONE', #18885, #26241, #15909, .T. ) ;
#5785 = CARTESIAN_POINT ( 'NONE',  ( 13.13233772467555660, 8.574708520419219937, -15.90495459411799395 ) ) ;
#5786 = CARTESIAN_POINT ( 'NONE',  ( 35.54859390953724585, -22.18451583373416014, -16.94733705004010460 ) ) ;
#5787 = VECTOR ( 'NONE', #28803, 1000.000000000000000 ) ;
#5788 = EDGE_LOOP ( 'NONE', ( #5194, #14429, #11267, #8827 ) ) ;
#5789 = CARTESIAN_POINT ( 'NONE',  ( 9.120682955242472190, 16.14398363876680520, -17.05135327743868245 ) ) ;
#5790 = CARTESIAN_POINT ( 'NONE',  ( 25.67262840375075328, -3.322766148301121714, -14.04542551033457798 ) ) ;
#5791 = CARTESIAN_POINT ( 'NONE',  ( 13.41286507499157388, 9.756708335562493062, -15.68136934427840856 ) ) ;
#5792 = FACE_BOUND ( 'NONE', #24163, .T. ) ;
#5793 = EDGE_LOOP ( 'NONE', ( #21940, #27566, #3078, #19528 ) ) ;
#5794 = CIRCLE ( 'NONE', #22374, 8.000000000000005329 ) ;
#5795 = ORIENTED_EDGE ( 'NONE', *, *, #18303, .T. ) ;
#5796 = CARTESIAN_POINT ( 'NONE',  ( -2.928571428571432378, -9.419004090963157619E-16, 9.480888224575629408 ) ) ;
#5797 = CARTESIAN_POINT ( 'NONE',  ( 12.49860086554322436, 8.570087612320898884, -15.13128986298120537 ) ) ;
#5798 = CARTESIAN_POINT ( 'NONE',  ( 0.000000000000000000, 0.000000000000000000, -23.00000000000000000 ) ) ;
#5799 = EDGE_LOOP ( 'NONE', ( #13620, #22872, #14489, #22037 ) ) ;
#5800 = LINE ( 'NONE', #24270, #6205 ) ;
#5801 = VERTEX_POINT ( 'NONE', #20943 ) ;
#5802 = CARTESIAN_POINT ( 'NONE',  ( 12.90142504057275197, 8.513187104919181181, -16.08590544042818493 ) ) ;
#5803 = EDGE_LOOP ( 'NONE', ( #17200, #22567, #7220, #29454, #6630 ) ) ;
#5804 = CARTESIAN_POINT ( 'NONE',  ( 17.82530828565625214, 4.245919164363588294, -12.95079069805369443 ) ) ;
#5805 = CARTESIAN_POINT ( 'NONE',  ( 20.92570677221209507, 1.074447142478794470, -13.03661572703551919 ) ) ;
#5806 = VERTEX_POINT ( 'NONE', #28168 ) ;
#5807 = DIRECTION ( 'NONE',  ( -1.110223024625156540E-16, 0.000000000000000000, -1.000000000000000000 ) ) ;
#5808 = ORIENTED_EDGE ( 'NONE', *, *, #14056, .T. ) ;
#5809 = CARTESIAN_POINT ( 'NONE',  ( 36.54779501103016770, -22.18092680593016652, -18.48200341583098449 ) ) ;
#5810 = APPLICATION_PROTOCOL_DEFINITION ( 'draft international standard', 'automotive_design', 1998, #12001 ) ;
#5811 = EDGE_CURVE ( 'NONE', #13972, #18723, #27712, .T. ) ;
#5812 = EDGE_CURVE ( 'NONE', #25860, #102, #9487, .T. ) ;
#5813 = EDGE_CURVE ( 'NONE', #25448, #20344, #13771, .T. ) ;
#5814 = VECTOR ( 'NONE', #19882, 1000.000000000000000 ) ;
#5815 = EDGE_CURVE ( 'NONE', #21366, #8557, #11474, .T. ) ;
#5816 = CARTESIAN_POINT ( 'NONE',  ( 17.66155849027303049, 7.702290371990539342, -14.74052880078125760 ) ) ;
#5817 = CARTESIAN_POINT ( 'NONE',  ( 149.5152310637605524, -4.999999999999976907, -1.659952520591374019E-14 ) ) ;
#5818 = DIRECTION ( 'NONE',  ( -0.9510565162951536422, 0.000000000000000000, -0.3090169943749472292 ) ) ;
#5819 = CARTESIAN_POINT ( 'NONE',  ( 157.2287565553230024, -10.00000000000000000, -29.49038105676660493 ) ) ;
#5820 = CARTESIAN_POINT ( 'NONE',  ( 33.43446274600908907, -12.68684440242773448, -19.71889742777951327 ) ) ;
#5821 = CARTESIAN_POINT ( 'NONE',  ( 8.452900878024367515, -5.000000000000015099, 26.01535387366982732 ) ) ;
#5822 = DIRECTION ( 'NONE',  ( -2.698458740408365879E-16, 1.000000000000000000, 0.000000000000000000 ) ) ;
#5823 = CARTESIAN_POINT ( 'NONE',  ( 12.27669453124947552, 9.495625565821059766, -15.31077886340536942 ) ) ;
#5824 = DIRECTION ( 'NONE',  ( -0.000000000000000000, -0.000000000000000000, -1.000000000000000000 ) ) ;
#5825 = ORIENTED_EDGE ( 'NONE', *, *, #26743, .T. ) ;
#5826 = AXIS2_PLACEMENT_3D ( 'NONE', #3984, #9135, #1865 ) ;
#5827 = LINE ( 'NONE', #17119, #4245 ) ;
#5828 = EDGE_LOOP ( 'NONE', ( #6316, #14751, #15447 ) ) ;
#5829 = CARTESIAN_POINT ( 'NONE',  ( 12.29195110325218288, 8.516770644378290456, -15.29309475950548958 ) ) ;
#5830 = ORIENTED_EDGE ( 'NONE', *, *, #11572, .T. ) ;
#5831 = CARTESIAN_POINT ( 'NONE',  ( 12.65299103417153681, 7.585129394224154886, -15.00786874580416530 ) ) ;
#5832 = CARTESIAN_POINT ( 'NONE',  ( -15.99999999999998224, -1.561251128379126385E-14, -5.000000000000000888 ) ) ;
#5833 = PLANE ( 'NONE',  #17397 ) ;
#5834 = ORIENTED_EDGE ( 'NONE', *, *, #8754, .F. ) ;
#5835 = AXIS2_PLACEMENT_3D ( 'NONE', #28711, #5477, #12635 ) ;
#5836 = ORIENTED_EDGE ( 'NONE', *, *, #520, .F. ) ;
#5837 = DIRECTION ( 'NONE',  ( -0.5877852522924731371, 0.000000000000000000, 0.8090169943749474513 ) ) ;
#5838 = ORIENTED_EDGE ( 'NONE', *, *, #8004, .F. ) ;
#5839 = CARTESIAN_POINT ( 'NONE',  ( 12.75119036009696316, 9.912382880115339745, -16.17456125963731850 ) ) ;
#5840 = VERTEX_POINT ( 'NONE', #4624 ) ;
#5841 = CARTESIAN_POINT ( 'NONE',  ( 36.19723272591463115, -19.60603615691276858, -19.44143419077989421 ) ) ;
#5842 = CARTESIAN_POINT ( 'NONE',  ( 18.80472905218952917, 2.352968372735388503, -20.19605574946481497 ) ) ;
#5843 = ORIENTED_EDGE ( 'NONE', *, *, #6742, .F. ) ;
#5844 = FACE_OUTER_BOUND ( 'NONE', #1301, .T. ) ;
#5845 = CARTESIAN_POINT ( 'NONE',  ( 17.83091951040035283, 10.74857467630938501, -15.40187535130914753 ) ) ;
#5846 = LINE ( 'NONE', #10714, #1398 ) ;
#5847 = CARTESIAN_POINT ( 'NONE',  ( 34.54859390953723874, -22.18451583373416014, -36.50100000000000477 ) ) ;
#5848 = EDGE_CURVE ( 'NONE', #27629, #12251, #2970, .T. ) ;
#5849 = CARTESIAN_POINT ( 'NONE',  ( 24.14852421541024441, 0.2028892341458684023, -15.23052705399570428 ) ) ;
#5850 = EDGE_CURVE ( 'NONE', #4487, #18112, #25617, .T. ) ;
#5851 = CARTESIAN_POINT ( 'NONE',  ( 21.72387110042699376, 1.401658020055618792, -20.45241765577301152 ) ) ;
#5852 = EDGE_CURVE ( 'NONE', #17919, #2926, #4325, .T. ) ;
#5853 = COLOUR_RGB ( '', 0.31764706, 0.68627451, 0.89019608) ;
#5854 = VERTEX_POINT ( 'NONE', #2359 ) ;
#5855 = LINE ( 'NONE', #5557, #21047 ) ;
#5856 = AXIS2_PLACEMENT_3D ( 'NONE', #14008, #23492, #18911 ) ;
#5858 = LINE ( 'NONE', #11018, #7276 ) ;
#5857 = AXIS2_PLACEMENT_3D ( 'NONE', #21397, #20937, #25527 ) ;
#5859 = VECTOR ( 'NONE', #6537, 1000.000000000000000 ) ;
#5860 = CARTESIAN_POINT ( 'NONE',  ( 133.7287565553229456, -9.999999999999980460, 8.500000000000003553 ) ) ;
#5861 = AXIS2_PLACEMENT_3D ( 'NONE', #6196, #17920, #22828 ) ;
#5862 = LINE ( 'NONE', #15144, #16421 ) ;
#5863 = DIRECTION ( 'NONE',  ( -0.9510565162951536422, 0.000000000000000000, -0.3090169943749472292 ) ) ;
#5864 = LINE ( 'NONE', #4019, #16301 ) ;
#5865 = ORIENTED_EDGE ( 'NONE', *, *, #26182, .F. ) ;
#5866 = CARTESIAN_POINT ( 'NONE',  ( 10.95411528722473626, 11.64838591225006859, -16.07543820933196699 ) ) ;
#5867 = CARTESIAN_POINT ( 'NONE',  ( 15.70491959545049987, 3.570626008024105680, -15.63470537622339229 ) ) ;
#5869 = VECTOR ( 'NONE', #14448, 1000.000000000000000 ) ;
#5868 = CARTESIAN_POINT ( 'NONE',  ( 24.51672896724849338, -10.45039314358892035, -14.45231470433035170 ) ) ;
#5870 = EDGE_LOOP ( 'NONE', ( #21744, #17723, #3552, #16571 ) ) ;
#5871 = PLANE ( 'NONE',  #30094 ) ;
#5872 = DIRECTION ( 'NONE',  ( 0.5877852522924731371, 0.000000000000000000, 0.8090169943749474513 ) ) ;
#5873 = CARTESIAN_POINT ( 'NONE',  ( 133.6922820468854241, -10.00000000000000711, -15.07341522555727309 ) ) ;
#5874 = AXIS2_PLACEMENT_3D ( 'NONE', #24794, #10882, #1297 ) ;
#5875 = DIRECTION ( 'NONE',  ( 0.000000000000000000, 0.000000000000000000, 1.000000000000000000 ) ) ;
#5876 = DIRECTION ( 'NONE',  ( 0.9510565162951536422, 0.000000000000000000, -0.3090169943749475623 ) ) ;
#5877 = FACE_OUTER_BOUND ( 'NONE', #11328, .T. ) ;
#5878 = CARTESIAN_POINT ( 'NONE',  ( 18.04049687913209610, 0.8262538513465327306, -14.27019888128743297 ) ) ;
#5879 = ORIENTED_EDGE ( 'NONE', *, *, #6746, .T. ) ;
#5880 = PLANE ( 'NONE',  #4674 ) ;
#5881 = CARTESIAN_POINT ( 'NONE',  ( 10.80186837770346919, 16.25936630249904269, -15.92067135797631217 ) ) ;
#5882 = EDGE_CURVE ( 'NONE', #23347, #888, #18667, .T. ) ;
#5883 =( GEOMETRIC_REPRESENTATION_CONTEXT ( 3 ) GLOBAL_UNCERTAINTY_ASSIGNED_CONTEXT ( ( #25378 ) ) GLOBAL_UNIT_ASSIGNED_CONTEXT ( ( #17320, #1021, #22364 ) ) REPRESENTATION_CONTEXT ( 'NONE', 'WORKASPACE' ) );
#5884 = CARTESIAN_POINT ( 'NONE',  ( 139.7287565553230309, -4.999999999999979572, -25.16025403784439973 ) ) ;
#5885 = DIRECTION ( 'NONE',  ( -2.698458740408365879E-16, 1.000000000000000000, 0.000000000000000000 ) ) ;
#5886 = EDGE_LOOP ( 'NONE', ( #16599, #6085, #10247, #2396 ) ) ;
#5887 = CARTESIAN_POINT ( 'NONE',  ( 20.14386580841007657, 1.771853782379294140, -13.30505882909219295 ) ) ;
#5888 = DIRECTION ( 'NONE',  ( 0.5877852522924731371, 1.586114251531760728E-16, -0.8090169943749474513 ) ) ;
#5889 = CARTESIAN_POINT ( 'NONE',  ( 20.33560388840259137, 1.841519175196629998, -20.14887626749220217 ) ) ;
#5890 = ORIENTED_EDGE ( 'NONE', *, *, #17332, .T. ) ;
#5891 = DIRECTION ( 'NONE',  ( -0.5877852522924731371, -1.586114251531760728E-16, -0.8090169943749474513 ) ) ;
#5892 = CARTESIAN_POINT ( 'NONE',  ( 23.37849240255853189, -5.075553540114302820, -18.86401745356084447 ) ) ;
#5893 = CARTESIAN_POINT ( 'NONE',  ( 22.85243615162648112, -7.655412890396200432, -19.01377894019457315 ) ) ;
#5894 = EDGE_CURVE ( 'NONE', #7473, #26271, #13623, .T. ) ;
#5895 = EDGE_CURVE ( 'NONE', #21764, #29919, #25687, .T. ) ;
#5896 = EDGE_CURVE ( 'NONE', #18587, #13963, #9646, .T. ) ;
#5897 = EDGE_CURVE ( 'NONE', #9309, #16652, #2514, .T. ) ;
#5898 = LINE ( 'NONE', #1170, #12713 ) ;
#5899 = CIRCLE ( 'NONE', #15128, 2.041999999999999815 ) ;
#5900 = CARTESIAN_POINT ( 'NONE',  ( 2.500000000000000444, -1.178949249685215417, 2.042000000000002036 ) ) ;
#5901 = LINE ( 'NONE', #29130, #12656 ) ;
#5902 = FACE_OUTER_BOUND ( 'NONE', #159, .T. ) ;
#5903 = DIRECTION ( 'NONE',  ( 1.000000000000000000, 0.000000000000000000, 0.000000000000000000 ) ) ;
#5904 = CARTESIAN_POINT ( 'NONE',  ( 167.2287565553229456, -9.999999999999998224, -20.83012701892220520 ) ) ;
#5905 = CARTESIAN_POINT ( 'NONE',  ( 25.86320101420157158, -8.291784280105535032, -12.84902276017926859 ) ) ;
#5906 = DIRECTION ( 'NONE',  ( -2.698458740408365879E-16, 1.000000000000000000, 0.000000000000000000 ) ) ;
#5907 = CARTESIAN_POINT ( 'NONE',  ( 34.18187006836440389, -11.68445768601494628, -19.79758194388510972 ) ) ;
#5908 = CARTESIAN_POINT ( 'NONE',  ( 13.00000000000000178, -2.870178842070716726E-15, 18.00000000000000000 ) ) ;
#5909 = CARTESIAN_POINT ( 'NONE',  ( 9.917015787971365626, 16.40465641526357743, -16.50431533440121257 ) ) ;
#5910 = PLANE ( 'NONE',  #13225 ) ;
#5911 = CARTESIAN_POINT ( 'NONE',  ( -20.00000000000017053, 34.64101615137744972, 9.999999999999998224 ) ) ;
#5912 = CARTESIAN_POINT ( 'NONE',  ( 9.661883061612440926, 16.25482663361732705, -17.95086732675816776 ) ) ;
#5913 = DIRECTION ( 'NONE',  ( 0.5877852522924731371, 1.586114251531760728E-16, -0.8090169943749474513 ) ) ;
#5914 = CARTESIAN_POINT ( 'NONE',  ( 138.6922820468854241, -1.999999999999980016, -0.6060766987539614181 ) ) ;
#5915 = VECTOR ( 'NONE', #9559, 1000.000000000000000 ) ;
#5916 = ORIENTED_EDGE ( 'NONE', *, *, #2413, .T. ) ;
#5917 = AXIS2_PLACEMENT_3D ( 'NONE', #12284, #17462, #17313 ) ;
#5918 = LINE ( 'NONE', #27153, #5659 ) ;
#5919 = DIRECTION ( 'NONE',  ( 0.000000000000000000, -1.224646799147353454E-16, 1.000000000000000000 ) ) ;
#5920 = DIRECTION ( 'NONE',  ( -0.5877852522924731371, 0.000000000000000000, 0.8090169943749474513 ) ) ;
#5921 = ORIENTED_EDGE ( 'NONE', *, *, #9051, .F. ) ;
#5922 = ORIENTED_EDGE ( 'NONE', *, *, #25828, .F. ) ;
#5923 = CARTESIAN_POINT ( 'NONE',  ( 8.944584683310379702, 16.95159276115599667, -21.33333333332589632 ) ) ;
#5924 = CARTESIAN_POINT ( 'NONE',  ( 13.70585326225313771, 5.953887885347688425, -14.73188983601744617 ) ) ;
#5925 = ADVANCED_FACE ( 'NONE', ( #21249 ), #27563, .T. ) ;
#5926 = CARTESIAN_POINT ( 'NONE',  ( 24.19195398915606532, -10.47609993289601427, -15.85356615136800151 ) ) ;
#5927 = LINE ( 'NONE', #15212, #2860 ) ;
#5928 = FACE_OUTER_BOUND ( 'NONE', #4329, .T. ) ;
#5929 = EDGE_CURVE ( 'NONE', #6861, #23077, #26599, .T. ) ;
#5930 = CARTESIAN_POINT ( 'NONE',  ( 142.0152310637606092, -10.00000000000000355, -32.93883019725009120 ) ) ;
#5931 = ADVANCED_FACE ( 'NONE', ( #3111 ), #23862, .F. ) ;
#5932 = ORIENTED_EDGE ( 'NONE', *, *, #17141, .F. ) ;
#5933 = CARTESIAN_POINT ( 'NONE',  ( 173.6922820468852819, -1.999999999999970024, -6.413161187712876909 ) ) ;
#5934 = LINE ( 'NONE', #24099, #25336 ) ;
#5935 = EDGE_LOOP ( 'NONE', ( #25680, #9529, #20094, #11677 ) ) ;
#5936 = DIRECTION ( 'NONE',  ( 0.3090169943749472292, 8.338696094057992503E-17, -0.9510565162951536422 ) ) ;
#5937 = CARTESIAN_POINT ( 'NONE',  ( 152.2287565553229456, -4.999999999999976907, -3.509618943233400401 ) ) ;
#5938 = CARTESIAN_POINT ( 'NONE',  ( 13.12404665403065707, 8.571044468271947991, -15.91156272984762765 ) ) ;
#5939 = CARTESIAN_POINT ( 'NONE',  ( 35.54859390953724585, -22.18451583373416014, -17.64281456791166036 ) ) ;
#5940 = ORIENTED_EDGE ( 'NONE', *, *, #16236, .F. ) ;
#5941 = CARTESIAN_POINT ( 'NONE',  ( 10.50660601767968139, 9.787963810330234438, -16.47822533839871539 ) ) ;
#5942 = VERTEX_POINT ( 'NONE', #28321 ) ;
#5943 = CARTESIAN_POINT ( 'NONE',  ( 21.16681283796276603, -5.103637247178538061, -17.00692323485822754 ) ) ;
#5944 = CARTESIAN_POINT ( 'NONE',  ( 12.89562877257107054, 9.528132359803098694, -16.09361580714184825 ) ) ;
#5945 = FACE_BOUND ( 'NONE', #13298, .T. ) ;
#5946 = ADVANCED_FACE ( 'NONE', ( #7516 ), #19557, .T. ) ;
#5947 = ORIENTED_EDGE ( 'NONE', *, *, #10800, .T. ) ;
#5948 = LINE ( 'NONE', #5796, #4795 ) ;
#5949 = VERTEX_POINT ( 'NONE', #12532 ) ;
#5950 = CARTESIAN_POINT ( 'NONE',  ( 11.46471852075427478, 9.306694396509932687, -15.86428581073749378 ) ) ;
#5952 = DIRECTION ( 'NONE',  ( 0.9510565162951536422, 2.566386769018988816E-16, 0.3090169943749472292 ) ) ;
#5951 = AXIS2_PLACEMENT_3D ( 'NONE', #29827, #8837, #4567 ) ;
#5953 = ORIENTED_EDGE ( 'NONE', *, *, #5328, .F. ) ;
#5954 = PLANE ( 'NONE',  #25201 ) ;
#5955 = ORIENTED_EDGE ( 'NONE', *, *, #17783, .F. ) ;
#5956 = CARTESIAN_POINT ( 'NONE',  ( 9.661883061612440926, 16.25482663361732705, -17.91664992932185996 ) ) ;
#5957 = EDGE_LOOP ( 'NONE', ( #3542, #4853, #18816, #22389, #19255 ) ) ;
#5958 = CARTESIAN_POINT ( 'NONE',  ( 20.05201200715256249, 8.675301412908657639, -18.33989206490851842 ) ) ;
#5959 = CARTESIAN_POINT ( 'NONE',  ( 17.82530828565625214, 4.245919164363588294, -12.95079069805369443 ) ) ;
#5960 = DIRECTION ( 'NONE',  ( -2.698458740408365879E-16, 1.000000000000000000, 0.000000000000000000 ) ) ;
#5961 = ORIENTED_EDGE ( 'NONE', *, *, #24957, .T. ) ;
#5962 = LINE ( 'NONE', #935, #3530 ) ;
#5963 = CARTESIAN_POINT ( 'NONE',  ( 16.79143122783437292, 7.330551994622505063, -14.54187356113185103 ) ) ;
#5964 = VECTOR ( 'NONE', #21578, 1000.000000000000000 ) ;
#5965 = CARTESIAN_POINT ( 'NONE',  ( 0.000000000000000000, 3.966417288046574668E-16, 4.187999999999997947 ) ) ;
#5966 = PLANE ( 'NONE',  #1594 ) ;
#5967 = VECTOR ( 'NONE', #29486, 1000.000000000000000 ) ;
#5968 = ORIENTED_EDGE ( 'NONE', *, *, #10161, .F. ) ;
#5969 = LINE ( 'NONE', #10383, #19014 ) ;
#5970 = CARTESIAN_POINT ( 'NONE',  ( 33.54145741815126058, -13.16751478770765793, -19.75123935038191192 ) ) ;
#5971 = DIRECTION ( 'NONE',  ( 0.9510565162951536422, 2.566386769018988816E-16, 0.3090169943749472292 ) ) ;
#5972 = CARTESIAN_POINT ( 'NONE',  ( 139.7287565553230309, -4.999999999999980460, -7.839745962155600267 ) ) ;
#5973 = CARTESIAN_POINT ( 'NONE',  ( 12.31319128649213646, 9.546177831575306527, -15.27906485473354792 ) ) ;
#5974 = EDGE_CURVE ( 'NONE', #18890, #20837, #960, .T. ) ;
#5975 = PLANE ( 'NONE',  #13494 ) ;
#5976 = ORIENTED_EDGE ( 'NONE', *, *, #1242, .F. ) ;
#5977 = CARTESIAN_POINT ( 'NONE',  ( 157.0152310637604955, -4.999999999999975131, -6.958068083716895558 ) ) ;
#5978 = ORIENTED_EDGE ( 'NONE', *, *, #19578, .F. ) ;
#5979 = VECTOR ( 'NONE', #2300, 1000.000000000000000 ) ;
#5980 = CARTESIAN_POINT ( 'NONE',  ( 12.73046782819888989, 7.614823354231524455, -14.94646497050939793 ) ) ;
#5981 = DIRECTION ( 'NONE',  ( -0.5877852522924731371, 0.000000000000000000, 0.8090169943749474513 ) ) ;
#5982 = DIRECTION ( 'NONE',  ( -1.000000000000000000, 0.000000000000000000, -0.000000000000000000 ) ) ;
#5983 = DIRECTION ( 'NONE',  ( -1.000000000000000000, 0.000000000000000000, -0.000000000000000000 ) ) ;
#5984 = EDGE_LOOP ( 'NONE', ( #28943, #21665, #1195, #13828, #12735 ) ) ;
#5985 = CARTESIAN_POINT ( 'NONE',  ( 12.83348778413740376, 9.536125428572121976, -16.14043921975381934 ) ) ;
#5986 = ORIENTED_EDGE ( 'NONE', *, *, #8660, .T. ) ;
#5987 = CARTESIAN_POINT ( 'NONE',  ( 35.54859390953724585, -21.18451583373416014, -16.11276402859391510 ) ) ;
#5988 = CARTESIAN_POINT ( 'NONE',  ( 20.51249478307574847, 1.942573248051725709, -13.31196225760961838 ) ) ;
#5989 = EDGE_LOOP ( 'NONE', ( #19822, #11466, #753, #3565 ) ) ;
#5990 = ORIENTED_EDGE ( 'NONE', *, *, #21425, .T. ) ;
#5991 = CARTESIAN_POINT ( 'NONE',  ( 159.7287565553229740, -1.999999999999972689, -25.16025403784440329 ) ) ;
#5992 = CIRCLE ( 'NONE', #18649, 2.500000000000002665 ) ;
#5993 = CARTESIAN_POINT ( 'NONE',  ( 27.50131297508284334, -11.63919202702402167, -19.74788458503752864 ) ) ;
#5994 = CARTESIAN_POINT ( 'NONE',  ( 8.000000000000000000, -4.618802153517027165, -4.285468820183664818 ) ) ;
#5995 = CARTESIAN_POINT ( 'NONE',  ( 103.8408967599626749, -4.999999999999989342, -75.44482764232697036 ) ) ;
#5996 = CARTESIAN_POINT ( 'NONE',  ( 28.73289915209718615, -4.972737245092835323, -15.12275039236161689 ) ) ;
#5997 = CARTESIAN_POINT ( 'NONE',  ( 23.26502027940742678, 3.673231887600847845, -16.77589761210995789 ) ) ;
#5998 = ORIENTED_EDGE ( 'NONE', *, *, #3032, .T. ) ;
#5999 = ORIENTED_EDGE ( 'NONE', *, *, #21306, .T. ) ;
#6000 = ORIENTED_EDGE ( 'NONE', *, *, #21516, .F. ) ;
#6001 = FACE_OUTER_BOUND ( 'NONE', #22884, .T. ) ;
#6002 = VECTOR ( 'NONE', #5476, 1000.000000000000000 ) ;
#6003 = DIRECTION ( 'NONE',  ( 1.000000000000000000, 0.000000000000000000, 0.000000000000000000 ) ) ;
#6004 = DIRECTION ( 'NONE',  ( 0.9510565162951535312, 2.566386769018988816E-16, -0.3090169943749475623 ) ) ;
#6005 = DIRECTION ( 'NONE',  ( -2.698458740408365879E-16, 1.000000000000000000, 0.000000000000000000 ) ) ;
#6006 = FACE_OUTER_BOUND ( 'NONE', #1713, .T. ) ;
#6007 = CARTESIAN_POINT ( 'NONE',  ( 163.6922820468853104, -4.999999999999973355, -9.266330736598359152 ) ) ;
#6008 = VECTOR ( 'NONE', #1208, 1000.000000000000000 ) ;
#6009 = CARTESIAN_POINT ( 'NONE',  ( 12.48979292151040177, 7.561326536588189207, -16.39201226339353212 ) ) ;
#6010 = CARTESIAN_POINT ( 'NONE',  ( 12.55500454421123457, 8.595009676161804890, -15.08633542003848049 ) ) ;
#6011 = CARTESIAN_POINT ( 'NONE',  ( 28.96558774451377971, -5.053040458581501859, -15.93506438242870971 ) ) ;
#6012 = ADVANCED_FACE ( 'NONE', ( #24015 ), #5226, .T. ) ;
#6013 = EDGE_CURVE ( 'NONE', #24548, #9707, #16675, .T. ) ;
#6014 = VERTEX_POINT ( 'NONE', #5686 ) ;
#6015 = DIRECTION ( 'NONE',  ( -0.000000000000000000, -0.000000000000000000, -1.000000000000000000 ) ) ;
#6016 = DIRECTION ( 'NONE',  ( 1.000000000000000000, 2.698458740408365879E-16, -1.110223024625156540E-16 ) ) ;
#6017 = ORIENTED_EDGE ( 'NONE', *, *, #10245, .T. ) ;
#6018 = LINE ( 'NONE', #8297, #22448 ) ;
#6019 = ADVANCED_FACE ( 'NONE', ( #3395 ), #2960, .T. ) ;
#6020 = CARTESIAN_POINT ( 'NONE',  ( -4.000000000000010658, -2.309401076758525573, -2.092734410091829034 ) ) ;
#6021 = DIRECTION ( 'NONE',  ( -0.9510565162951536422, -2.566386769018988816E-16, -0.3090169943749472292 ) ) ;
#6022 = EDGE_CURVE ( 'NONE', #314, #4943, #12385, .T. ) ;
#6024 = ORIENTED_EDGE ( 'NONE', *, *, #29168, .F. ) ;
#6023 = CARTESIAN_POINT ( 'NONE',  ( 25.77659985377941254, -6.250509680199615836, -13.67467641272277312 ) ) ;
#6025 = ORIENTED_EDGE ( 'NONE', *, *, #6948, .F. ) ;
#6026 = LINE ( 'NONE', #22352, #10017 ) ;
#6027 = CARTESIAN_POINT ( 'NONE',  ( 12.27679999902766284, 9.495116139066881900, -15.31073721177884650 ) ) ;
#6028 = CARTESIAN_POINT ( 'NONE',  ( 32.62126879184269512, -11.04717877266006987, -18.30218954475424908 ) ) ;
#6029 = CARTESIAN_POINT ( 'NONE',  ( 147.0152310637605524, -1.999999999999977129, -6.958068083716895558 ) ) ;
#6030 = CARTESIAN_POINT ( 'NONE',  ( 27.51942754507220812, -5.605608590038333006, -14.64806962472005658 ) ) ;
#6031 = CARTESIAN_POINT ( 'NONE',  ( 130.7287565553229456, -4.999999999999983125, 3.500000000000003109 ) ) ;
#6032 = CARTESIAN_POINT ( 'NONE',  ( 15.68163020692053422, 2.793964495486057409, -19.44966893625607085 ) ) ;
#6033 = ORIENTED_EDGE ( 'NONE', *, *, #28282, .F. ) ;
#6034 = CARTESIAN_POINT ( 'NONE',  ( 113.9712810924319797, -4.999999999999986677, -82.80498268490511293 ) ) ;
#6035 = EDGE_LOOP ( 'NONE', ( #19667, #11495, #14664, #1767, #10738 ) ) ;
#6036 = PRESENTATION_STYLE_ASSIGNMENT (( #3747 ) ) ;
#6037 = CARTESIAN_POINT ( 'NONE',  ( 25.84292692831908766, -2.469955994367391661, -17.24682881138801704 ) ) ;
#6038 = CARTESIAN_POINT ( 'NONE',  ( 25.33177305468611351, -7.180647579645999201, -12.45679661262278870 ) ) ;
#6039 = VECTOR ( 'NONE', #4014, 1000.000000000000000 ) ;
#6040 = ORIENTED_EDGE ( 'NONE', *, *, #27075, .T. ) ;
#6041 = CARTESIAN_POINT ( 'NONE',  ( -0.6543471694412855699, -8.859816792613662173, -0.4964154566688078751 ) ) ;
#6042 = LINE ( 'NONE', #20075, #17224 ) ;
#6043 = FACE_OUTER_BOUND ( 'NONE', #15318, .T. ) ;
#6044 = CARTESIAN_POINT ( 'NONE',  ( 127.7287565553229740, -1.999999999999982681, 0.5000000000000397460 ) ) ;
#6045 = DIRECTION ( 'NONE',  ( -2.698458740408365879E-16, 1.000000000000000000, 0.000000000000000000 ) ) ;
#6046 = DIRECTION ( 'NONE',  ( 0.000000000000000000, -0.4999999999999993894, 0.8660254037844389297 ) ) ;
#6047 = CARTESIAN_POINT ( 'NONE',  ( 23.04322939705109974, -6.346999004730295546, -16.23111451206203881 ) ) ;
#6048 = CARTESIAN_POINT ( 'NONE',  ( 17.78134717446047119, 9.288666448780150020, -20.14505390916605521 ) ) ;
#6049 = CARTESIAN_POINT ( 'NONE',  ( 35.79875902618127270, -19.81590490140210647, -21.40562824699871314 ) ) ;
#6050 = DIRECTION ( 'NONE',  ( -2.698458740408365879E-16, 1.000000000000000000, 0.000000000000000000 ) ) ;
#6051 = CARTESIAN_POINT ( 'NONE',  ( 9.843778300897430000, 16.74053286659246709, -16.57516421589427225 ) ) ;
#6052 = EDGE_CURVE ( 'NONE', #22459, #8937, #3432, .T. ) ;
#6053 = VECTOR ( 'NONE', #26711, 1000.000000000000000 ) ;
#6054 = DIRECTION ( 'NONE',  ( 0.000000000000000000, -1.000000000000000000, 0.000000000000000000 ) ) ;
#6055 = CARTESIAN_POINT ( 'NONE',  ( 2.645508037661892686, 7.710219529346620249, -4.931901280394563436 ) ) ;
#6056 = EDGE_CURVE ( 'NONE', #6774, #12566, #19405, .T. ) ;
#6057 = EDGE_CURVE ( 'NONE', #18517, #21669, #21405, .T. ) ;
#6058 = CARTESIAN_POINT ( 'NONE',  ( 9.661883245193708447, 16.25482579169019459, -17.91553454599451101 ) ) ;
#6059 = FACE_OUTER_BOUND ( 'NONE', #14935, .T. ) ;
#6060 = CARTESIAN_POINT ( 'NONE',  ( 172.2287565553229172, -1.999999999999969580, -20.83012701892220520 ) ) ;
#6061 = CARTESIAN_POINT ( 'NONE',  ( 11.45256130090833935, 9.362448956408465861, -15.86931324879919991 ) ) ;
#6062 = VERTEX_POINT ( 'NONE', #802 ) ;
#6063 = PLANE ( 'NONE',  #10995 ) ;
#6064 = CARTESIAN_POINT ( 'NONE',  ( 134.7287565553230024, -10.00000000000000711, -33.82050807568879947 ) ) ;
#6065 = CARTESIAN_POINT ( 'NONE',  ( 164.5152310637604387, -4.999999999999973355, -4.391296821672111328 ) ) ;
#6066 = ORIENTED_EDGE ( 'NONE', *, *, #29403, .T. ) ;
#6067 = VERTEX_POINT ( 'NONE', #657 ) ;
#6068 = CARTESIAN_POINT ( 'NONE',  ( 13.38031868501602872, 7.626265983139092874, -15.70730939156535655 ) ) ;
#6069 = CARTESIAN_POINT ( 'NONE',  ( 36.54859390953724585, -23.18451583373416014, -17.22552805718784441 ) ) ;
#6070 = CARTESIAN_POINT ( 'NONE',  ( 25.08912532741139501, -12.86307741315042108, -14.91192194027685147 ) ) ;
#6071 = CARTESIAN_POINT ( 'NONE',  ( 24.27430760268559595, -10.23567508289028716, -17.26834523416827949 ) ) ;
#6072 = CARTESIAN_POINT ( 'NONE',  ( 163.6922820468852819, -1.999999999999973133, 2.247092850131519715 ) ) ;
#6073 = FACE_OUTER_BOUND ( 'NONE', #24845, .T. ) ;
#6074 = FACE_OUTER_BOUND ( 'NONE', #13336, .T. ) ;
#6075 = VECTOR ( 'NONE', #17923, 1000.000000000000000 ) ;
#6076 = ORIENTED_EDGE ( 'NONE', *, *, #26828, .T. ) ;
#6077 = ORIENTED_EDGE ( 'NONE', *, *, #2755, .F. ) ;
#6078 = DIRECTION ( 'NONE',  ( -0.5877852522924731371, 0.000000000000000000, 0.8090169943749474513 ) ) ;
#6079 = DIRECTION ( 'NONE',  ( -2.698458740408365879E-16, 1.000000000000000000, 0.000000000000000000 ) ) ;
#6080 = DIRECTION ( 'NONE',  ( -0.000000000000000000, -0.000000000000000000, -1.000000000000000000 ) ) ;
#6081 = DIRECTION ( 'NONE',  ( 1.000000000000000000, 2.891205793294675861E-16, 0.000000000000000000 ) ) ;
#6082 = CARTESIAN_POINT ( 'NONE',  ( 13.15105351193492744, 8.582979361647906202, -15.89003778131599098 ) ) ;
#6083 = CARTESIAN_POINT ( 'NONE',  ( 33.61336211056222112, -12.49217533051321993, -18.72970452740151970 ) ) ;
#6084 = CARTESIAN_POINT ( 'NONE',  ( 8.965340528640792783, 16.85640380871598509, -17.50303937619785444 ) ) ;
#6085 = ORIENTED_EDGE ( 'NONE', *, *, #17585, .F. ) ;
#6086 = EDGE_CURVE ( 'NONE', #29734, #26271, #21697, .T. ) ;
#6087 = EDGE_CURVE ( 'NONE', #23116, #17842, #509, .T. ) ;
#6088 = CARTESIAN_POINT ( 'NONE',  ( 29.72799312938100513, -7.689056491358781997, -15.42978383025728384 ) ) ;
#6089 = ADVANCED_FACE ( 'NONE', ( #9798 ), #14669, .T. ) ;
#6090 = CARTESIAN_POINT ( 'NONE',  ( 12.86840956200995301, 9.516103707707461723, -16.11530999810414500 ) ) ;
#6091 = FACE_BOUND ( 'NONE', #15265, .T. ) ;
#6092 = ADVANCED_FACE ( 'NONE', ( #28610 ), #7667, .T. ) ;
#6093 = ORIENTED_EDGE ( 'NONE', *, *, #7697, .T. ) ;
#6094 = CARTESIAN_POINT ( 'NONE',  ( 172.2287565553228603, -1.999999999999970468, -3.509618943233403510 ) ) ;
#6095 = VECTOR ( 'NONE', #14244, 1000.000000000000000 ) ;
#6096 = CARTESIAN_POINT ( 'NONE',  ( 11.46269231744662420, 9.315986823159681407, -15.86512371708112212 ) ) ;
#6097 = CARTESIAN_POINT ( 'NONE',  ( 132.0152310637605808, -10.00000000000000711, -24.27857615940569147 ) ) ;
#6098 = ORIENTED_EDGE ( 'NONE', *, *, #9758, .F. ) ;
#6099 = LINE ( 'NONE', #8528, #29641 ) ;
#6100 = ORIENTED_EDGE ( 'NONE', *, *, #3033, .T. ) ;
#6101 = CARTESIAN_POINT ( 'NONE',  ( 13.12299649507002464, 8.570581087883812899, -15.91239967140973022 ) ) ;
#6102 = ORIENTED_EDGE ( 'NONE', *, *, #9626, .T. ) ;
#6103 = CARTESIAN_POINT ( 'NONE',  ( 15.09088459799990822, 3.595497735170159803, -19.35696164441904443 ) ) ;
#6104 = CARTESIAN_POINT ( 'NONE',  ( 22.44359388949645151, 4.989503210053415572, -18.93028356096972686 ) ) ;
#6105 = FACE_OUTER_BOUND ( 'NONE', #5799, .T. ) ;
#6106 = EDGE_LOOP ( 'NONE', ( #8573, #12990, #11398, #46 ) ) ;
#6107 = CARTESIAN_POINT ( 'NONE',  ( 36.13838427452936486, -20.34166123773320578, -20.43658233646779365 ) ) ;
#6108 = ORIENTED_EDGE ( 'NONE', *, *, #24279, .F. ) ;
#6109 = CARTESIAN_POINT ( 'NONE',  ( 25.57370974413349884, -0.4222200280313516685, -16.88676729435558599 ) ) ;
#6110 = ORIENTED_EDGE ( 'NONE', *, *, #17913, .T. ) ;
#6111 = DIRECTION ( 'NONE',  ( -0.000000000000000000, 0.000000000000000000, 1.000000000000000000 ) ) ;
#6112 = FACE_BOUND ( 'NONE', #4092, .T. ) ;
#6113 = VECTOR ( 'NONE', #23197, 999.9999999999998863 ) ;
#6114 = ORIENTED_EDGE ( 'NONE', *, *, #18133, .T. ) ;
#6115 = LINE ( 'NONE', #24746, #21089 ) ;
#6116 = CARTESIAN_POINT ( 'NONE',  ( 35.03938282813840743, -19.89690018161999419, -20.20402626681843117 ) ) ;
#6117 = CARTESIAN_POINT ( 'NONE',  ( 151.1922820468854241, -4.999999999999976907, -22.25671179336496053 ) ) ;
#6118 = EDGE_LOOP ( 'NONE', ( #27463, #20840, #21549, #13025 ) ) ;
#6119 = ORIENTED_EDGE ( 'NONE', *, *, #20622, .F. ) ;
#6120 = DIRECTION ( 'NONE',  ( -0.8090169943749474513, -2.183098979609982436E-16, 0.5877852522924731371 ) ) ;
#6121 = CARTESIAN_POINT ( 'NONE',  ( 12.68070129083326236, 9.708587077508630259, -14.98615289428795094 ) ) ;
#6122 = CARTESIAN_POINT ( 'NONE',  ( 35.54859125455464408, -23.18450390630307822, -18.42126094939176895 ) ) ;
#6123 = EDGE_CURVE ( 'NONE', #10558, #22420, #10242, .T. ) ;
#6124 = CIRCLE ( 'NONE', #13433, 4.250000000000003553 ) ;
#6125 = LINE ( 'NONE', #128, #24662 ) ;
#6126 = EDGE_LOOP ( 'NONE', ( #14213, #22314, #11910, #19662 ) ) ;
#6127 = DIRECTION ( 'NONE',  ( -0.8090169943749474513, -2.183098979609982436E-16, -0.5877852522924731371 ) ) ;
#6128 = ORIENTED_EDGE ( 'NONE', *, *, #21680, .F. ) ;
#6129 = VECTOR ( 'NONE', #1375, 999.9999999999998863 ) ;
#6130 = CARTESIAN_POINT ( 'NONE',  ( 10.68833914101186444, 8.961267084878116407, -16.40255713880337751 ) ) ;
#6131 = PLANE ( 'NONE',  #19539 ) ;
#6132 = PLANE ( 'NONE',  #17425 ) ;
#6133 = DIRECTION ( 'NONE',  ( -0.5877852522924731371, -1.586114251531760235E-16, 0.8090169943749474513 ) ) ;
#6134 = EDGE_LOOP ( 'NONE', ( #6660, #11581, #9398 ) ) ;
#6135 = CARTESIAN_POINT ( 'NONE',  ( 12.93646321750111916, 9.546177831575306527, -16.06107003375496944 ) ) ;
#6136 = ORIENTED_EDGE ( 'NONE', *, *, #18264, .F. ) ;
#6138 = CARTESIAN_POINT ( 'NONE',  ( 35.57309713841538468, -16.80212557611773505, -19.25277297559858525 ) ) ;
#6137 = AXIS2_PLACEMENT_3D ( 'NONE', #10592, #19901, #29268 ) ;
#6139 = CARTESIAN_POINT ( 'NONE',  ( 24.66978787416869068, -0.3063955544261361963, -14.42797892638687784 ) ) ;
#6140 = VERTEX_POINT ( 'NONE', #17566 ) ;
#6141 = ORIENTED_EDGE ( 'NONE', *, *, #10477, .T. ) ;
#6142 = AXIS2_PLACEMENT_3D ( 'NONE', #5028, #12042, #2912 ) ;
#6143 = CARTESIAN_POINT ( 'NONE',  ( 134.5152310637605808, -4.999999999999981348, -2.627941064794695691 ) ) ;
#6144 = CARTESIAN_POINT ( 'NONE',  ( 134.7287565553230024, -10.00000000000000711, -16.50000000000000000 ) ) ;
#6145 = CARTESIAN_POINT ( 'NONE',  ( 131.1922820468854241, -4.999999999999982236, -10.74328820663507322 ) ) ;
#6146 = CARTESIAN_POINT ( 'NONE',  ( 26.53548354394225228, -12.81408696708834860, -17.07385457597708367 ) ) ;
#6147 = AXIS2_PLACEMENT_3D ( 'NONE', #16087, #4503, #28639 ) ;
#6148 = CARTESIAN_POINT ( 'NONE',  ( 19.77054944300549622, 4.331964111641410042, -19.42026316723860901 ) ) ;
#6149 = ORIENTED_EDGE ( 'NONE', *, *, #2491, .T. ) ;
#6150 = ORIENTED_EDGE ( 'NONE', *, *, #21754, .T. ) ;
#6151 = EDGE_CURVE ( 'NONE', #3855, #25397, #10396, .T. ) ;
#6152 = DIRECTION ( 'NONE',  ( -1.000000000000000000, 0.000000000000000000, 0.000000000000000000 ) ) ;
#6153 = PRODUCT_DEFINITION ( 'UNKNOWN', '', #13639, #14055 ) ;
#6154 = FILL_AREA_STYLE ('',( #20035 ) ) ;
#6155 = AXIS2_PLACEMENT_3D ( 'NONE', #21450, #25892, #16864 ) ;
#6156 = DIRECTION ( 'NONE',  ( -2.698458740408365879E-16, 1.000000000000000000, 0.000000000000000000 ) ) ;
#6157 = LINE ( 'NONE', #24781, #29670 ) ;
#6158 = CARTESIAN_POINT ( 'NONE',  ( 157.0152310637604387, -10.00000000000000000, -0.06116980274991495881 ) ) ;
#6159 = VECTOR ( 'NONE', #28472, 1000.000000000000000 ) ;
#6160 = LINE ( 'NONE', #8287, #11433 ) ;
#6161 = VECTOR ( 'NONE', #23741, 1000.000000000000000 ) ;
#6162 = CARTESIAN_POINT ( 'NONE',  ( 11.21386537247953363, 9.137237924250291243, -17.24575182870169598 ) ) ;
#6163 = CARTESIAN_POINT ( 'NONE',  ( 12.46899830068120352, 8.557956911948249257, -15.15481108270911825 ) ) ;
#6164 = CARTESIAN_POINT ( 'NONE',  ( 26.53548354394225228, -12.81408696708834860, -17.07385457597708367 ) ) ;
#6165 = VERTEX_POINT ( 'NONE', #29219 ) ;
#6166 = DIRECTION ( 'NONE',  ( 1.000000000000000000, 2.891205793294675861E-16, 0.000000000000000000 ) ) ;
#6167 = DIRECTION ( 'NONE',  ( -0.5877852522924731371, 0.000000000000000000, 0.8090169943749474513 ) ) ;
#6168 = ORIENTED_EDGE ( 'NONE', *, *, #3675, .T. ) ;
#6169 = CARTESIAN_POINT ( 'NONE',  ( 9.641350810849047548, 17.66889113945805789, -17.91796598306941135 ) ) ;
#6170 = DIRECTION ( 'NONE',  ( 1.000000000000000000, 0.000000000000000000, -1.387778780781445676E-16 ) ) ;
#6171 = CARTESIAN_POINT ( 'NONE',  ( 139.5152310637606092, -4.999999999999979572, -28.60870317832789311 ) ) ;
#6172 = CARTESIAN_POINT ( 'NONE',  ( 23.61827771231835982, -0.6465389018800060672, -13.57143891608981612 ) ) ;
#6173 = ORIENTED_EDGE ( 'NONE', *, *, #14540, .F. ) ;
#6174 = DIRECTION ( 'NONE',  ( 1.110223024625156540E-16, 2.995891024602366092E-32, 1.000000000000000000 ) ) ;
#6175 = CARTESIAN_POINT ( 'NONE',  ( 11.05541531668977662, 17.68942339022145305, -17.97192418671890835 ) ) ;
#6176 = DIRECTION ( 'NONE',  ( -2.698458740408365879E-16, 1.000000000000000000, 0.000000000000000000 ) ) ;
#6177 = CARTESIAN_POINT ( 'NONE',  ( 142.0152310637606092, -10.00000000000000355, -24.27857615940569147 ) ) ;
#6178 = CIRCLE ( 'NONE', #20295, 8.000000000000005329 ) ;
#6179 = CARTESIAN_POINT ( 'NONE',  ( 25.77659985377941254, -6.250509680199615836, -13.67467641272277312 ) ) ;
#6180 = LINE ( 'NONE', #15168, #22295 ) ;
#6181 = CARTESIAN_POINT ( 'NONE',  ( 15.35879474092683594, 2.467707791974911302, -18.63256289774529151 ) ) ;
#6182 = EDGE_LOOP ( 'NONE', ( #27277, #9247, #2340, #21506, #17026 ) ) ;
#6183 = CARTESIAN_POINT ( 'NONE',  ( 35.54859390954303677, -22.18451583373416014, -15.55638201429745848 ) ) ;
#6184 = ORIENTED_EDGE ( 'NONE', *, *, #13385, .T. ) ;
#6185 = CARTESIAN_POINT ( 'NONE',  ( 19.14398323884976350, 7.495936751868839565, -14.71076302495156263 ) ) ;
#6186 = CONICAL_SURFACE ( 'NONE', #10541, 5.000000000000000000, 0.2131563744996336218 ) ;
#6187 = CARTESIAN_POINT ( 'NONE',  ( 25.20714760837546464, -2.665945389627573991, -12.53535894516201665 ) ) ;
#6188 = VECTOR ( 'NONE', #4620, 1000.000000000000000 ) ;
#6189 = ORIENTED_EDGE ( 'NONE', *, *, #14859, .T. ) ;
#6190 = ADVANCED_FACE ( 'NONE', ( #20014 ), #29692, .T. ) ;
#6191 = ADVANCED_FACE ( 'NONE', ( #10705, #13294, #15729 ), #10546, .F. ) ;
#6192 = CARTESIAN_POINT ( 'NONE',  ( 24.60501232743784783, -9.531698448777172317, -16.22453333552994792 ) ) ;
#6193 = ADVANCED_FACE ( 'NONE', ( #27073 ), #15270, .T. ) ;
#6194 = EDGE_CURVE ( 'NONE', #16074, #7950, #22613, .T. ) ;
#6195 = CARTESIAN_POINT ( 'NONE',  ( 158.6922820468853388, -10.00000000000000000, -9.266330736598359152 ) ) ;
#6196 = CARTESIAN_POINT ( 'NONE',  ( 159.5152310637604955, -9.999999999999998224, -11.28819510263909542 ) ) ;
#6197 = CARTESIAN_POINT ( 'NONE',  ( 171.1922820468853388, -1.999999999999970468, -22.25671179336496053 ) ) ;
#6198 = FACE_OUTER_BOUND ( 'NONE', #8677, .T. ) ;
#6199 = AXIS2_PLACEMENT_3D ( 'NONE', #18966, #7226, #5227 ) ;
#6200 = CARTESIAN_POINT ( 'NONE',  ( 9.641350810849047548, 17.66889113945805789, -17.95086732675817132 ) ) ;
#6201 = CARTESIAN_POINT ( 'NONE',  ( 27.30941123812745275, -4.721684434479056947, -15.35818731037458029 ) ) ;
#6202 = CARTESIAN_POINT ( 'NONE',  ( 13.93479307118181509, 9.207276677253689812, -14.11477394318545286 ) ) ;
#6203 = CARTESIAN_POINT ( 'NONE',  ( 34.69314741404605229, -14.84897758684750890, -21.07142838010442176 ) ) ;
#6204 = DIRECTION ( 'NONE',  ( 0.8660254037844375974, -0.5000000000000016653, 0.000000000000000000 ) ) ;
#6205 = VECTOR ( 'NONE', #17238, 1000.000000000000000 ) ;
#6206 = CARTESIAN_POINT ( 'NONE',  ( 12.46899830068120352, 8.557956911948249257, -15.15481108270911825 ) ) ;
#6207 = LINE ( 'NONE', #25124, #18077 ) ;
#6208 = FACE_OUTER_BOUND ( 'NONE', #16911, .T. ) ;
#6209 = CARTESIAN_POINT ( 'NONE',  ( 13.19188795686497429, 8.601024833420110483, -15.85749200792911573 ) ) ;
#6210 = CARTESIAN_POINT ( 'NONE',  ( 3.319543390096043378, -7.321065037175453760, -4.983111142572217211 ) ) ;
#6211 = ORIENTED_EDGE ( 'NONE', *, *, #27803, .T. ) ;
#6212 = CARTESIAN_POINT ( 'NONE',  ( 18.23030615683139644, -5.000000000000012434, -56.10711313654469024 ) ) ;
#6213 = CARTESIAN_POINT ( 'NONE',  ( 10.17605321708455257, 15.21667774575863419, -16.39719424528293246 ) ) ;
#6214 = ORIENTED_EDGE ( 'NONE', *, *, #23686, .F. ) ;
#6215 = CARTESIAN_POINT ( 'NONE',  ( -4.000000000000001776, -1.286498119741308097E-15, 9.480888224575629408 ) ) ;
#6216 = DIRECTION ( 'NONE',  ( 0.9510565162951536422, 2.566386769018988816E-16, 0.3090169943749472292 ) ) ;
#6217 = DIRECTION ( 'NONE',  ( -0.9510565162951536422, -2.566386769018988816E-16, -0.3090169943749472292 ) ) ;
#6218 = ORIENTED_EDGE ( 'NONE', *, *, #6821, .T. ) ;
#6219 = CARTESIAN_POINT ( 'NONE',  ( 8.944584683310379702, 16.95159276115599667, -17.91752729848688830 ) ) ;
#6220 = CARTESIAN_POINT ( 'NONE',  ( 35.69176435403931436, -19.33523451612313693, -21.37328632439622922 ) ) ;
#6221 = CARTESIAN_POINT ( 'NONE',  ( 22.63682584648026008, 4.680144189823682410, -16.86151017930854223 ) ) ;
#6222 = CARTESIAN_POINT ( 'NONE',  ( 27.50962693642323131, -9.092369620780022643, -12.61635453147917474 ) ) ;
#6223 = AXIS2_PLACEMENT_3D ( 'NONE', #12751, #17037, #5447 ) ;
#6224 = DIRECTION ( 'NONE',  ( -0.5877852522924731371, -1.586114251531760728E-16, -0.8090169943749474513 ) ) ;
#6225 = CARTESIAN_POINT ( 'NONE',  ( 167.2287565553229740, -9.999999999999996447, -29.49038105676660493 ) ) ;
#6226 = LINE ( 'NONE', #22564, #17185 ) ;
#6227 = CARTESIAN_POINT ( 'NONE',  ( 17.76107737582129431, 3.703408080355245158, -15.36634439411934316 ) ) ;
#6228 = ADVANCED_FACE ( 'NONE', ( #8256 ), #1412, .T. ) ;
#6229 = EDGE_CURVE ( 'NONE', #29408, #10756, #1711, .T. ) ;
#6230 = ADVANCED_FACE ( 'NONE', ( #3692 ), #6131, .T. ) ;
#6231 = ORIENTED_EDGE ( 'NONE', *, *, #30222, .F. ) ;
#6232 = EDGE_CURVE ( 'NONE', #10747, #16128, #17859, .T. ) ;
#6233 = CARTESIAN_POINT ( 'NONE',  ( 129.5152310637605808, -10.00000000000000888, -28.60870317832789311 ) ) ;
#6234 = VECTOR ( 'NONE', #18342, 1000.000000000000000 ) ;
#6235 = SHAPE_REPRESENTATION ( 'torque nut 08_iso_ISO 10511-M5-N', ( #13190 ), #1965 ) ;
#6236 = DIRECTION ( 'NONE',  ( -0.000000000000000000, -0.000000000000000000, -1.000000000000000000 ) ) ;
#6237 = DIRECTION ( 'NONE',  ( -0.5877852522924731371, 0.000000000000000000, 0.8090169943749474513 ) ) ;
#6238 = CARTESIAN_POINT ( 'NONE',  ( 12.22285885739602662, 8.868278133530205665, -16.57678160000113721 ) ) ;
#6239 = CARTESIAN_POINT ( 'NONE',  ( 35.40392844931823646, -20.53461055239511879, -19.22110946685632271 ) ) ;
#6240 = ORIENTED_EDGE ( 'NONE', *, *, #25702, .T. ) ;
#6241 = CARTESIAN_POINT ( 'NONE',  ( 9.057417708256320310, 16.43412612588882027, -17.11704294810955318 ) ) ;
#6242 = ORIENTED_EDGE ( 'NONE', *, *, #21166, .T. ) ;
#6243 = AXIS2_PLACEMENT_3D ( 'NONE', #13325, #29575, #2322 ) ;
#6244 = CARTESIAN_POINT ( 'NONE',  ( 27.44219139316946965, -6.774709612358828181, -18.29578255718776703 ) ) ;
#6245 = CARTESIAN_POINT ( 'NONE',  ( 10.35864918915110877, 16.97212501191939538, -17.97192418671891190 ) ) ;
#6246 = CARTESIAN_POINT ( 'NONE',  ( 149.5152310637604955, -10.00000000000000178, -4.391296821672111328 ) ) ;
#6247 = ORIENTED_EDGE ( 'NONE', *, *, #28616, .T. ) ;
#6248 = TOROIDAL_SURFACE ( 'NONE', #13052, 7.000000000000000888, 2.000000000000000000 ) ;
#6249 = CARTESIAN_POINT ( 'NONE',  ( 142.2287565553230024, -10.00000000000000533, -3.509618943233403510 ) ) ;
#6250 = CARTESIAN_POINT ( 'NONE',  ( -1.310841663519413114, 0.000000000000000000, 0.000000000000000000 ) ) ;
#6251 = DIRECTION ( 'NONE',  ( 0.9510565162951536422, 0.000000000000000000, -0.3090169943749475623 ) ) ;
#6252 = EDGE_LOOP ( 'NONE', ( #16969, #7148, #15001, #14025 ) ) ;
#6253 = DIRECTION ( 'NONE',  ( 1.000000000000000000, 4.440892098500622217E-16, 0.000000000000000000 ) ) ;
#6254 = EDGE_LOOP ( 'NONE', ( #18779, #18525, #7670, #21521, #10674, #3039 ) ) ;
#6255 = CARTESIAN_POINT ( 'NONE',  ( 13.23272240178861381, 8.619070305187777947, -15.82494623455082916 ) ) ;
#6256 = CARTESIAN_POINT ( 'NONE',  ( 15.83402620853355636, 4.298615461832955731, -20.35054180922590916 ) ) ;
#6257 = CARTESIAN_POINT ( 'NONE',  ( 21.88956083454650781, 5.816198478639956093, -14.73130718433538178 ) ) ;
#6258 = VERTEX_POINT ( 'NONE', #15118 ) ;
#6259 = CARTESIAN_POINT ( 'NONE',  ( 154.5152310637604671, -10.00000000000000178, -4.391296821672111328 ) ) ;
#6260 = ORIENTED_EDGE ( 'NONE', *, *, #24740, .T. ) ;
#6261 = DIRECTION ( 'NONE',  ( 0.9510565162951535312, 2.566386769018988816E-16, -0.3090169943749475623 ) ) ;
#6262 = CARTESIAN_POINT ( 'NONE',  ( 24.92864811393110358, -0.2441600445015326137, -14.78813717129899885 ) ) ;
#6263 = EDGE_CURVE ( 'NONE', #27224, #23986, #24760, .T. ) ;
#6264 = VECTOR ( 'NONE', #3364, 1000.000000000000000 ) ;
#6265 = EDGE_CURVE ( 'NONE', #4310, #16894, #27385, .T. ) ;
#6266 = ADVANCED_FACE ( 'NONE', ( #20304, #20155 ), #8555, .F. ) ;
#6267 = DIRECTION ( 'NONE',  ( 0.000000000000000000, -2.775557561562890735E-17, 1.000000000000000000 ) ) ;
#6268 = ADVANCED_FACE ( 'NONE', ( #25058 ), #27232, .T. ) ;
#6269 = PLANE ( 'NONE',  #3087 ) ;
#6270 = VECTOR ( 'NONE', #21492, 1000.000000000000000 ) ;
#6271 = EDGE_LOOP ( 'NONE', ( #28727, #8049, #22630, #25535 ) ) ;
#6272 = CARTESIAN_POINT ( 'NONE',  ( 157.0152310637605524, -4.999999999999975131, -24.27857615940569502 ) ) ;
#6273 = CARTESIAN_POINT ( 'NONE',  ( 32.54305136433941215, -11.03529315477374517, -18.08112484791816499 ) ) ;
#6274 = LINE ( 'NONE', #13870, #29277 ) ;
#6275 = ORIENTED_EDGE ( 'NONE', *, *, #21485, .T. ) ;
#6276 = FACE_OUTER_BOUND ( 'NONE', #8405, .T. ) ;
#6277 = CARTESIAN_POINT ( 'NONE',  ( 11.05541531668977662, 17.68942339022145305, -17.97192418671890835 ) ) ;
#6278 = CARTESIAN_POINT ( 'NONE',  ( 33.10952763335142635, -11.62914684427059697, -19.38687730282833499 ) ) ;
#6279 = ORIENTED_EDGE ( 'NONE', *, *, #9714, .F. ) ;
#6280 = CARTESIAN_POINT ( 'NONE',  ( -24.00000000000017053, 34.64101615137744972, -10.00000000000000000 ) ) ;
#6281 = CARTESIAN_POINT ( 'NONE',  ( 10.66984875114861886, 9.039338215604900029, -16.41071671300888823 ) ) ;
#6282 = DIRECTION ( 'NONE',  ( -1.000000000000000000, 0.000000000000000000, 0.000000000000000000 ) ) ;
#6283 = DIRECTION ( 'NONE',  ( 0.9510565162951535312, 2.566386769018988816E-16, -0.3090169943749475623 ) ) ;
#6284 = EDGE_LOOP ( 'NONE', ( #27724, #3824, #23982, #27001 ) ) ;
#6285 = DIRECTION ( 'NONE',  ( -2.698458740408365879E-16, 1.000000000000000000, 0.000000000000000000 ) ) ;
#6286 = ORIENTED_EDGE ( 'NONE', *, *, #28912, .T. ) ;
#6287 = CARTESIAN_POINT ( 'NONE',  ( 13.08618951557147803, 9.612344561400664844, -15.94173553134588595 ) ) ;
#6288 = VECTOR ( 'NONE', #22244, 1000.000000000000000 ) ;
#6289 = CARTESIAN_POINT ( 'NONE',  ( 36.54517214193456454, -21.16914364445853280, -18.53042016804813841 ) ) ;
#6290 = CARTESIAN_POINT ( 'NONE',  ( 23.61827771231835982, -0.6465389018800060672, -13.57143891608981612 ) ) ;
#6291 = ORIENTED_EDGE ( 'NONE', *, *, #22136, .T. ) ;
#6292 = CARTESIAN_POINT ( 'NONE',  ( 20.00000000000017053, 34.64101615137744972, 12.00000000000000178 ) ) ;
#6293 = CARTESIAN_POINT ( 'NONE',  ( 8.000000000000014211, -3.098204225878181006, -4.684209322808117193 ) ) ;
#6294 = AXIS2_PLACEMENT_3D ( 'NONE', #22185, #1295, #21889 ) ;
#6295 = DIRECTION ( 'NONE',  ( -0.5877852522924731371, 0.000000000000000000, 0.8090169943749474513 ) ) ;
#6296 = AXIS2_PLACEMENT_3D ( 'NONE', #20170, #19570, #26618 ) ;
#6297 = CARTESIAN_POINT ( 'NONE',  ( 28.56280713547801398, -4.978584871567802494, -14.74258920993753641 ) ) ;
#6298 = CARTESIAN_POINT ( 'NONE',  ( 26.30156876094583396, -3.312801620251602852, -13.23872229457767169 ) ) ;
#6299 = EDGE_CURVE ( 'NONE', #10211, #14083, #22768, .T. ) ;
#6300 = EDGE_CURVE ( 'NONE', #19520, #17576, #6895, .T. ) ;
#6302 = VERTEX_POINT ( 'NONE', #9453 ) ;
#6301 = EDGE_CURVE ( 'NONE', #14224, #7426, #18170, .T. ) ;
#6303 = ORIENTED_EDGE ( 'NONE', *, *, #10903, .F. ) ;
#6304 = DIRECTION ( 'NONE',  ( -0.000000000000000000, -0.000000000000000000, -1.000000000000000000 ) ) ;
#6305 = VECTOR ( 'NONE', #8594, 1000.000000000000000 ) ;
#6306 = CARTESIAN_POINT ( 'NONE',  ( -20.00000000000017053, 34.64101615137744972, -10.00000000000000000 ) ) ;
#6307 = PLANE ( 'NONE',  #19178 ) ;
#6308 = DIRECTION ( 'NONE',  ( -0.5000000000000051070, 1.060575238724903217E-16, -0.8660254037844355990 ) ) ;
#6309 = AXIS2_PLACEMENT_3D ( 'NONE', #6158, #12712, #29562 ) ;
#6310 = CARTESIAN_POINT ( 'NONE',  ( 143.6922820468854525, -10.00000000000000355, -15.07341522555727664 ) ) ;
#6311 = DIRECTION ( 'NONE',  ( 0.000000000000000000, -2.775557561562890735E-17, 1.000000000000000000 ) ) ;
#6312 = CARTESIAN_POINT ( 'NONE',  ( 11.23176012633392595, 9.056260211165422902, -17.23826859254635835 ) ) ;
#6313 = CARTESIAN_POINT ( 'NONE',  ( 13.04501788334644630, 8.811555337407297017, -14.69578613943112799 ) ) ;
#6314 = VECTOR ( 'NONE', #418, 1000.000000000000000 ) ;
#6315 = DIRECTION ( 'NONE',  ( -0.9773680663943724589, 3.177847737406116550E-17, -0.2115458881484710285 ) ) ;
#6316 = ORIENTED_EDGE ( 'NONE', *, *, #22458, .T. ) ;
#6317 = CARTESIAN_POINT ( 'NONE',  ( 158.6922820468854241, -1.999999999999972689, -32.39392330124607611 ) ) ;
#6318 = LINE ( 'NONE', #27414, #1317 ) ;
#6319 = ORIENTED_EDGE ( 'NONE', *, *, #13892, .F. ) ;
#6320 = CARTESIAN_POINT ( 'NONE',  ( 9.641351654859628084, 17.66888726871794191, -17.91235298298990841 ) ) ;
#6321 = CARTESIAN_POINT ( 'NONE',  ( 0.000000000000000000, 0.000000000000000000, 18.00000000000000000 ) ) ;
#6322 = LINE ( 'NONE', #13326, #25856 ) ;
#6323 = CARTESIAN_POINT ( 'NONE',  ( 162.0152310637604955, -9.999999999999998224, -15.61832212156129707 ) ) ;
#6325 = ORIENTED_EDGE ( 'NONE', *, *, #16896, .T. ) ;
#6324 = CARTESIAN_POINT ( 'NONE',  ( 22.16846437878366061, -4.107540447007581363, -19.06500358040360865 ) ) ;
#6326 = ORIENTED_EDGE ( 'NONE', *, *, #11426, .F. ) ;
#6327 = DIRECTION ( 'NONE',  ( 0.5877852522924731371, 1.586114251531760728E-16, -0.8090169943749474513 ) ) ;
#6328 = CARTESIAN_POINT ( 'NONE',  ( 12.24562038388194551, 9.516309650702005740, -15.33292062045688908 ) ) ;
#6329 = EDGE_CURVE ( 'NONE', #11088, #10839, #5899, .T. ) ;
#6330 = CARTESIAN_POINT ( 'NONE',  ( 33.41663030065195272, -12.60673267154789201, -19.71350710734569134 ) ) ;
#6331 = CARTESIAN_POINT ( 'NONE',  ( -4.000000000000004441, -1.549102112939100273, -0.1578953385959418754 ) ) ;
#6332 = CARTESIAN_POINT ( 'NONE',  ( 27.95388715220626707, -5.541385876428546631, -15.41148221666858831 ) ) ;
#6333 = CARTESIAN_POINT ( 'NONE',  ( 147.0152310637605808, -1.999999999999976241, -26.04193191628311155 ) ) ;
#6334 = CARTESIAN_POINT ( 'NONE',  ( 20.77099883799555258, -1.523348603316126981, -18.27480029096593839 ) ) ;
#6335 = ORIENTED_EDGE ( 'NONE', *, *, #26532, .F. ) ;
#6336 = CARTESIAN_POINT ( 'NONE',  ( 172.7287565553229456, -4.999999999999971578, 3.500000000000003109 ) ) ;
#6337 = AXIS2_PLACEMENT_3D ( 'NONE', #4844, #25920, #18737 ) ;
#6338 = CARTESIAN_POINT ( 'NONE',  ( 16.96387855261641775, 8.441957738943033362, -20.67322241009641814 ) ) ;
#6339 = CARTESIAN_POINT ( 'NONE',  ( 29.18140637672732396, -9.206484972055292815, -13.74645275385354815 ) ) ;
#6340 = VECTOR ( 'NONE', #11029, 1000.000000000000000 ) ;
#6341 = VECTOR ( 'NONE', #5906, 1000.000000000000000 ) ;
#6342 = EDGE_CURVE ( 'NONE', #11008, #929, #11155, .T. ) ;
#6343 = VECTOR ( 'NONE', #11063, 1000.000000000000000 ) ;
#6344 = ORIENTED_EDGE ( 'NONE', *, *, #26926, .T. ) ;
#6345 = CARTESIAN_POINT ( 'NONE',  ( 29.82081855766934453, -7.722587238354316597, -15.76009366473342332 ) ) ;
#6346 = CARTESIAN_POINT ( 'NONE',  ( 174.5152310637604387, -9.999999999999994671, -11.28819510263909542 ) ) ;
#6347 = EDGE_LOOP ( 'NONE', ( #29434, #17755 ) ) ;
#6348 = ORIENTED_EDGE ( 'NONE', *, *, #11037, .T. ) ;
#6349 = VECTOR ( 'NONE', #21442, 1000.000000000000000 ) ;
#6350 = DIRECTION ( 'NONE',  ( 0.000000000000000000, 0.000000000000000000, 1.000000000000000000 ) ) ;
#6351 = CARTESIAN_POINT ( 'NONE',  ( 137.0152310637605808, -1.999999999999979572, -17.38167787843870826 ) ) ;
#6352 = CARTESIAN_POINT ( 'NONE',  ( 133.6922820468854241, -1.999999999999981348, -15.07341522555727309 ) ) ;
#6353 = LINE ( 'NONE', #8476, #4334 ) ;
#6354 = AXIS2_PLACEMENT_3D ( 'NONE', #7353, #14043, #9321 ) ;
#6355 = CARTESIAN_POINT ( 'NONE',  ( 26.37829838608531219, -4.974601419860719353, -14.31557877768424092 ) ) ;
#6356 = CARTESIAN_POINT ( 'NONE',  ( 20.37871551743239351, 7.600776799596193456, -17.08157252577618479 ) ) ;
#6357 = CARTESIAN_POINT ( 'NONE',  ( 32.66938126488236804, -9.629547215342803668, -18.20796273874843507 ) ) ;
#6359 = LINE ( 'NONE', #25122, #23682 ) ;
#6358 = CIRCLE ( 'NONE', #14130, 4.250000000000003553 ) ;
#6360 = CARTESIAN_POINT ( 'NONE',  ( 11.47304865262203499, 9.268493388164605662, -15.86084085272616484 ) ) ;
#6361 = CARTESIAN_POINT ( 'NONE',  ( 136.1922820468854241, -10.00000000000000533, -13.59645775552055547 ) ) ;
#6362 = DIRECTION ( 'NONE',  ( -0.9510565162951536422, -2.566386769018988816E-16, -0.3090169943749472292 ) ) ;
#6363 = CARTESIAN_POINT ( 'NONE',  ( 9.661883062008595147, 16.25482663180050835, -17.91564816060341769 ) ) ;
#6364 = CARTESIAN_POINT ( 'NONE',  ( 154.7287565553230024, -1.999999999999974021, -25.16025403784440329 ) ) ;
#6365 = CARTESIAN_POINT ( 'NONE',  ( 142.2287565553230309, -10.00000000000000533, -12.16987298107780369 ) ) ;
#6366 = CARTESIAN_POINT ( 'NONE',  ( 10.33811693838771717, 18.38618951776012267, -17.92015940598198753 ) ) ;
#6367 = ADVANCED_FACE ( 'NONE', ( #9147 ), #18631, .T. ) ;
#6368 = ADVANCED_FACE ( 'NONE', ( #16185 ), #6736, .T. ) ;
#6369 = ORIENTED_EDGE ( 'NONE', *, *, #1080, .T. ) ;
#6370 = LINE ( 'NONE', #12917, #5675 ) ;
#6371 = CARTESIAN_POINT ( 'NONE',  ( 176.1922820468853388, -9.999999999999994671, -30.91696583120936026 ) ) ;
#6372 = EDGE_CURVE ( 'NONE', #9595, #15913, #7039, .T. ) ;
#6373 = CARTESIAN_POINT ( 'NONE',  ( 162.0152310637604955, -9.999999999999998224, -26.04193191628311155 ) ) ;
#6374 = ORIENTED_EDGE ( 'NONE', *, *, #16959, .F. ) ;
#6375 = ORIENTED_EDGE ( 'NONE', *, *, #10559, .F. ) ;
#6376 = CARTESIAN_POINT ( 'NONE',  ( 8.944586743066221146, 16.95158331485313852, -17.91159992548655566 ) ) ;
#6378 = AXIS2_PLACEMENT_3D ( 'NONE', #23617, #16138, #4688 ) ;
#6377 = CARTESIAN_POINT ( 'NONE',  ( 32.03687507811291368, -10.31171301082699543, -18.65038288416666390 ) ) ;
#6379 = CARTESIAN_POINT ( 'NONE',  ( 16.03284225665507279, 2.387151393075086059, -14.54955438622115338 ) ) ;
#6380 = VECTOR ( 'NONE', #18965, 1000.000000000000000 ) ;
#6381 = CARTESIAN_POINT ( 'NONE',  ( 30.76698452600511402, -8.440788201038053273, -16.67119366161266925 ) ) ;
#6382 = CARTESIAN_POINT ( 'NONE',  ( 0.000000000000000000, -1.178949249685215417, 2.042000000000002036 ) ) ;
#6383 = CARTESIAN_POINT ( 'NONE',  ( 134.5152310637605808, -10.00000000000000533, -11.28819510263909187 ) ) ;
#6384 = CARTESIAN_POINT ( 'NONE',  ( 24.07185007603571592, -6.521566527568181115, -20.06683206624251525 ) ) ;
#6385 = COLOUR_RGB ( '', 0.66274510, 0.83137255, 0.94901961) ;
#6386 = EDGE_LOOP ( 'NONE', ( #8265, #17702, #14316, #10337 ) ) ;
#6387 = DIRECTION ( 'NONE',  ( -0.5877852522924731371, -1.586114251531760235E-16, 0.8090169943749474513 ) ) ;
#6389 = ORIENTED_EDGE ( 'NONE', *, *, #3982, .F. ) ;
#6388 = CARTESIAN_POINT ( 'NONE',  ( 152.0152310637604955, -10.00000000000000178, -15.61832212156129351 ) ) ;
#6390 = CARTESIAN_POINT ( 'NONE',  ( 134.7287565553230024, -1.999999999999980460, -25.16025403784439973 ) ) ;
#6391 = DIRECTION ( 'NONE',  ( 0.3090169943749475623, 8.338696094058001131E-17, 0.9510565162951536422 ) ) ;
#6392 = VECTOR ( 'NONE', #24987, 1000.000000000000000 ) ;
#6393 = DIRECTION ( 'NONE',  ( -1.000000000000000000, 0.000000000000000000, 0.000000000000000000 ) ) ;
#6394 = CARTESIAN_POINT ( 'NONE',  ( 33.78268718695997563, -11.09826429569044670, -17.35115476112383348 ) ) ;
#6395 = EDGE_LOOP ( 'NONE', ( #13261, #15694, #18419, #27452 ) ) ;
#6396 = VECTOR ( 'NONE', #6585, 1000.000000000000000 ) ;
#6397 = CARTESIAN_POINT ( 'NONE',  ( 10.66878845912243534, 9.044174962973633214, -16.41115715542894193 ) ) ;
#6398 = EDGE_LOOP ( 'NONE', ( #15075, #22901, #9265, #14465 ) ) ;
#6399 = CARTESIAN_POINT ( 'NONE',  ( 25.97851742199650005, -11.98992670343847244, -16.97112261376066655 ) ) ;
#6400 = FACE_OUTER_BOUND ( 'NONE', #27355, .T. ) ;
#6401 = CARTESIAN_POINT ( 'NONE',  ( 10.35864919664826900, 16.97212497753646687, -17.91558149794984445 ) ) ;
#6402 = DIRECTION ( 'NONE',  ( -2.698458740408365879E-16, 1.000000000000000000, 0.000000000000000000 ) ) ;
#6403 = EDGE_CURVE ( 'NONE', #11673, #25136, #4739, .T. ) ;
#6404 = MECHANICAL_DESIGN_GEOMETRIC_PRESENTATION_REPRESENTATION (  '', ( #24857 ), #24927 ) ;
#6405 = ORIENTED_EDGE ( 'NONE', *, *, #9301, .T. ) ;
#6406 = DIRECTION ( 'NONE',  ( 1.110223024625156540E-16, 2.995891024602366092E-32, 1.000000000000000000 ) ) ;
#6407 = EDGE_CURVE ( 'NONE', #1746, #22518, #29849, .T. ) ;
#6408 = DIRECTION ( 'NONE',  ( 0.000000000000000000, -1.287488025362403787E-15, -1.000000000000000000 ) ) ;
#6409 = FACE_OUTER_BOUND ( 'NONE', #27575, .T. ) ;
#6410 = EDGE_CURVE ( 'NONE', #12130, #8557, #18475, .T. ) ;
#6411 = DIRECTION ( 'NONE',  ( -0.9510565162951536422, -2.566386769018988323E-16, 0.3090169943749475623 ) ) ;
#6412 = ORIENTED_EDGE ( 'NONE', *, *, #9858, .F. ) ;
#6413 = CARTESIAN_POINT ( 'NONE',  ( 15.00903923349565972, 9.404056492746565965, -14.40919036548495669 ) ) ;
#6414 = CARTESIAN_POINT ( 'NONE',  ( 21.76882177598054113, -1.089445278190608102, -19.78435629462099854 ) ) ;
#6415 = CARTESIAN_POINT ( 'NONE',  ( 19.90219557808113038, 2.290409793443704878, -20.93543687874882053 ) ) ;
#6416 = ORIENTED_EDGE ( 'NONE', *, *, #27182, .F. ) ;
#6417 = LINE ( 'NONE', #18147, #21838 ) ;
#6418 = DIRECTION ( 'NONE',  ( 0.3090169943749472292, 8.338696094057992503E-17, -0.9510565162951536422 ) ) ;
#6419 = VECTOR ( 'NONE', #21595, 1000.000000000000000 ) ;
#6420 = AXIS2_PLACEMENT_3D ( 'NONE', #15016, #24345, #3443 ) ;
#6421 = CARTESIAN_POINT ( 'NONE',  ( 18.04049687913209610, 0.8262538513465327306, -14.27019888128743297 ) ) ;
#6422 = EDGE_LOOP ( 'NONE', ( #29806, #28571, #24361, #4126 ) ) ;
#6423 = DIRECTION ( 'NONE',  ( -1.110223024625156540E-16, 0.000000000000000000, -1.000000000000000000 ) ) ;
#6424 = CARTESIAN_POINT ( 'NONE',  ( 158.6922820468853104, -1.999999999999974465, 2.247092850131519715 ) ) ;
#6425 = VERTEX_POINT ( 'NONE', #2022 ) ;
#6426 = LINE ( 'NONE', #24898, #4862 ) ;
#6427 = CARTESIAN_POINT ( 'NONE',  ( 31.62102023406892215, -10.89525581102303420, -15.47516137550896609 ) ) ;
#6428 = DIRECTION ( 'NONE',  ( 2.908569913943825554E-16, -1.000000000000000000, 0.000000000000000000 ) ) ;
#6429 = VERTEX_POINT ( 'NONE', #29991 ) ;
#6430 = CARTESIAN_POINT ( 'NONE',  ( 2.500000000000000444, -1.178949249685215417, 2.042000000000002036 ) ) ;
#6431 = CARTESIAN_POINT ( 'NONE',  ( 14.03850921439652311, 8.975161913830900673, -15.18271992443145635 ) ) ;
#6432 = CARTESIAN_POINT ( 'NONE',  ( 12.24537663854593816, 9.516207477791880365, -15.33311446707169701 ) ) ;
#6433 = CARTESIAN_POINT ( 'NONE',  ( 35.54859390953724585, -22.18451583373416014, -17.99055332684694974 ) ) ;
#6434 = ORIENTED_EDGE ( 'NONE', *, *, #25521, .F. ) ;
#6435 = LINE ( 'NONE', #6280, #19995 ) ;
#6436 = ADVANCED_FACE ( 'NONE', ( #2476 ), #13741, .T. ) ;
#6437 = CARTESIAN_POINT ( 'NONE',  ( 12.75200725638203281, 7.624046516185085665, -14.92932020320056452 ) ) ;
#6438 = DIRECTION ( 'NONE',  ( 0.000000000000000000, -0.000000000000000000, 1.000000000000000000 ) ) ;
#6439 = ADVANCED_FACE ( 'NONE', ( #14183 ), #20753, .T. ) ;
#6440 = EDGE_CURVE ( 'NONE', #6518, #29309, #30141, .T. ) ;
#6441 = ORIENTED_EDGE ( 'NONE', *, *, #12071, .F. ) ;
#6442 = CARTESIAN_POINT ( 'NONE',  ( 132.0152310637605808, -1.999999999999981348, -6.958068083716893781 ) ) ;
#6443 = ADVANCED_FACE ( 'NONE', ( #27830 ), #8855, .T. ) ;
#6444 = ORIENTED_EDGE ( 'NONE', *, *, #14851, .F. ) ;
#6445 = CARTESIAN_POINT ( 'NONE',  ( 10.35864940629342890, 16.97212401607702148, -17.91464645457531191 ) ) ;
#6446 = CARTESIAN_POINT ( 'NONE',  ( 33.54536560287652946, -10.49856191242287373, -18.63199441812703583 ) ) ;
#6447 = CARTESIAN_POINT ( 'NONE',  ( 18.98200677837107264, -2.562081333921657933, -16.63161468174866187 ) ) ;
#6448 = CIRCLE ( 'NONE', #16165, 129.8897274573438381 ) ;
#6449 = DIRECTION ( 'NONE',  ( -2.698458740408365879E-16, 1.000000000000000000, 0.000000000000000000 ) ) ;
#6450 = PLANE ( 'NONE',  #28423 ) ;
#6451 = CARTESIAN_POINT ( 'NONE',  ( 22.24201797625671517, -7.474445146391827777, -15.38054711335415803 ) ) ;
#6452 = CARTESIAN_POINT ( 'NONE',  ( 23.18557557936948044, -8.345241077663208884, -16.42592668061853800 ) ) ;
#6453 = VERTEX_POINT ( 'NONE', #28130 ) ;
#6454 = VECTOR ( 'NONE', #1885, 1000.000000000000000 ) ;
#6455 = ORIENTED_EDGE ( 'NONE', *, *, #19996, .T. ) ;
#6456 = CARTESIAN_POINT ( 'NONE',  ( 164.7287565553229740, -9.999999999999998224, -33.82050807568879947 ) ) ;
#6457 = CARTESIAN_POINT ( 'NONE',  ( 9.641350810849047548, 17.66889113945805789, -23.00000000000000711 ) ) ;
#6458 = DIRECTION ( 'NONE',  ( -1.000000000000000000, -2.908569913943825554E-16, 0.000000000000000000 ) ) ;
#6459 = VECTOR ( 'NONE', #10980, 1000.000000000000000 ) ;
#6460 = DIRECTION ( 'NONE',  ( 0.3090169943749472292, 8.338696094057992503E-17, -0.9510565162951536422 ) ) ;
#6461 = CARTESIAN_POINT ( 'NONE',  ( 11.06190012440529102, 9.834169922982590961, -17.30859480447365328 ) ) ;
#6462 = CARTESIAN_POINT ( 'NONE',  ( 10.33811693838771717, 18.38618951776012267, -17.97192418671890835 ) ) ;
#6463 = CARTESIAN_POINT ( 'NONE',  ( 28.40444427461093113, -11.06999723682266179, -18.98653349803348078 ) ) ;
#6464 = ORIENTED_EDGE ( 'NONE', *, *, #13008, .T. ) ;
#6465 = CARTESIAN_POINT ( 'NONE',  ( 130.7287565553229172, -4.999999999999983125, -28.21440484423857242 ) ) ;
#6466 = EDGE_LOOP ( 'NONE', ( #26352, #21118, #5879, #6910, #26741 ) ) ;
#6467 = CARTESIAN_POINT ( 'NONE',  ( 9.644802874473198173, 17.65305953564175567, -17.69767226479352118 ) ) ;
#6468 = EDGE_CURVE ( 'NONE', #26900, #10926, #1875, .T. ) ;
#6470 = FACE_OUTER_BOUND ( 'NONE', #1254, .T. ) ;
#6469 = AXIS2_PLACEMENT_3D ( 'NONE', #17359, #12631, #898 ) ;
#6471 = CARTESIAN_POINT ( 'NONE',  ( 15.60359850163179551, 6.442352727238609411, -18.97839103356167101 ) ) ;
#6472 = CARTESIAN_POINT ( 'NONE',  ( -4.000000000000003553, -6.938893903907228378E-15, -2.450000000000000178 ) ) ;
#6473 = CARTESIAN_POINT ( 'NONE',  ( 26.10647222977721071, -5.000000000000010658, -80.34745979530829629 ) ) ;
#6474 = EDGE_CURVE ( 'NONE', #7790, #25049, #20907, .T. ) ;
#6476 = EDGE_LOOP ( 'NONE', ( #7891, #624, #7449, #1224 ) ) ;
#6475 = CARTESIAN_POINT ( 'NONE',  ( 23.29338531092689735, -7.078548041224526521, -17.51562821661096336 ) ) ;
#6477 = VERTEX_POINT ( 'NONE', #15874 ) ;
#6478 = LINE ( 'NONE', #20643, #23726 ) ;
#6479 = EDGE_CURVE ( 'NONE', #17865, #7141, #9307, .T. ) ;
#6480 = CARTESIAN_POINT ( 'NONE',  ( 12.25874535991881764, 9.522117202545773651, -15.32245921924925902 ) ) ;
#6481 = CARTESIAN_POINT ( 'NONE',  ( 33.47012763672258728, -12.84706786418751534, -19.72967806864707541 ) ) ;
#6482 = LINE ( 'NONE', #4336, #6903 ) ;
#6483 = CARTESIAN_POINT ( 'NONE',  ( 26.72181814967143509, -3.137724904577397389, -15.69709663067708050 ) ) ;
#6484 = DIRECTION ( 'NONE',  ( 1.000000000000000000, 0.000000000000000000, 0.000000000000000000 ) ) ;
#6485 = CARTESIAN_POINT ( 'NONE',  ( 24.85091453934022709, -2.360935040140837771, -14.69038261433388293 ) ) ;
#6486 = ORIENTED_EDGE ( 'NONE', *, *, #8617, .F. ) ;
#6487 = DIRECTION ( 'NONE',  ( -0.9510565162951536422, -2.566386769018988816E-16, -0.3090169943749472292 ) ) ;
#6488 = CARTESIAN_POINT ( 'NONE',  ( 16.94700227795405212, 10.49100606271714931, -14.51747230701220559 ) ) ;
#6489 = CARTESIAN_POINT ( 'NONE',  ( 27.29378187812181267, -6.326311925282933402, -12.73600023524891967 ) ) ;
#6490 = ORIENTED_EDGE ( 'NONE', *, *, #10410, .F. ) ;
#6491 = VERTEX_POINT ( 'NONE', #19943 ) ;
#6492 = CARTESIAN_POINT ( 'NONE',  ( 166.1922820468853672, -9.999999999999998224, -22.25671179336496053 ) ) ;
#6493 = VECTOR ( 'NONE', #29490, 1000.000000000000000 ) ;
#6494 = FACE_OUTER_BOUND ( 'NONE', #7878, .T. ) ;
#6495 = VERTEX_POINT ( 'NONE', #8185 ) ;
#6496 = EDGE_CURVE ( 'NONE', #10227, #10342, #24381, .T. ) ;
#6497 = CARTESIAN_POINT ( 'NONE',  ( 157.0152310637604955, -1.999999999999974465, -6.958068083716895558 ) ) ;
#6498 = LINE ( 'NONE', #15939, #9156 ) ;
#6499 = DIRECTION ( 'NONE',  ( 0.9510565162951536422, 2.566386769018988816E-16, 0.3090169943749472292 ) ) ;
#6500 = CARTESIAN_POINT ( 'NONE',  ( 149.5152310637604955, -10.00000000000000178, -4.391296821672111328 ) ) ;
#6501 = CARTESIAN_POINT ( 'NONE',  ( 23.72538513773186608, -9.146839435613468794, -15.72061189943629600 ) ) ;
#6502 = CARTESIAN_POINT ( 'NONE',  ( 16.03657434348277633, 2.746931742562784162, -16.83325620853174698 ) ) ;
#6503 = CARTESIAN_POINT ( 'NONE',  ( 36.19022241692326247, -21.57454255207833071, -21.10101832753974449 ) ) ;
#6504 = CARTESIAN_POINT ( 'NONE',  ( 154.5152310637605808, -1.999999999999974021, -28.60870317832789667 ) ) ;
#6505 = CARTESIAN_POINT ( 'NONE',  ( 11.47079713067724782, 9.278817116560638567, -15.86177209170659275 ) ) ;
#6506 = CARTESIAN_POINT ( 'NONE',  ( 15.93055805288878801, -5.000000000000013323, 49.02921625739047329 ) ) ;
#6507 = CARTESIAN_POINT ( 'NONE',  ( 132.0152310637605524, -10.00000000000000711, -0.06116980274991495881 ) ) ;
#6508 = CARTESIAN_POINT ( 'NONE',  ( 9.748920381043669536, 15.85566239202790406, -17.85155811514292878 ) ) ;
#6510 = ORIENTED_EDGE ( 'NONE', *, *, #5320, .F. ) ;
#6509 = CARTESIAN_POINT ( 'NONE',  ( -1.313474075707254052, -8.479269695850879529, -4.683279549040147316 ) ) ;
#6511 = ORIENTED_EDGE ( 'NONE', *, *, #29568, .F. ) ;
#6512 = DIRECTION ( 'NONE',  ( 0.9510565162951536422, 2.566386769018988816E-16, 0.3090169943749472292 ) ) ;
#6513 = EDGE_CURVE ( 'NONE', #3997, #486, #2620, .T. ) ;
#6514 = CARTESIAN_POINT ( 'NONE',  ( 13.04501788334644630, 8.811555337407297017, -14.69578613943112799 ) ) ;
#6515 = ORIENTED_EDGE ( 'NONE', *, *, #10062, .T. ) ;
#6516 = CARTESIAN_POINT ( 'NONE',  ( 159.5152310637604955, -1.999999999999973577, -11.28819510263909542 ) ) ;
#6517 = LINE ( 'NONE', #15807, #22976 ) ;
#6518 = VERTEX_POINT ( 'NONE', #884 ) ;
#6519 = PLANE ( 'NONE',  #24895 ) ;
#6520 = VECTOR ( 'NONE', #28347, 1000.000000000000000 ) ;
#6521 = ORIENTED_EDGE ( 'NONE', *, *, #2826, .T. ) ;
#6522 = CARTESIAN_POINT ( 'NONE',  ( 13.44731269622883296, 7.655871835264917102, -15.65391398210326201 ) ) ;
#6523 = CARTESIAN_POINT ( 'NONE',  ( 34.81339731023632567, -19.88166695754494384, -21.17803781427711840 ) ) ;
#6524 = CARTESIAN_POINT ( 'NONE',  ( 17.99875044999096119, -0.3805832805143671838, -17.40611996466761369 ) ) ;
#6525 = CARTESIAN_POINT ( 'NONE',  ( 15.11341857612343809, 8.679638894638937785, -13.66094189273949056 ) ) ;
#6526 = CARTESIAN_POINT ( 'NONE',  ( 137.2287565553230309, -10.00000000000000533, -29.49038105676660138 ) ) ;
#6527 = CARTESIAN_POINT ( 'NONE',  ( 24.79321154704742725, 0.1008434151899674086, -19.04223803188042652 ) ) ;
#6528 = VERTEX_POINT ( 'NONE', #29147 ) ;
#6529 = DIRECTION ( 'NONE',  ( -0.5877852522924731371, 0.000000000000000000, 0.8090169943749474513 ) ) ;
#6530 = EDGE_CURVE ( 'NONE', #4371, #12000, #10470, .T. ) ;
#6532 = VERTEX_POINT ( 'NONE', #22233 ) ;
#6531 = LINE ( 'NONE', #4390, #7763 ) ;
#6533 = DIRECTION ( 'NONE',  ( 0.9510565162951536422, 2.566386769018988816E-16, 0.3090169943749472292 ) ) ;
#6534 = DIRECTION ( 'NONE',  ( -0.5877852522924731371, -1.586114251531760235E-16, 0.8090169943749474513 ) ) ;
#6535 = AXIS2_PLACEMENT_3D ( 'NONE', #29412, #8433, #10418 ) ;
#6536 = ORIENTED_EDGE ( 'NONE', *, *, #4198, .T. ) ;
#6537 = DIRECTION ( 'NONE',  ( 0.5877852522924731371, 1.586114251531760728E-16, 0.8090169943749474513 ) ) ;
#6538 = CARTESIAN_POINT ( 'NONE',  ( 34.04598001273328833, -11.17175086900407166, -18.07582794505754364 ) ) ;
#6539 = VERTEX_POINT ( 'NONE', #17054 ) ;
#6540 = CARTESIAN_POINT ( 'NONE',  ( 11.89457502915311160, 7.563359933683480918, -15.58843798323820096 ) ) ;
#6541 = ORIENTED_EDGE ( 'NONE', *, *, #27650, .T. ) ;
#6542 = CARTESIAN_POINT ( 'NONE',  ( 27.11191462667604313, -11.78482644060662743, -13.28705938033944989 ) ) ;
#6543 = CARTESIAN_POINT ( 'NONE',  ( 162.0152310637605240, -1.999999999999972244, -24.27857615940569502 ) ) ;
#6544 = CARTESIAN_POINT ( 'NONE',  ( 11.50940939395034768, 11.69459202490242689, -16.90580767540677343 ) ) ;
#6545 = CARTESIAN_POINT ( 'NONE',  ( 172.7287565553229456, -9.999999999999971578, 3.500000000000003109 ) ) ;
#6546 = EDGE_LOOP ( 'NONE', ( #11198, #11163, #24453, #18438 ) ) ;
#6547 = ORIENTED_EDGE ( 'NONE', *, *, #29831, .F. ) ;
#6548 = CARTESIAN_POINT ( 'NONE',  ( 156.1922820468853388, -10.00000000000000178, -4.936203717676158398 ) ) ;
#6549 = CARTESIAN_POINT ( 'NONE',  ( 139.5152310637605524, -1.999999999999979128, -4.391296821672111328 ) ) ;
#6551 = ORIENTED_EDGE ( 'NONE', *, *, #17179, .T. ) ;
#6550 = LINE ( 'NONE', #17683, #13533 ) ;
#6552 = DIRECTION ( 'NONE',  ( -0.9510565162951536422, -2.566386769018988816E-16, -0.3090169943749472292 ) ) ;
#6553 = VERTEX_POINT ( 'NONE', #21784 ) ;
#6554 = CARTESIAN_POINT ( 'NONE',  ( 13.12553198385420927, 8.571700941790735939, -15.91037888968202552 ) ) ;
#6555 = VERTEX_POINT ( 'NONE', #19488 ) ;
#6556 = CARTESIAN_POINT ( 'NONE',  ( 20.42254326673722531, -2.835881520377886655, -15.10989100197473789 ) ) ;
#6557 = CARTESIAN_POINT ( 'NONE',  ( 19.88518670226333995, -2.923732859705698850, -17.09422515135678111 ) ) ;
#6558 = VERTEX_POINT ( 'NONE', #10172 ) ;
#6559 = CARTESIAN_POINT ( 'NONE',  ( 18.23802153489769751, 0.9697156596711644649, -18.35043786425562828 ) ) ;
#6560 = CARTESIAN_POINT ( 'NONE',  ( 136.1922820468854241, -1.999999999999980460, -10.74328820663507322 ) ) ;
#6561 = VECTOR ( 'NONE', #6045, 1000.000000000000000 ) ;
#6562 = ADVANCED_BREP_SHAPE_REPRESENTATION ( '', ( #11686, #13190 ), #1965 ) ;
#6563 = CARTESIAN_POINT ( 'NONE',  ( 163.6922820468853388, -1.999999999999972689, -17.92658477444275889 ) ) ;
#6564 = CARTESIAN_POINT ( 'NONE',  ( 17.96884874826282186, 1.586046385177752871, -19.67104016136476119 ) ) ;
#6565 = ORIENTED_EDGE ( 'NONE', *, *, #24880, .T. ) ;
#6566 = DIRECTION ( 'NONE',  ( -0.000000000000000000, -0.000000000000000000, -1.000000000000000000 ) ) ;
#6567 = EDGE_CURVE ( 'NONE', #5949, #13402, #19333, .T. ) ;
#6568 = DIRECTION ( 'NONE',  ( 0.5877852522924731371, 1.586114251531760728E-16, 0.8090169943749474513 ) ) ;
#6569 = EDGE_CURVE ( 'NONE', #23922, #4780, #9168, .T. ) ;
#6570 = ADVANCED_FACE ( 'NONE', ( #24085 ), #3186, .T. ) ;
#6571 = EDGE_CURVE ( 'NONE', #24722, #28182, #17202, .T. ) ;
#6572 = EDGE_LOOP ( 'NONE', ( #8098, #6114, #7686, #28054 ) ) ;
#6573 = DIRECTION ( 'NONE',  ( -1.000000000000000000, 0.000000000000000000, 0.000000000000000000 ) ) ;
#6574 = CARTESIAN_POINT ( 'NONE',  ( -20.00000000000017053, 34.64101615137744972, 0.000000000000000000 ) ) ;
#6575 = LINE ( 'NONE', #25192, #25334 ) ;
#6576 = ORIENTED_EDGE ( 'NONE', *, *, #13069, .T. ) ;
#6577 = ORIENTED_EDGE ( 'NONE', *, *, #27289, .T. ) ;
#6578 = CARTESIAN_POINT ( 'NONE',  ( 164.7287565553229172, -1.999999999999971800, -16.50000000000000355 ) ) ;
#6579 = CARTESIAN_POINT ( 'NONE',  ( 17.66155849027303049, 7.702290371990539342, -14.74052880078125760 ) ) ;
#6580 = CARTESIAN_POINT ( 'NONE',  ( 11.05541531668977662, 17.68942339022145305, -17.94384837343789130 ) ) ;
#6581 = CARTESIAN_POINT ( 'NONE',  ( 35.54859390953724585, -22.18451583373416014, -18.06010107863414405 ) ) ;
#6582 = VERTEX_POINT ( 'NONE', #7893 ) ;
#6583 = CARTESIAN_POINT ( 'NONE',  ( 171.1922820468853672, -1.999999999999970024, -30.91696583120936026 ) ) ;
#6584 = CARTESIAN_POINT ( 'NONE',  ( 12.76959483864652611, 7.631811206235384226, -14.91530316759754982 ) ) ;
#6585 = DIRECTION ( 'NONE',  ( -1.110223024625156540E-16, 0.000000000000000000, -1.000000000000000000 ) ) ;
#6586 = CARTESIAN_POINT ( 'NONE',  ( 0.000000000000000000, 0.000000000000000000, -5.000000000000000888 ) ) ;
#6587 = ORIENTED_EDGE ( 'NONE', *, *, #22792, .F. ) ;
#6588 = PLANE ( 'NONE',  #21268 ) ;
#6589 = ORIENTED_EDGE ( 'NONE', *, *, #30190, .T. ) ;
#6590 = CARTESIAN_POINT ( 'NONE',  ( 12.86833691348896203, 9.516071730297785081, -16.11536789055087837 ) ) ;
#6591 = CARTESIAN_POINT ( 'NONE',  ( 36.54859390953724585, -21.18451583373416014, -17.64281456791166391 ) ) ;
#6592 = CARTESIAN_POINT ( 'NONE',  ( 21.18945582756405344, -5.194394521544061227, -16.21196392551894405 ) ) ;
#6593 = CARTESIAN_POINT ( 'NONE',  ( 137.0152310637605808, -4.999999999999980460, -1.521174642513229767E-14 ) ) ;
#6594 = CARTESIAN_POINT ( 'NONE',  ( 130.7287565553229456, -4.999999999999983125, 3.500000000000003109 ) ) ;
#6595 = SURFACE_STYLE_FILL_AREA ( #2037 ) ;
#6596 = CARTESIAN_POINT ( 'NONE',  ( 24.19195398915606532, -10.47609993289601427, -15.85356615136800151 ) ) ;
#6597 = CARTESIAN_POINT ( 'NONE',  ( 27.85231147893869874, -3.451530096863186792, -17.11803778117090857 ) ) ;
#6598 = VECTOR ( 'NONE', #26753, 1000.000000000000000 ) ;
#6599 = ORIENTED_EDGE ( 'NONE', *, *, #3403, .T. ) ;
#6600 = LINE ( 'NONE', #4163, #29443 ) ;
#6601 = EDGE_CURVE ( 'NONE', #29946, #5949, #5612, .T. ) ;
#6602 = EDGE_CURVE ( 'NONE', #14986, #26056, #21480, .T. ) ;
#6603 = EDGE_CURVE ( 'NONE', #27886, #15011, #17344, .T. ) ;
#6604 = VECTOR ( 'NONE', #8778, 1000.000000000000000 ) ;
#6605 = DIRECTION ( 'NONE',  ( -2.698458740408365879E-16, 1.000000000000000000, 0.000000000000000000 ) ) ;
#6606 = DIRECTION ( 'NONE',  ( 0.9510565162951536422, 2.566386769018988816E-16, 0.3090169943749472292 ) ) ;
#6607 = CARTESIAN_POINT ( 'NONE',  ( 8.000000000000014211, 1.572549600175628060, -0.06894455525514016359 ) ) ;
#6608 = CARTESIAN_POINT ( 'NONE',  ( 12.52778158092594474, 8.582979361647906202, -15.10803260229456946 ) ) ;
#6609 = DIRECTION ( 'NONE',  ( -2.698458740408365879E-16, 1.000000000000000000, 0.000000000000000000 ) ) ;
#6610 = LINE ( 'NONE', #18198, #8612 ) ;
#6611 = ORIENTED_EDGE ( 'NONE', *, *, #28665, .T. ) ;
#6612 = VECTOR ( 'NONE', #13067, 1000.000000000000000 ) ;
#6613 = CARTESIAN_POINT ( 'NONE',  ( 9.641350829061996919, 17.66889105593114806, -17.91548090047172437 ) ) ;
#6614 = CONICAL_SURFACE ( 'NONE', #25628, 5.000000000000000888, 0.2131563744996338439 ) ;
#6615 = CARTESIAN_POINT ( 'NONE',  ( 28.93285792728966044, -11.80516759558957673, -13.86517224201260134 ) ) ;
#6616 = CARTESIAN_POINT ( 'NONE',  ( 129.5152310637605524, -1.999999999999982236, -13.05155085951650840 ) ) ;
#6617 = DIRECTION ( 'NONE',  ( 0.5877852522924731371, 1.586114251531760728E-16, 0.8090169943749474513 ) ) ;
#6618 = ORIENTED_EDGE ( 'NONE', *, *, #23106, .F. ) ;
#6620 = ORIENTED_EDGE ( 'NONE', *, *, #27483, .F. ) ;
#6619 = CARTESIAN_POINT ( 'NONE',  ( 21.79935899731381710, -1.430375723040585356, -13.25318265510616733 ) ) ;
#6621 = ORIENTED_EDGE ( 'NONE', *, *, #23772, .T. ) ;
#6622 = CARTESIAN_POINT ( 'NONE',  ( 132.0152310637605524, -10.00000000000000711, -34.70218595412750773 ) ) ;
#6623 = CARTESIAN_POINT ( 'NONE',  ( 12.27916258238306746, 9.531139938431367753, -15.30618633255685879 ) ) ;
#6624 = VERTEX_POINT ( 'NONE', #28999 ) ;
#6625 = CARTESIAN_POINT ( 'NONE',  ( 35.13870703111577143, -20.34311121210408757, -20.23074448643712486 ) ) ;
#6626 = DIRECTION ( 'NONE',  ( -0.8090169943749474513, -2.183098979609982436E-16, 0.5877852522924731371 ) ) ;
#6627 = CARTESIAN_POINT ( 'NONE',  ( 22.34083945069921739, -4.755659482961629436, -14.12236044035638116 ) ) ;
#6628 = DIRECTION ( 'NONE',  ( 1.000000000000000000, 0.000000000000000000, 0.000000000000000000 ) ) ;
#6629 = CARTESIAN_POINT ( 'NONE',  ( 25.80045869113294543, -2.244538201703065283, -16.37342509101419807 ) ) ;
#6630 = ORIENTED_EDGE ( 'NONE', *, *, #10380, .T. ) ;
#6631 = CARTESIAN_POINT ( 'NONE',  ( 164.5152310637605240, -9.999999999999996447, -28.60870317832789667 ) ) ;
#6632 = CARTESIAN_POINT ( 'NONE',  ( 27.15828739042733631, -11.95405637977086677, -19.54710185400437794 ) ) ;
#6633 = CARTESIAN_POINT ( 'NONE',  ( 30.81871029749655477, -11.10956723898439868, -14.94490981684777431 ) ) ;
#6634 = VECTOR ( 'NONE', #20235, 1000.000000000000000 ) ;
#6635 = VERTEX_POINT ( 'NONE', #3334 ) ;
#6636 = ORIENTED_EDGE ( 'NONE', *, *, #11341, .F. ) ;
#6637 = CARTESIAN_POINT ( 'NONE',  ( 154.5152310637605524, -4.999999999999976019, -1.715463671822631846E-14 ) ) ;
#6638 = CIRCLE ( 'NONE', #11497, 8.000000000000000000 ) ;
#6639 = EDGE_CURVE ( 'NONE', #22085, #4384, #26689, .T. ) ;
#6640 = EDGE_CURVE ( 'NONE', #6979, #26011, #3476, .T. ) ;
#6641 = VECTOR ( 'NONE', #15152, 1000.000000000000000 ) ;
#6642 = EDGE_CURVE ( 'NONE', #26171, #23545, #19780, .T. ) ;
#6643 = DIRECTION ( 'NONE',  ( 0.3090169943749475623, 8.338696094058001131E-17, 0.9510565162951536422 ) ) ;
#6644 = EDGE_CURVE ( 'NONE', #29341, #25494, #20021, .T. ) ;
#6645 = DIRECTION ( 'NONE',  ( -0.5877852522924731371, -1.586114251531760235E-16, 0.8090169943749474513 ) ) ;
#6646 = LINE ( 'NONE', #8619, #17443 ) ;
#6647 = FACE_OUTER_BOUND ( 'NONE', #15415, .T. ) ;
#6648 = LINE ( 'NONE', #27741, #914 ) ;
#6649 = CARTESIAN_POINT ( 'NONE',  ( 27.00045552667489446, -4.635344809676953837, -19.07524480842047510 ) ) ;
#6650 = CARTESIAN_POINT ( 'NONE',  ( 13.86827785273622737, 5.312354197023893221, -16.63408457058017120 ) ) ;
#6652 = VERTEX_POINT ( 'NONE', #15200 ) ;
#6651 = CARTESIAN_POINT ( 'NONE',  ( 32.85377328814971065, -9.687349299063408026, -18.71178847241494481 ) ) ;
#6653 = CARTESIAN_POINT ( 'NONE',  ( 0.000000000000000000, 0.000000000000000000, 15.00000000000000000 ) ) ;
#6654 = CARTESIAN_POINT ( 'NONE',  ( 11.47327446659168615, 9.267463859335506982, -15.86074700677745852 ) ) ;
#6655 = CIRCLE ( 'NONE', #9552, 0.5000000000000004441 ) ;
#6656 = DIRECTION ( 'NONE',  ( 0.3090169943749475623, 8.338696094058001131E-17, 0.9510565162951536422 ) ) ;
#6657 = DIRECTION ( 'NONE',  ( -0.9510565162951536422, -2.566386769018988816E-16, -0.3090169943749472292 ) ) ;
#6658 = CARTESIAN_POINT ( 'NONE',  ( 9.667904883771802460, 16.22720978959070592, -17.88506087084571305 ) ) ;
#6659 = PLANE ( 'NONE',  #8277 ) ;
#6660 = ORIENTED_EDGE ( 'NONE', *, *, #815, .T. ) ;
#6661 = CARTESIAN_POINT ( 'NONE',  ( 177.2287565553229172, -9.999999999999994671, -29.49038105676660493 ) ) ;
#6662 = CARTESIAN_POINT ( 'NONE',  ( 12.13006862794127017, 8.527244997094612700, -15.41586291625151972 ) ) ;
#6663 = EDGE_LOOP ( 'NONE', ( #29489, #16083, #23607, #19984 ) ) ;
#6664 = VECTOR ( 'NONE', #4629, 1000.000000000000000 ) ;
#6665 = DIRECTION ( 'NONE',  ( -1.110223024625156540E-16, 0.000000000000000000, -1.000000000000000000 ) ) ;
#6666 = CARTESIAN_POINT ( 'NONE',  ( 133.7287565553229172, -4.000000000000003553, -41.50000000000000000 ) ) ;
#6667 = EDGE_LOOP ( 'NONE', ( #17570, #16992, #19207, #1374, #331, #27010 ) ) ;
#6668 = AXIS2_PLACEMENT_3D ( 'NONE', #10878, #27268, #22646 ) ;
#6669 = CARTESIAN_POINT ( 'NONE',  ( 172.7287565553229456, -9.999999999999980460, -41.50000000000000711 ) ) ;
#6670 = ORIENTED_EDGE ( 'NONE', *, *, #26054, .F. ) ;
#6671 = ORIENTED_EDGE ( 'NONE', *, *, #3644, .F. ) ;
#6672 = CARTESIAN_POINT ( 'NONE',  ( 9.106918858820071350, 16.20710753947419747, -17.05743340929950946 ) ) ;
#6673 = CARTESIAN_POINT ( 'NONE',  ( 35.52699606538937616, -23.08748816067360465, -19.11185354855568619 ) ) ;
#6674 = CARTESIAN_POINT ( 'NONE',  ( 19.69411524970139737, 8.437195840132273972, -14.56566581881308409 ) ) ;
#6675 = CARTESIAN_POINT ( 'NONE',  ( 19.85258860919307367, 6.732389232436280402, -16.96582824858274208 ) ) ;
#6676 = CARTESIAN_POINT ( 'NONE',  ( 163.6922820468853956, -4.999999999999973355, -32.39392330124607611 ) ) ;
#6677 = CARTESIAN_POINT ( 'NONE',  ( 27.84123584509972815, -2.508445798277625371, -17.45642919975013285 ) ) ;
#6678 = EDGE_CURVE ( 'NONE', #7514, #9503, #6876, .T. ) ;
#6679 = AXIS2_PLACEMENT_3D ( 'NONE', #30039, #11054, #2070 ) ;
#6680 = VERTEX_POINT ( 'NONE', #10019 ) ;
#6681 = ADVANCED_FACE ( 'NONE', ( #27154 ), #20682, .T. ) ;
#6682 = PLANE ( 'NONE',  #29452 ) ;
#6683 = EDGE_CURVE ( 'NONE', #22665, #25015, #10928, .T. ) ;
#6685 = ORIENTED_EDGE ( 'NONE', *, *, #19856, .T. ) ;
#6684 = DIRECTION ( 'NONE',  ( -0.06678507476159963041, 0.9947851038922184141, -0.07708664516786083165 ) ) ;
#6686 = VECTOR ( 'NONE', #6411, 999.9999999999998863 ) ;
#6687 = VERTEX_POINT ( 'NONE', #24688 ) ;
#6689 = CARTESIAN_POINT ( 'NONE',  ( 169.5152310637604387, -1.999999999999971356, -2.627941064794695691 ) ) ;
#6688 = VECTOR ( 'NONE', #14663, 1000.000000000000000 ) ;
#6690 = CARTESIAN_POINT ( 'NONE',  ( 131.1922820468854241, -4.999999999999982236, -28.06379628232387446 ) ) ;
#6691 = ORIENTED_EDGE ( 'NONE', *, *, #7497, .F. ) ;
#6692 = CARTESIAN_POINT ( 'NONE',  ( 34.98004922032874475, -18.63034571161586683, -19.14376959241974774 ) ) ;
#6693 = VECTOR ( 'NONE', #1285, 1000.000000000000000 ) ;
#6694 = CARTESIAN_POINT ( 'NONE',  ( 12.54775956925048774, 7.553149829897631840, -15.09063234640338003 ) ) ;
#6695 = EDGE_LOOP ( 'NONE', ( #15231, #3066, #5326, #4700 ) ) ;
#6696 = CARTESIAN_POINT ( 'NONE',  ( 29.46565128511723586, -7.689737916804423534, -14.82739468409561567 ) ) ;
#6697 = DIRECTION ( 'NONE',  ( -1.000000000000000000, 0.000000000000000000, 0.000000000000000000 ) ) ;
#6698 = CARTESIAN_POINT ( 'NONE',  ( 10.46436961932593945, 16.48727764291732711, -17.33901581970886241 ) ) ;
#6699 = CARTESIAN_POINT ( 'NONE',  ( 92.15659011758447150, -4.999999999999992006, 66.95568195638367115 ) ) ;
#6700 = DIRECTION ( 'NONE',  ( 1.000000000000000000, 2.698458740408365879E-16, -1.110223024625156540E-16 ) ) ;
#6701 = ORIENTED_EDGE ( 'NONE', *, *, #23422, .T. ) ;
#6702 = CARTESIAN_POINT ( 'NONE',  ( 136.1922820468854241, -10.00000000000000533, -4.936203717676158398 ) ) ;
#6703 = VECTOR ( 'NONE', #29069, 1000.000000000000000 ) ;
#6704 = CARTESIAN_POINT ( 'NONE',  ( -13.00000000000000178, -2.870178842070716726E-15, -23.00000000000000000 ) ) ;
#6705 = EDGE_LOOP ( 'NONE', ( #24685, #11756, #9320, #13185 ) ) ;
#6706 = ORIENTED_EDGE ( 'NONE', *, *, #3749, .T. ) ;
#6707 = DIRECTION ( 'NONE',  ( -2.698458740408365879E-16, 1.000000000000000000, 0.000000000000000000 ) ) ;
#6708 = ORIENTED_EDGE ( 'NONE', *, *, #6954, .F. ) ;
#6709 = CARTESIAN_POINT ( 'NONE',  ( 10.70528834225764392, 11.46963701334067842, -17.45606632095149280 ) ) ;
#6710 = EDGE_CURVE ( 'NONE', #21232, #25023, #3929, .T. ) ;
#6711 = VECTOR ( 'NONE', #26813, 1000.000000000000000 ) ;
#6712 = CARTESIAN_POINT ( 'NONE',  ( 23.66883837772530441, 2.046813550970532969, -14.77838854720118000 ) ) ;
#6713 = CARTESIAN_POINT ( 'NONE',  ( 23.59026362060683724, -1.443753810951279082, -14.18444229111703514 ) ) ;
#6714 = CARTESIAN_POINT ( 'NONE',  ( 20.13607245741800611, 4.456688099076253629, -14.49627829575511129 ) ) ;
#6715 = DIRECTION ( 'NONE',  ( -2.698458740408365879E-16, 1.000000000000000000, 0.000000000000000000 ) ) ;
#6716 = CARTESIAN_POINT ( 'NONE',  ( 169.7287565553229740, -9.999999999999996447, -33.82050807568879947 ) ) ;
#6717 = CARTESIAN_POINT ( 'NONE',  ( 25.31619048431776875, -0.2099727537683927225, -15.56338435260822628 ) ) ;
#6718 = VERTEX_POINT ( 'NONE', #11086 ) ;
#6719 = CARTESIAN_POINT ( 'NONE',  ( 171.1922820468853672, -4.999999999999971578, -30.91696583120936026 ) ) ;
#6720 = CARTESIAN_POINT ( 'NONE',  ( 169.5152310637604387, -1.999999999999970912, -13.05155085951651195 ) ) ;
#6721 = VECTOR ( 'NONE', #10362, 1000.000000000000000 ) ;
#6722 = DIRECTION ( 'NONE',  ( -1.000000000000000000, -4.440892098500622217E-16, 0.000000000000000000 ) ) ;
#6723 = CARTESIAN_POINT ( 'NONE',  ( 35.49237112349044310, -21.93193663806729887, -19.32748734164077931 ) ) ;
#6724 = LINE ( 'NONE', #2307, #23382 ) ;
#6725 = AXIS2_PLACEMENT_3D ( 'NONE', #19230, #2630, #23369 ) ;
#6726 = VERTEX_POINT ( 'NONE', #13674 ) ;
#6727 = ORIENTED_EDGE ( 'NONE', *, *, #4737, .F. ) ;
#6728 = DIRECTION ( 'NONE',  ( -0.000000000000000000, -0.000000000000000000, -1.000000000000000000 ) ) ;
#6729 = CARTESIAN_POINT ( 'NONE',  ( 14.39533340154967433, 6.572929804808670617, -18.54476805420031837 ) ) ;
#6730 = CARTESIAN_POINT ( 'NONE',  ( 11.92449941057312124, 13.70369295321711256, -16.51642704783386506 ) ) ;
#6731 = CARTESIAN_POINT ( 'NONE',  ( 35.49237112349044310, -21.93193663806729887, -19.32748734164077931 ) ) ;
#6732 = ORIENTED_EDGE ( 'NONE', *, *, #11958, .F. ) ;
#6733 = VERTEX_POINT ( 'NONE', #6666 ) ;
#6734 = CARTESIAN_POINT ( 'NONE',  ( 9.641350810849047548, 17.66889113945805789, -17.92454625180715766 ) ) ;
#6735 = CARTESIAN_POINT ( 'NONE',  ( 9.641350835837977584, 17.66889102485563612, -17.91507476468484938 ) ) ;
#6736 = PLANE ( 'NONE',  #17105 ) ;
#6737 =( NAMED_UNIT ( * ) SI_UNIT ( $, .STERADIAN. ) SOLID_ANGLE_UNIT ( ) );
#6738 = ORIENTED_EDGE ( 'NONE', *, *, #15367, .T. ) ;
#6739 = DIRECTION ( 'NONE',  ( -0.000000000000000000, 1.000000000000000000, 0.000000000000000000 ) ) ;
#6740 = ORIENTED_EDGE ( 'NONE', *, *, #25658, .F. ) ;
#6741 = CARTESIAN_POINT ( 'NONE',  ( 17.21732962576914616, 11.43796928512929867, -12.64914394394206454 ) ) ;
#6742 = EDGE_CURVE ( 'NONE', #9720, #981, #20386, .T. ) ;
#6743 = CARTESIAN_POINT ( 'NONE',  ( 33.28625081342995884, -10.37305140221732991, -17.94975064729133862 ) ) ;
#6744 = CARTESIAN_POINT ( 'NONE',  ( 24.43075134246613800, -6.859861339260811874, -14.00379227226492951 ) ) ;
#6745 = EDGE_LOOP ( 'NONE', ( #7962, #14115 ) ) ;
#6746 = EDGE_CURVE ( 'NONE', #22297, #7033, #24840, .T. ) ;
#6747 = VECTOR ( 'NONE', #24822, 1000.000000000000000 ) ;
#6748 = CARTESIAN_POINT ( 'NONE',  ( 133.6922820468854241, -10.00000000000000711, 2.247092850131519715 ) ) ;
#6749 = DIRECTION ( 'NONE',  ( 0.3090169943749472292, 8.338696094057992503E-17, -0.9510565162951536422 ) ) ;
#6750 = PRODUCT_CONTEXT ( 'NONE', #27655, 'mechanical' ) ;
#6751 = CARTESIAN_POINT ( 'NONE',  ( 15.92010713857317938, 6.231155140105813395, -20.15531274222559333 ) ) ;
#6752 = VECTOR ( 'NONE', #14000, 1000.000000000000000 ) ;
#6753 = CARTESIAN_POINT ( 'NONE',  ( 20.36141319467227362, -5.793038086071195636, -16.11598603859005507 ) ) ;
#6754 = ORIENTED_EDGE ( 'NONE', *, *, #23993, .T. ) ;
#6755 = CARTESIAN_POINT ( 'NONE',  ( 20.21908482906315996, -5.000000000000012434, -62.22794451515765957 ) ) ;
#6756 = CARTESIAN_POINT ( 'NONE',  ( 2.500000000000000444, 0.000000000000000000, 0.000000000000000000 ) ) ;
#6757 = CARTESIAN_POINT ( 'NONE',  ( 169.5152310637604671, -1.999999999999970912, -11.28819510263909542 ) ) ;
#6758 = CARTESIAN_POINT ( 'NONE',  ( -31.74999999999995737, 3.061616997868384127E-16, -2.500000000000000888 ) ) ;
#6759 = APPLICATION_CONTEXT ( 'automotive_design' ) ;
#6760 = UNCERTAINTY_MEASURE_WITH_UNIT (LENGTH_MEASURE( 1.000000000000000082E-05 ), #22024, 'distance_accuracy_value', 'NONE');
#6761 = CARTESIAN_POINT ( 'NONE',  ( 10.76134431155039373, 16.44521483549405971, -15.93742948484896615 ) ) ;
#6762 = LINE ( 'NONE', #18196, #20456 ) ;
#6763 = EDGE_LOOP ( 'NONE', ( #30100, #6098, #18821, #24033 ) ) ;
#6764 = VECTOR ( 'NONE', #8294, 1000.000000000000000 ) ;
#6765 = FACE_OUTER_BOUND ( 'NONE', #29980, .T. ) ;
#6766 = VERTEX_POINT ( 'NONE', #18406 ) ;
#6767 = CARTESIAN_POINT ( 'NONE',  ( 9.641350810849047548, 17.66889113945805789, -17.92015940598198753 ) ) ;
#6768 = CARTESIAN_POINT ( 'NONE',  ( 17.65249788084269511, 8.387921445357553907, -19.05198057976592452 ) ) ;
#6769 = DIRECTION ( 'NONE',  ( 1.110223024625156540E-16, 2.995891024602366092E-32, 1.000000000000000000 ) ) ;
#6770 = DIRECTION ( 'NONE',  ( -1.000000000000000000, 0.000000000000000000, -0.000000000000000000 ) ) ;
#6772 = ORIENTED_EDGE ( 'NONE', *, *, #3348, .F. ) ;
#6771 = CARTESIAN_POINT ( 'NONE',  ( 28.16462234717350199, -5.661059359726887230, -16.30864077692347536 ) ) ;
#6773 = TOROIDAL_SURFACE ( 'NONE', #13099, 2.700000000000001066, 0.2000000000000000111 ) ;
#6774 = VERTEX_POINT ( 'NONE', #20236 ) ;
#6775 = DIRECTION ( 'NONE',  ( 0.5877852522924731371, 1.586114251531760728E-16, -0.8090169943749474513 ) ) ;
#6776 = CARTESIAN_POINT ( 'NONE',  ( 12.26214823032917778, 9.523620991859985452, -15.31974707146758341 ) ) ;
#6777 = ORIENTED_EDGE ( 'NONE', *, *, #6567, .F. ) ;
#6778 = EDGE_CURVE ( 'NONE', #9083, #14185, #20538, .T. ) ;
#6779 = AXIS2_PLACEMENT_3D ( 'NONE', #2750, #12187, #13055 ) ;
#6780 = CARTESIAN_POINT ( 'NONE',  ( 35.37764311538968087, -21.41652447078215005, -19.89511094362359955 ) ) ;
#6781 = DIRECTION ( 'NONE',  ( 0.5877852522924731371, 1.586114251531760728E-16, 0.8090169943749474513 ) ) ;
#6782 = ORIENTED_EDGE ( 'NONE', *, *, #17366, .F. ) ;
#6783 = EDGE_CURVE ( 'NONE', #13070, #5527, #22551, .T. ) ;
#6784 = CARTESIAN_POINT ( 'NONE',  ( -31.74999999999995737, 0.000000000000000000, 2.500000000000000888 ) ) ;
#6785 = EDGE_CURVE ( 'NONE', #3713, #22665, #4374, .T. ) ;
#6786 = CARTESIAN_POINT ( 'NONE',  ( 20.82085833995528290, -1.902372073343062908, -15.34044165217533617 ) ) ;
#6787 = ORIENTED_EDGE ( 'NONE', *, *, #9162, .T. ) ;
#6788 = LINE ( 'NONE', #28026, #19320 ) ;
#6789 =( NAMED_UNIT ( * ) PLANE_ANGLE_UNIT ( ) SI_UNIT ( $, .RADIAN. ) );
#6790 = CARTESIAN_POINT ( 'NONE',  ( 13.15390973649967599, 8.859676595473322536, -14.60899741038990562 ) ) ;
#6791 = CARTESIAN_POINT ( 'NONE',  ( 28.34689840388910653, -5.967659833748593101, -13.48819167749268644 ) ) ;
#6792 = ORIENTED_EDGE ( 'NONE', *, *, #13566, .T. ) ;
#6793 = CARTESIAN_POINT ( 'NONE',  ( 143.6922820468854525, -10.00000000000000355, -17.92658477444275889 ) ) ;
#6794 = VECTOR ( 'NONE', #20005, 1000.000000000000000 ) ;
#6795 = DIRECTION ( 'NONE',  ( 0.5877852522924731371, 1.586114251531760728E-16, -0.8090169943749474513 ) ) ;
#6796 = AXIS2_PLACEMENT_3D ( 'NONE', #23766, #16272, #2417 ) ;
#6797 = ORIENTED_EDGE ( 'NONE', *, *, #11613, .F. ) ;
#6798 = CLOSED_SHELL ( 'NONE', ( #21266, #4061, #12742, #6439, #21342, #24110, #25546, #11795, #26786, #21093, #25212, #17075, #18523, #19902, #20814, #21936, #25449, #4438, #8867, #21278 ) ) ;
#6799 = DIRECTION ( 'NONE',  ( 1.000000000000000000, 2.168404344971006896E-16, 0.000000000000000000 ) ) ;
#6800 = LINE ( 'NONE', #9057, #3828 ) ;
#6801 = CARTESIAN_POINT ( 'NONE',  ( 144.5152310637605808, -10.00000000000000355, -11.28819510263909542 ) ) ;
#6802 = CARTESIAN_POINT ( 'NONE',  ( 172.0152310637604671, -9.999999999999994671, -15.61832212156129707 ) ) ;
#6803 = CARTESIAN_POINT ( 'NONE',  ( 25.92522129715230506, 0.6472387150544522960, -15.98534533675435299 ) ) ;
#6804 = CARTESIAN_POINT ( 'NONE',  ( 17.40782953567980229, 3.270613820851801190, -14.52895612053623609 ) ) ;
#6805 = CARTESIAN_POINT ( 'NONE',  ( 36.54859682288668665, -23.18452892187019643, -18.24988411864624993 ) ) ;
#6806 = CARTESIAN_POINT ( 'NONE',  ( 11.49350937636955372, 9.187954247928445284, -15.85136552863131421 ) ) ;
#6807 = DIRECTION ( 'NONE',  ( -0.9510565162951536422, 0.000000000000000000, -0.3090169943749472292 ) ) ;
#6808 = CARTESIAN_POINT ( 'NONE',  ( 0.000000000000000000, 0.000000000000000000, -2.450000000000000178 ) ) ;
#6809 = CARTESIAN_POINT ( 'NONE',  ( 9.662182123323882266, 16.25345509848694547, -17.90638241064055336 ) ) ;
#6811 = ORIENTED_EDGE ( 'NONE', *, *, #1803, .T. ) ;
#6810 = LINE ( 'NONE', #8780, #29821 ) ;
#6812 = ORIENTED_EDGE ( 'NONE', *, *, #17074, .T. ) ;
#6813 = DIRECTION ( 'NONE',  ( 0.9510565162951536422, 2.566386769018988816E-16, 0.3090169943749472292 ) ) ;
#6814 = CARTESIAN_POINT ( 'NONE',  ( 12.49271550807400999, 8.567542729147559655, -15.13597632865050535 ) ) ;
#6815 = ORIENTED_EDGE ( 'NONE', *, *, #16699, .F. ) ;
#6816 = AXIS2_PLACEMENT_3D ( 'NONE', #15988, #18436, #23163 ) ;
#6817 = DIRECTION ( 'NONE',  ( -0.9510565162951536422, -2.566386769018988816E-16, -0.3090169943749472292 ) ) ;
#6818 = DIRECTION ( 'NONE',  ( -0.5877852522924731371, -1.586114251531760235E-16, 0.8090169943749474513 ) ) ;
#6819 = EDGE_CURVE ( 'NONE', #8969, #24258, #4904, .T. ) ;
#6820 = LINE ( 'NONE', #27466, #29334 ) ;
#6821 = EDGE_CURVE ( 'NONE', #7982, #7358, #13372, .T. ) ;
#6822 = ORIENTED_EDGE ( 'NONE', *, *, #26182, .T. ) ;
#6823 = ADVANCED_FACE ( 'NONE', ( #15664 ), #4224, .F. ) ;
#6824 = AXIS2_PLACEMENT_3D ( 'NONE', #3350, #24399, #7910 ) ;
#6825 = EDGE_LOOP ( 'NONE', ( #7150, #20706, #4882, #3677, #23875 ) ) ;
#6826 = EDGE_CURVE ( 'NONE', #27678, #25209, #17941, .T. ) ;
#6827 = CARTESIAN_POINT ( 'NONE',  ( 9.113591243665672081, 16.17650713204097102, -17.05428594964136835 ) ) ;
#6828 = CARTESIAN_POINT ( 'NONE',  ( 32.84381624265927968, -11.41053889131397980, -20.36336433681493929 ) ) ;
#6829 = CARTESIAN_POINT ( 'NONE',  ( 21.03983889671009422, 4.536326888612346231, -13.89983168792289270 ) ) ;
#6830 = CARTESIAN_POINT ( 'NONE',  ( 19.47111902912460124, 6.782054727477878409, -15.90798308235397407 ) ) ;
#6831 = DIRECTION ( 'NONE',  ( 1.000000000000000000, 4.440892098500622217E-16, 0.000000000000000000 ) ) ;
#6832 = CARTESIAN_POINT ( 'NONE',  ( 26.15289264771154620, -4.614421047071551207, -20.21764904625508663 ) ) ;
#6833 = ORIENTED_EDGE ( 'NONE', *, *, #22246, .T. ) ;
#6834 = CARTESIAN_POINT ( 'NONE',  ( 167.0152310637604955, -9.999999999999996447, -15.61832212156129707 ) ) ;
#6835 = AXIS2_PLACEMENT_3D ( 'NONE', #23372, #339, #4606 ) ;
#6836 = VECTOR ( 'NONE', #3330, 1000.000000000000000 ) ;
#6838 = VERTEX_POINT ( 'NONE', #9079 ) ;
#6837 = CARTESIAN_POINT ( 'NONE',  ( 0.000000000000000000, 0.000000000000000000, 18.00000000000000000 ) ) ;
#6839 = ORIENTED_EDGE ( 'NONE', *, *, #2649, .F. ) ;
#6840 = VECTOR ( 'NONE', #7687, 1000.000000000000000 ) ;
#6841 = CARTESIAN_POINT ( 'NONE',  ( 148.6922820468853672, -10.00000000000000355, -0.6060766987539614181 ) ) ;
#6842 = VECTOR ( 'NONE', #14730, 1000.000000000000000 ) ;
#6843 = LINE ( 'NONE', #25589, #3419 ) ;
#6844 = CARTESIAN_POINT ( 'NONE',  ( 35.53758243340352863, -21.13504710440451007, -18.64505253599016044 ) ) ;
#6845 = CARTESIAN_POINT ( 'NONE',  ( 11.03967536873724242, 8.192193740582544237, -16.19303379925286279 ) ) ;
#6846 = ORIENTED_EDGE ( 'NONE', *, *, #26970, .T. ) ;
#6847 = CARTESIAN_POINT ( 'NONE',  ( 76.63953071969194752, -4.999999999999996447, 55.68187839422949281 ) ) ;
#6848 = LINE ( 'NONE', #13984, #12853 ) ;
#6849 = CARTESIAN_POINT ( 'NONE',  ( 10.35870477237433818, 16.97187010017241349, -17.89775757279876700 ) ) ;
#6850 = CARTESIAN_POINT ( 'NONE',  ( 24.00000000000017053, 34.64101615137744972, 10.00000000000000178 ) ) ;
#6851 = CARTESIAN_POINT ( 'NONE',  ( 153.6922820468854525, -4.999999999999975131, -32.39392330124607611 ) ) ;
#6852 = CIRCLE ( 'NONE', #515, 8.000000000000005329 ) ;
#6853 = VERTEX_POINT ( 'NONE', #17794 ) ;
#6854 = AXIS2_PLACEMENT_3D ( 'NONE', #8148, #24195, #10430 ) ;
#6855 = PLANE ( 'NONE',  #1257 ) ;
#6856 = EDGE_CURVE ( 'NONE', #29309, #10540, #27757, .T. ) ;
#6857 = DIRECTION ( 'NONE',  ( 0.000000000000000000, 0.000000000000000000, 1.000000000000000000 ) ) ;
#6858 = ORIENTED_EDGE ( 'NONE', *, *, #7905, .T. ) ;
#6859 = ADVANCED_FACE ( 'NONE', ( #22696 ), #13072, .T. ) ;
#6860 = DIRECTION ( 'NONE',  ( 0.000000000000000000, 0.000000000000000000, 1.000000000000000000 ) ) ;
#6861 = VERTEX_POINT ( 'NONE', #11235 ) ;
#6862 = EDGE_CURVE ( 'NONE', #10393, #25794, #29777, .T. ) ;
#6863 = CARTESIAN_POINT ( 'NONE',  ( 9.666286124033039329, 16.23463362809610899, -17.88661257689534878 ) ) ;
#6864 = AXIS2_PLACEMENT_3D ( 'NONE', #17071, #14615, #15065 ) ;
#6865 = CARTESIAN_POINT ( 'NONE',  ( 22.25649556587329414, -4.532042753231527499, -15.61575944733927024 ) ) ;
#6866 = CARTESIAN_POINT ( 'NONE',  ( 22.01749846045582970, -4.595750957016929483, -16.30794181244783303 ) ) ;
#6867 = CARTESIAN_POINT ( 'NONE',  ( 22.84118038848623655, 1.850029439873439152, -18.07216660426987431 ) ) ;
#6868 = CARTESIAN_POINT ( 'NONE',  ( 137.0152310637605808, -1.999999999999979572, -17.38167787843870826 ) ) ;
#6869 = CARTESIAN_POINT ( 'NONE',  ( 172.0152310637604103, -1.999999999999970912, 1.702185954127501066 ) ) ;
#6870 = DIRECTION ( 'NONE',  ( 0.9510565162951535312, 2.566386769018988816E-16, -0.3090169943749475623 ) ) ;
#6871 = CARTESIAN_POINT ( 'NONE',  ( 21.69765170278760280, -5.035756590920279940, -14.89200278627170881 ) ) ;
#6872 = CARTESIAN_POINT ( 'NONE',  ( 130.7287565553229456, -4.999999999999983125, 3.500000000000003109 ) ) ;
#6873 = VECTOR ( 'NONE', #13549, 1000.000000000000000 ) ;
#6874 = DIRECTION ( 'NONE',  ( -1.000000000000000000, 0.000000000000000000, 0.000000000000000000 ) ) ;
#6875 = DIRECTION ( 'NONE',  ( -2.698458740408365879E-16, 1.000000000000000000, 0.000000000000000000 ) ) ;
#6876 = CIRCLE ( 'NONE', #23944, 2.000000000000000000 ) ;
#6877 = FACE_OUTER_BOUND ( 'NONE', #6271, .T. ) ;
#6878 = DIRECTION ( 'NONE',  ( 0.5877852522924731371, 1.586114251531760728E-16, 0.8090169943749474513 ) ) ;
#6879 = EDGE_CURVE ( 'NONE', #10809, #23695, #6517, .T. ) ;
#6880 = CARTESIAN_POINT ( 'NONE',  ( 10.45680941692980959, 16.52194969480735764, -17.34528143170414083 ) ) ;
#6881 = CARTESIAN_POINT ( 'NONE',  ( 0.000000000000000000, 0.000000000000000000, -2.144516984716112518 ) ) ;
#6882 =( GEOMETRIC_REPRESENTATION_CONTEXT ( 3 ) GLOBAL_UNCERTAINTY_ASSIGNED_CONTEXT ( ( #16508 ) ) GLOBAL_UNIT_ASSIGNED_CONTEXT ( ( #14232, #3562, #21571 ) ) REPRESENTATION_CONTEXT ( 'NONE', 'WORKASPACE' ) );
#6883 = CARTESIAN_POINT ( 'NONE',  ( 143.6922820468854525, -1.999999999999978684, -32.39392330124607611 ) ) ;
#6884 = ORIENTED_EDGE ( 'NONE', *, *, #18246, .T. ) ;
#6885 = ORIENTED_EDGE ( 'NONE', *, *, #14907, .F. ) ;
#6886 = CARTESIAN_POINT ( 'NONE',  ( 49.00000000000000000, 0.000000000000000000, 0.000000000000000000 ) ) ;
#6887 = CARTESIAN_POINT ( 'NONE',  ( 16.53342136567307108, 10.04554801986687629, -15.32032680638607047 ) ) ;
#6888 = CARTESIAN_POINT ( 'NONE',  ( 11.05542208158282769, 17.68939236555957706, -17.90700183802944778 ) ) ;
#6889 = CARTESIAN_POINT ( 'NONE',  ( 35.54859390953724585, -22.18451583373416014, -17.22552805718784441 ) ) ;
#6890 = VERTEX_POINT ( 'NONE', #1499 ) ;
#6891 = VERTEX_POINT ( 'NONE', #16257 ) ;
#6892 = EDGE_LOOP ( 'NONE', ( #7849, #29201, #1624, #4134, #13677 ) ) ;
#6893 = CARTESIAN_POINT ( 'NONE',  ( 9.641364314812712166, 17.66882920855936590, -17.90209449470656722 ) ) ;
#6894 = CARTESIAN_POINT ( 'NONE',  ( 13.02821298986966703, 7.746099194123166498, -14.70917993614958519 ) ) ;
#6895 = LINE ( 'NONE', #27531, #25872 ) ;
#6896 = CARTESIAN_POINT ( 'NONE',  ( 162.2287565553229740, -1.999999999999971800, -29.49038105676660493 ) ) ;
#6897 = EDGE_LOOP ( 'NONE', ( #21228, #15480, #10400, #2353 ) ) ;
#6898 = CARTESIAN_POINT ( 'NONE',  ( 153.6922820468854525, -1.999999999999974465, -35.24709285013155835 ) ) ;
#6899 = VERTEX_POINT ( 'NONE', #11974 ) ;
#6900 = CARTESIAN_POINT ( 'NONE',  ( 11.37973238226026318, 12.28930733048782642, -16.95943368139929319 ) ) ;
#6901 = CIRCLE ( 'NONE', #1545, 2.928571428571432378 ) ;
#6903 = VECTOR ( 'NONE', #1461, 1000.000000000000000 ) ;
#6902 = CARTESIAN_POINT ( 'NONE',  ( 36.54859390953724585, -21.18451583373416014, -17.99055332684694974 ) ) ;
#6904 = CARTESIAN_POINT ( 'NONE',  ( 26.31132954256896639, -3.159408024760113509, -14.81636702655834803 ) ) ;
#6905 = DIRECTION ( 'NONE',  ( 0.000000000000000000, 0.000000000000000000, 1.000000000000000000 ) ) ;
#6906 = CARTESIAN_POINT ( 'NONE',  ( -13.00000000000000178, -2.870178842070716726E-15, -23.00000000000000000 ) ) ;
#6907 = CARTESIAN_POINT ( 'NONE',  ( 0.000000000000000000, 0.000000000000000000, 0.000000000000000000 ) ) ;
#6908 = CARTESIAN_POINT ( 'NONE',  ( 17.37262532792671976, 6.041285449496323068, -14.53661901313261495 ) ) ;
#6909 = CARTESIAN_POINT ( 'NONE',  ( 23.72497280669020014, -7.722717790116627512, -18.49470058199314693 ) ) ;
#6910 = ORIENTED_EDGE ( 'NONE', *, *, #23626, .T. ) ;
#6911 = DIRECTION ( 'NONE',  ( -2.698458740408365879E-16, 1.000000000000000000, 0.000000000000000000 ) ) ;
#6912 = ADVANCED_FACE ( 'NONE', ( #4522 ), #6970, .T. ) ;
#6913 = CARTESIAN_POINT ( 'NONE',  ( 5.430258561686096108, -5.000000000000015987, 16.71261737790626256 ) ) ;
#6914 = FACE_OUTER_BOUND ( 'NONE', #11035, .T. ) ;
#6915 = EDGE_CURVE ( 'NONE', #25136, #18177, #13810, .T. ) ;
#6916 = DIRECTION ( 'NONE',  ( -2.698458740408365879E-16, 1.000000000000000000, 0.000000000000000000 ) ) ;
#6917 = CARTESIAN_POINT ( 'NONE',  ( 10.66955227599643408, 16.86618481130757630, -15.98952479117537173 ) ) ;
#6918 = DIRECTION ( 'NONE',  ( 2.908569913943826047E-16, -1.000000000000000000, 6.826925868028107924E-18 ) ) ;
#6919 = ORIENTED_EDGE ( 'NONE', *, *, #19274, .F. ) ;
#6920 = DIRECTION ( 'NONE',  ( -2.698458740408365879E-16, 1.000000000000000000, 0.000000000000000000 ) ) ;
#6921 = VERTEX_POINT ( 'NONE', #20834 ) ;
#6922 = CARTESIAN_POINT ( 'NONE',  ( 10.04637620539468124, 15.81139305134258599, -16.45082025127570091 ) ) ;
#6923 = AXIS2_PLACEMENT_3D ( 'NONE', #1136, #14837, #24174 ) ;
#6924 = CARTESIAN_POINT ( 'NONE',  ( 15.60254075764268755, 8.625145012302763092, -14.61600764054077395 ) ) ;
#6925 = LINE ( 'NONE', #11630, #38 ) ;
#6926 = DIRECTION ( 'NONE',  ( -2.698458740408365879E-16, 1.000000000000000000, 0.000000000000000000 ) ) ;
#6928 = EDGE_LOOP ( 'NONE', ( #13375, #29027, #7026, #15865, #23302 ) ) ;
#6927 = CARTESIAN_POINT ( 'NONE',  ( 28.01381056668970260, -10.10121741814351459, -18.82353034625045041 ) ) ;
#6929 = ORIENTED_EDGE ( 'NONE', *, *, #7533, .T. ) ;
#6930 = CARTESIAN_POINT ( 'NONE',  ( 4.000000000000000000, -0.3902508023145602190, -2.450000000000001066 ) ) ;
#6931 = CARTESIAN_POINT ( 'NONE',  ( 11.30853360504539751, 16.52859065474556033, -16.77115057629831441 ) ) ;
#6932 = CARTESIAN_POINT ( 'NONE',  ( 35.32886446602115171, -21.19738783794349857, -20.03221113960638178 ) ) ;
#6933 = CARTESIAN_POINT ( 'NONE',  ( 10.55189716074911921, 7.593251366112848899, 9.999999999999998224 ) ) ;
#6934 = ORIENTED_EDGE ( 'NONE', *, *, #28151, .T. ) ;
#6935 = CARTESIAN_POINT ( 'NONE',  ( 172.2287565553229456, -9.999999999999994671, -29.49038105676660493 ) ) ;
#6936 = VECTOR ( 'NONE', #17837, 1000.000000000000000 ) ;
#6937 = CARTESIAN_POINT ( 'NONE',  ( 23.62051642037636157, -5.854316150849339984, -13.42181569741374503 ) ) ;
#6938 = ORIENTED_EDGE ( 'NONE', *, *, #13349, .T. ) ;
#6939 = CARTESIAN_POINT ( 'NONE',  ( 153.6922820468854241, -10.00000000000000000, -23.73366926340167637 ) ) ;
#6940 =( NAMED_UNIT ( * ) PLANE_ANGLE_UNIT ( ) SI_UNIT ( $, .RADIAN. ) );
#6941 = CARTESIAN_POINT ( 'NONE',  ( 19.82332968365342296, 2.432204761014481242, -19.52120720162773537 ) ) ;
#6942 = CARTESIAN_POINT ( 'NONE',  ( 27.32534031592636836, -8.675155620653059785, -19.25315075663615971 ) ) ;
#6943 = EDGE_LOOP ( 'NONE', ( #28134, #12008, #8971, #8894 ) ) ;
#6944 = CARTESIAN_POINT ( 'NONE',  ( 5.200000000000002842, 0.000000000000000000, 0.000000000000000000 ) ) ;
#6945 = VECTOR ( 'NONE', #15857, 1000.000000000000114 ) ;
#6946 = CARTESIAN_POINT ( 'NONE',  ( 157.0152310637604387, -1.999999999999974909, -0.06116980274991495881 ) ) ;
#6947 = EDGE_CURVE ( 'NONE', #19572, #20829, #30217, .T. ) ;
#6948 = EDGE_CURVE ( 'NONE', #2774, #7135, #9227, .T. ) ;
#6949 = DIRECTION ( 'NONE',  ( -0.5877852522924731371, -1.586114251531760728E-16, -0.8090169943749474513 ) ) ;
#6950 = VERTEX_POINT ( 'NONE', #2248 ) ;
#6951 = ADVANCED_FACE ( 'NONE', ( #18554 ), #4817, .F. ) ;
#6952 = PLANE ( 'NONE',  #8482 ) ;
#6953 = VECTOR ( 'NONE', #19425, 1000.000000000000000 ) ;
#6954 = EDGE_CURVE ( 'NONE', #10786, #2363, #26043, .T. ) ;
#6955 = CARTESIAN_POINT ( 'NONE',  ( 9.641566850259106758, 17.66790035518494051, -17.86107206016944460 ) ) ;
#6956 = CARTESIAN_POINT ( 'NONE',  ( 24.71165717419137309, -6.805198111665588634, -19.34662478563667065 ) ) ;
#6957 = CARTESIAN_POINT ( 'NONE',  ( 21.50147616854745891, 4.214167280306792662, -18.19698480873994839 ) ) ;
#6958 = CARTESIAN_POINT ( 'NONE',  ( 31.91112766891453845, -10.28950255622343946, -18.29678896503644481 ) ) ;
#6959 = SURFACE_STYLE_USAGE ( .BOTH. , #9066 ) ;
#6960 = CARTESIAN_POINT ( 'NONE',  ( 119.3579561578551562, -4.999999999999985789, -86.71863120448111317 ) ) ;
#6961 = LINE ( 'NONE', #16249, #19551 ) ;
#6962 = DIRECTION ( 'NONE',  ( -1.000000000000000000, -2.698458740408365879E-16, 0.000000000000000000 ) ) ;
#6963 = DIRECTION ( 'NONE',  ( -2.698458740408365879E-16, 1.000000000000000000, 0.000000000000000000 ) ) ;
#6964 = ORIENTED_EDGE ( 'NONE', *, *, #19238, .F. ) ;
#6965 = DIRECTION ( 'NONE',  ( 0.5877852522924731371, 1.586114251531760728E-16, -0.8090169943749474513 ) ) ;
#6966 = CARTESIAN_POINT ( 'NONE',  ( 10.33811693838771717, 18.38618951776012267, -17.94384837343789130 ) ) ;
#6967 = B_SPLINE_CURVE_WITH_KNOTS ( 'NONE', 3,
 ( #12893, #6041, #8470, #1320, #13205, #10609 ),
 .UNSPECIFIED., .F., .F.,
 ( 4, 2, 4 ),
 ( 2.380731630115174505E-07, 0.002336973833157602806, 0.004673709593152193878 ),
 .UNSPECIFIED. ) ;
#6968 = EDGE_LOOP ( 'NONE', ( #4621, #6348, #23415, #5393 ) ) ;
#6969 = PLANE ( 'NONE',  #13456 ) ;
#6970 = PLANE ( 'NONE',  #567 ) ;
#6971 = CARTESIAN_POINT ( 'NONE',  ( 18.69974902744413470, 8.051839821468062652, -15.50866580261103955 ) ) ;
#6972 = ORIENTED_EDGE ( 'NONE', *, *, #26601, .T. ) ;
#6973 = VERTEX_POINT ( 'NONE', #23139 ) ;
#6974 = CARTESIAN_POINT ( 'NONE',  ( 32.98128152813007574, -11.80310687477359188, -20.53574887303233609 ) ) ;
#6975 = CARTESIAN_POINT ( 'NONE',  ( 22.08459858401872467, -3.550466661657427636, -14.88928395763347723 ) ) ;
#6976 = CARTESIAN_POINT ( 'NONE',  ( 16.98323446405135329, 7.186294067752427850, -20.40390978395066313 ) ) ;
#6977 = VECTOR ( 'NONE', #28676, 1000.000000000000000 ) ;
#6978 = CARTESIAN_POINT ( 'NONE',  ( 27.64540148246904749, -2.072091111371471506, -15.50399641584551702 ) ) ;
#6979 = VERTEX_POINT ( 'NONE', #16723 ) ;
#6980 = DIRECTION ( 'NONE',  ( 0.9510565162951536422, 0.000000000000000000, -0.3090169943749475623 ) ) ;
#6982 = ORIENTED_EDGE ( 'NONE', *, *, #3646, .F. ) ;
#6981 = DIRECTION ( 'NONE',  ( -2.698458740408365879E-16, 1.000000000000000000, 0.000000000000000000 ) ) ;
#6983 = VERTEX_POINT ( 'NONE', #27911 ) ;
#6984 = ADVANCED_FACE ( 'NONE', ( #7267 ), #23290, .T. ) ;
#6985 = PLANE ( 'NONE',  #4614 ) ;
#6986 = EDGE_CURVE ( 'NONE', #23467, #19109, #14192, .T. ) ;
#6987 = EDGE_CURVE ( 'NONE', #17600, #4081, #14411, .T. ) ;
#6988 = CARTESIAN_POINT ( 'NONE',  ( 47.87499999999999289, -1.320193954157388764E-16, 4.756499999999999062 ) ) ;
#6989 = CARTESIAN_POINT ( 'NONE',  ( 32.83462640711407232, -10.30445905196369516, -16.67331141712644538 ) ) ;
#6990 = CARTESIAN_POINT ( 'NONE',  ( 12.74005437760208181, 7.618877980503234504, -14.93883819022932080 ) ) ;
#6991 = ORIENTED_EDGE ( 'NONE', *, *, #28381, .T. ) ;
#6992 = AXIS2_PLACEMENT_3D ( 'NONE', #28193, #23890, #7248 ) ;
#6993 = CARTESIAN_POINT ( 'NONE',  ( 162.0152310637605524, -1.999999999999971800, -32.93883019725009120 ) ) ;
#6994 = CARTESIAN_POINT ( 'NONE',  ( 49.00000000000000000, 1.387778780781445676E-16, -5.000000000000000888 ) ) ;
#6995 = CARTESIAN_POINT ( 'NONE',  ( 10.60167031212029443, 15.85759916399494607, -17.28118971735050735 ) ) ;
#6996 = CARTESIAN_POINT ( 'NONE',  ( 159.7287565553230024, -1.999999999999972244, -33.82050807568879947 ) ) ;
#6997 = FACE_OUTER_BOUND ( 'NONE', #22827, .T. ) ;
#6998 = ORIENTED_EDGE ( 'NONE', *, *, #24395, .T. ) ;
#6999 = VERTEX_POINT ( 'NONE', #2401 ) ;
#7000 = DIRECTION ( 'NONE',  ( -0.9510565162951536422, -2.566386769018988816E-16, -0.3090169943749472292 ) ) ;
#7001 = CARTESIAN_POINT ( 'NONE',  ( 0.000000000000000000, 0.000000000000000000, -5.000000000000000888 ) ) ;
#7002 = EDGE_LOOP ( 'NONE', ( #6247, #22653, #10221, #1072 ) ) ;
#7003 = DIRECTION ( 'NONE',  ( 1.000000000000000000, 0.000000000000000000, 0.000000000000000000 ) ) ;
#7004 = ORIENTED_EDGE ( 'NONE', *, *, #1719, .T. ) ;
#7005 = CARTESIAN_POINT ( 'NONE',  ( 9.668188843004273281, 16.22590751635418371, -17.88494344602179709 ) ) ;
#7006 = CARTESIAN_POINT ( 'NONE',  ( 21.31799488982693802, -2.441251725956471219, -14.24326171688714204 ) ) ;
#7007 = CARTESIAN_POINT ( 'NONE',  ( 22.25649556587329414, -4.532042753231527499, -15.61575944733927024 ) ) ;
#7008 = CARTESIAN_POINT ( 'NONE',  ( 21.19231167106929803, 0.1271100694386541607, -19.24388053421374778 ) ) ;
#7009 = CARTESIAN_POINT ( 'NONE',  ( 143.6922820468853956, -10.00000000000000533, -0.6060766987539614181 ) ) ;
#7010 = CARTESIAN_POINT ( 'NONE',  ( 158.6922820468854241, -9.999999999999998224, -35.24709285013155835 ) ) ;
#7011 = LINE ( 'NONE', #23331, #9363 ) ;
#7012 = CARTESIAN_POINT ( 'NONE',  ( 25.67262840375075328, -3.322766148301121714, -14.04542551033457798 ) ) ;
#7013 = AXIS2_PLACEMENT_3D ( 'NONE', #25012, #4097, #29799 ) ;
#7014 = LINE ( 'NONE', #16614, #2779 ) ;
#7015 = LINE ( 'NONE', #27958, #25479 ) ;
#7016 = CARTESIAN_POINT ( 'NONE',  ( -22.75000000000017053, 34.64101615137744972, 0.000000000000000000 ) ) ;
#7017 = EDGE_CURVE ( 'NONE', #29240, #8141, #254, .T. ) ;
#7018 = EDGE_CURVE ( 'NONE', #29468, #23116, #20991, .T. ) ;
#7019 = DIRECTION ( 'NONE',  ( -0.5877852522924731371, 0.000000000000000000, 0.8090169943749474513 ) ) ;
#7020 = CARTESIAN_POINT ( 'NONE',  ( 132.2287565553230024, -1.999999999999981348, -3.509618943233403510 ) ) ;
#7021 = EDGE_CURVE ( 'NONE', #13222, #6861, #2692, .T. ) ;
#7022 = EDGE_CURVE ( 'NONE', #25081, #10203, #9531, .T. ) ;
#7023 = CARTESIAN_POINT ( 'NONE',  ( 10.35864918915110877, 16.97212501191939538, -17.91664992932186351 ) ) ;
#7024 = FACE_OUTER_BOUND ( 'NONE', #25518, .T. ) ;
#7025 = CARTESIAN_POINT ( 'NONE',  ( 32.00110207675911767, -10.95298233446834502, -16.54939777171900417 ) ) ;
#7026 = ORIENTED_EDGE ( 'NONE', *, *, #5327, .T. ) ;
#7027 = CARTESIAN_POINT ( 'NONE',  ( 11.22494245711612848, 9.086454032755447940, -17.24116976563960435 ) ) ;
#7028 = VERTEX_POINT ( 'NONE', #14260 ) ;
#7029 = DIRECTION ( 'NONE',  ( -1.110223024625156540E-16, 0.000000000000000000, -1.000000000000000000 ) ) ;
#7030 = CARTESIAN_POINT ( 'NONE',  ( 21.63873165585565417, 2.424707942738766331, -13.54651715722292060 ) ) ;
#7031 = CARTESIAN_POINT ( 'NONE',  ( 11.09873500484433606, 17.49075377836879497, -17.25232203421226274 ) ) ;
#7032 = LINE ( 'NONE', #13432, #24858 ) ;
#7033 = VERTEX_POINT ( 'NONE', #98 ) ;
#7034 = EDGE_LOOP ( 'NONE', ( #15544, #8379, #5614, #28228 ) ) ;
#7035 = CARTESIAN_POINT ( 'NONE',  ( 9.641350810849047548, 17.66889113945805789, -17.91664992932186351 ) ) ;
#7036 = FACE_OUTER_BOUND ( 'NONE', #5870, .T. ) ;
#7037 = AXIS2_PLACEMENT_3D ( 'NONE', #2123, #14279, #30237 ) ;
#7038 = CARTESIAN_POINT ( 'NONE',  ( 9.641350944112486943, 17.66889052829492002, -17.91441860517739215 ) ) ;
#7039 = LINE ( 'NONE', #21067, #10271 ) ;
#7040 = FACE_OUTER_BOUND ( 'NONE', #924, .T. ) ;
#7041 = VERTEX_POINT ( 'NONE', #16111 ) ;
#7042 = LINE ( 'NONE', #14034, #24226 ) ;
#7043 = ORIENTED_EDGE ( 'NONE', *, *, #5815, .F. ) ;
#7044 = CARTESIAN_POINT ( 'NONE',  ( 10.47452605456472696, 16.44069893626776491, -17.33376834041267145 ) ) ;
#7045 = EDGE_LOOP ( 'NONE', ( #6541, #15446, #22071, #14491 ) ) ;
#7046 = CARTESIAN_POINT ( 'NONE',  ( 36.54460969663918490, -22.16661687567949457, -18.62492107750662029 ) ) ;
#7047 = CARTESIAN_POINT ( 'NONE',  ( 27.83100014064079275, -5.545984359997562230, -15.13782040115233052 ) ) ;
#7048 = ORIENTED_EDGE ( 'NONE', *, *, #18941, .F. ) ;
#7049 = FACE_OUTER_BOUND ( 'NONE', #23783, .T. ) ;
#7050 = AXIS2_PLACEMENT_3D ( 'NONE', #11624, #14060, #13909 ) ;
#7051 = CARTESIAN_POINT ( 'NONE',  ( 34.41982446195410716, -12.62108234628556680, -19.94648786050102274 ) ) ;
#7052 = CARTESIAN_POINT ( 'NONE',  ( 0.000000000000000000, 0.000000000000000000, -37.50000000000000000 ) ) ;
#7053 = CARTESIAN_POINT ( 'NONE',  ( 14.24687995347741420, 8.287322832548987606, -13.87414582376881000 ) ) ;
#7054 = CARTESIAN_POINT ( 'NONE',  ( 26.77273401934504093, -11.50074486517209138, -16.59227217106661101 ) ) ;
#7055 = ORIENTED_EDGE ( 'NONE', *, *, #12445, .F. ) ;
#7056 = FACE_BOUND ( 'NONE', #24704, .T. ) ;
#7057 = AXIS2_PLACEMENT_3D ( 'NONE', #8583, #3722, #22494 ) ;
#7058 = EDGE_CURVE ( 'NONE', #23288, #26251, #28056, .T. ) ;
#7059 = ADVANCED_FACE ( 'NONE', ( #16414 ), #25735, .T. ) ;
#7060 = CARTESIAN_POINT ( 'NONE',  ( 137.2287565553230309, -1.999999999999979572, -29.49038105676660138 ) ) ;
#7061 = LINE ( 'NONE', #21543, #18958 ) ;
#7062 = FACE_OUTER_BOUND ( 'NONE', #11556, .T. ) ;
#7063 = CARTESIAN_POINT ( 'NONE',  ( 10.72042364955539284, 16.63288220757436164, -15.95435249082810003 ) ) ;
#7064 = LINE ( 'NONE', #2352, #25078 ) ;
#7065 = ORIENTED_EDGE ( 'NONE', *, *, #13610, .F. ) ;
#7066 = DIRECTION ( 'NONE',  ( -0.5877852522924731371, -1.586114251531760235E-16, 0.8090169943749474513 ) ) ;
#7067 = ORIENTED_EDGE ( 'NONE', *, *, #1804, .T. ) ;
#7068 = CARTESIAN_POINT ( 'NONE',  ( 11.44040408106239326, 9.418203516307107392, -15.87434068686103394 ) ) ;
#7069 = ORIENTED_EDGE ( 'NONE', *, *, #15291, .F. ) ;
#7070 = CARTESIAN_POINT ( 'NONE',  ( 18.03247465133560468, 8.846858265128714649, -18.47062581007826410 ) ) ;
#7071 = CARTESIAN_POINT ( 'NONE',  ( 133.6922820468854241, -10.00000000000000711, -35.24709285013155835 ) ) ;
#7072 = DIRECTION ( 'NONE',  ( 0.5877852522924731371, 1.586114251531760728E-16, -0.8090169943749474513 ) ) ;
#7073 = CARTESIAN_POINT ( 'NONE',  ( 26.38113052396219516, -11.59678093645141672, -17.84452879788985769 ) ) ;
#7074 = ORIENTED_EDGE ( 'NONE', *, *, #8524, .T. ) ;
#7075 = CARTESIAN_POINT ( 'NONE',  ( 23.08382991343894020, -5.000000000000011546, -71.04472329954472798 ) ) ;
#7076 = CARTESIAN_POINT ( 'NONE',  ( 11.27495124880614163, 16.68260362121340279, -16.78505081266910182 ) ) ;
#7077 = CARTESIAN_POINT ( 'NONE',  ( 35.54859477393411993, -21.18451971701249548, -18.28760485896911803 ) ) ;
#7078 = DIRECTION ( 'NONE',  ( 0.9510565162951536422, 0.000000000000000000, -0.3090169943749475623 ) ) ;
#7079 = VECTOR ( 'NONE', #4585, 1000.000000000000000 ) ;
#7080 = ADVANCED_FACE ( 'NONE', ( #24057 ), #19600, .T. ) ;
#7081 = CARTESIAN_POINT ( 'NONE',  ( 163.6922820468853956, -1.999999999999971800, -35.24709285013155835 ) ) ;
#7082 = CARTESIAN_POINT ( 'NONE',  ( 25.92665957894408280, -9.004797978260709712, -12.14503282074142909 ) ) ;
#7083 = VERTEX_POINT ( 'NONE', #19747 ) ;
#7084 = DIRECTION ( 'NONE',  ( -2.698458740408365879E-16, 1.000000000000000000, 0.000000000000000000 ) ) ;
#7085 = EDGE_CURVE ( 'NONE', #10807, #1890, #5276, .T. ) ;
#7086 = CARTESIAN_POINT ( 'NONE',  ( 18.75392633456350922, 0.8452085672475394551, -14.97946080469353447 ) ) ;
#7087 = CARTESIAN_POINT ( 'NONE',  ( 16.02697758069565381, 6.204487712298734081, -15.55946274640501237 ) ) ;
#7088 = ORIENTED_EDGE ( 'NONE', *, *, #13757, .T. ) ;
#7089 = DIRECTION ( 'NONE',  ( -2.698458740408365879E-16, 1.000000000000000000, 0.000000000000000000 ) ) ;
#7090 = DIRECTION ( 'NONE',  ( 1.000000000000000000, 4.440892098500622217E-16, 0.000000000000000000 ) ) ;
#7091 = ORIENTED_EDGE ( 'NONE', *, *, #15854, .F. ) ;
#7092 = CARTESIAN_POINT ( 'NONE',  ( 156.1922820468853672, -4.999999999999976019, -13.59645775552055902 ) ) ;
#7093 = PLANE ( 'NONE',  #9269 ) ;
#7094 = FACE_OUTER_BOUND ( 'NONE', #27794, .T. ) ;
#7095 = VECTOR ( 'NONE', #5721, 1000.000000000000000 ) ;
#7096 = CARTESIAN_POINT ( 'NONE',  ( 9.912057827679275235, 16.42739425315605928, -16.50652470164456531 ) ) ;
#7097 = CARTESIAN_POINT ( 'NONE',  ( 23.31633574299079825, -8.368445843159939557, -15.61931793633953980 ) ) ;
#7098 = CARTESIAN_POINT ( 'NONE',  ( 19.60850488237918654, -1.635242255716521820, -15.65509664672261003 ) ) ;
#7100 = ORIENTED_EDGE ( 'NONE', *, *, #23136, .F. ) ;
#7099 = CARTESIAN_POINT ( 'NONE',  ( 32.08869746025642655, -10.33200466608398216, -18.78962723441388150 ) ) ;
#7101 = CARTESIAN_POINT ( 'NONE',  ( 12.53458732174692258, 8.585986940276173485, -15.10260830673100330 ) ) ;
#7102 = DIRECTION ( 'NONE',  ( 0.3090169943749472292, 8.338696094057992503E-17, -0.9510565162951536422 ) ) ;
#7103 = CARTESIAN_POINT ( 'NONE',  ( 0.000000000000000000, 0.000000000000000000, 15.00000000000000000 ) ) ;
#7104 = CARTESIAN_POINT ( 'NONE',  ( 17.78594395145776019, 10.14170102421038422, -17.68001733040774681 ) ) ;
#7105 = ORIENTED_EDGE ( 'NONE', *, *, #11828, .T. ) ;
#7106 = CARTESIAN_POINT ( 'NONE',  ( 131.1922820468854241, -1.999999999999982236, -30.91696583120935671 ) ) ;
#7107 = CARTESIAN_POINT ( 'NONE',  ( 10.72113683966407294, 16.62961142682532767, -15.95405668885543982 ) ) ;
#7108 = ORIENTED_EDGE ( 'NONE', *, *, #3989, .T. ) ;
#7109 = CARTESIAN_POINT ( 'NONE',  ( -8.000000000000000000, 0.000000000000000000, 4.999999999999997335 ) ) ;
#7110 = CARTESIAN_POINT ( 'NONE',  ( 109.9631552159402617, -4.999999999999987566, -79.89290877803512103 ) ) ;
#7111 = AXIS2_PLACEMENT_3D ( 'NONE', #9110, #2584, #18740 ) ;
#7112 = CARTESIAN_POINT ( 'NONE',  ( 15.41431293496917121, 3.575304669039410133, -17.09800041271234150 ) ) ;
#7113 = VERTEX_POINT ( 'NONE', #26348 ) ;
#7114 = CARTESIAN_POINT ( 'NONE',  ( 17.49446177548951553, 10.34313653870878547, -20.19723249710358104 ) ) ;
#7115 = ORIENTED_EDGE ( 'NONE', *, *, #231, .T. ) ;
#7116 = CARTESIAN_POINT ( 'NONE',  ( 35.05385823632300912, -20.96193052275466329, -21.15110683048779805 ) ) ;
#7117 = EDGE_CURVE ( 'NONE', #19168, #29985, #23912, .T. ) ;
#7118 = ADVANCED_FACE ( 'NONE', ( #3157 ), #26399, .T. ) ;
#7119 = CARTESIAN_POINT ( 'NONE',  ( 21.15397186503396654, -1.756306506132798706, -15.01670888948634364 ) ) ;
#7120 = VECTOR ( 'NONE', #6775, 1000.000000000000000 ) ;
#7121 = EDGE_CURVE ( 'NONE', #11338, #28260, #8006, .T. ) ;
#7122 = CARTESIAN_POINT ( 'NONE',  ( 19.85629768685782537, 6.556105584440964584, -17.58075288388961965 ) ) ;
#7123 = VECTOR ( 'NONE', #5210, 1000.000000000000000 ) ;
#7124 = CARTESIAN_POINT ( 'NONE',  ( 29.08439603799166306, -5.802884797086306001, -14.52222230071497755 ) ) ;
#7125 = VERTEX_POINT ( 'NONE', #12580 ) ;
#7126 = EDGE_LOOP ( 'NONE', ( #20196, #1673, #5235, #3818, #9597 ) ) ;
#7127 = CARTESIAN_POINT ( 'NONE',  ( -8.000000000000000000, 4.618802153517028941, -4.285468820183664818 ) ) ;
#7129 = ORIENTED_EDGE ( 'NONE', *, *, #11864, .T. ) ;
#7128 = FACE_OUTER_BOUND ( 'NONE', #7034, .T. ) ;
#7130 = ORIENTED_EDGE ( 'NONE', *, *, #18694, .T. ) ;
#7131 = CARTESIAN_POINT ( 'NONE',  ( 163.6922820468853388, -1.999999999999972244, -15.07341522555727664 ) ) ;
#7132 = CARTESIAN_POINT ( 'NONE',  ( -6.499999999999929834, -11.25833024919774239, -186.4312945166758482 ) ) ;
#7133 = CARTESIAN_POINT ( 'NONE',  ( 36.51492826578181194, -21.03327392953103825, -18.93061234292109063 ) ) ;
#7134 = CARTESIAN_POINT ( 'NONE',  ( 12.97376706329020557, 7.722038565090276308, -14.75257430067278719 ) ) ;
#7135 = VERTEX_POINT ( 'NONE', #5428 ) ;
#7136 = MECHANICAL_DESIGN_GEOMETRIC_PRESENTATION_REPRESENTATION (  '', ( #5174 ), #20264 ) ;
#7137 = FACE_OUTER_BOUND ( 'NONE', #13454, .T. ) ;
#7138 = LINE ( 'NONE', #16437, #4091 ) ;
#7139 = CARTESIAN_POINT ( 'NONE',  ( 10.46817501828509123, 16.46982559821503145, -17.33665662920367723 ) ) ;
#7140 = DIRECTION ( 'NONE',  ( 1.000000000000000000, 2.891205793294675861E-16, 0.000000000000000000 ) ) ;
#7141 = VERTEX_POINT ( 'NONE', #12430 ) ;
#7142 = CARTESIAN_POINT ( 'NONE',  ( 152.0152310637605808, -1.999999999999974909, -24.27857615940569502 ) ) ;
#7143 = ORIENTED_EDGE ( 'NONE', *, *, #1135, .T. ) ;
#7144 = LINE ( 'NONE', #25463, #15374 ) ;
#7145 = CARTESIAN_POINT ( 'NONE',  ( 0.000000000000000000, 0.000000000000000000, 18.00000000000000000 ) ) ;
#7146 = ORIENTED_EDGE ( 'NONE', *, *, #779, .T. ) ;
#7147 = ORIENTED_EDGE ( 'NONE', *, *, #8524, .F. ) ;
#7148 = ORIENTED_EDGE ( 'NONE', *, *, #27556, .F. ) ;
#7149 = PLANE ( 'NONE',  #19827 ) ;
#7150 = ORIENTED_EDGE ( 'NONE', *, *, #29044, .T. ) ;
#7151 = CARTESIAN_POINT ( 'NONE',  ( 9.667840685194843076, 16.22750421244806063, -17.88508776754438401 ) ) ;
#7152 = VERTEX_POINT ( 'NONE', #10140 ) ;
#7153 = ADVANCED_FACE ( 'NONE', ( #17170 ), #15165, .T. ) ;
#7154 = CARTESIAN_POINT ( 'NONE',  ( 26.91914097958202845, -7.808663323052361882, -12.67700453112951209 ) ) ;
#7155 = ADVANCED_FACE ( 'NONE', ( #24501 ), #10437, .T. ) ;
#7156 = ORIENTED_EDGE ( 'NONE', *, *, #15125, .F. ) ;
#7157 = EDGE_CURVE ( 'NONE', #16501, #14857, #14563, .T. ) ;
#7158 = CARTESIAN_POINT ( 'NONE',  ( 17.90640022563237110, 0.6078909361919438981, -17.24624654394265377 ) ) ;
#7159 = VECTOR ( 'NONE', #4341, 1000.000000000000000 ) ;
#7160 = LINE ( 'NONE', #21181, #26746 ) ;
#7161 = DIRECTION ( 'NONE',  ( -0.9510565162951536422, -2.566386769018988816E-16, -0.3090169943749472292 ) ) ;
#7162 = EDGE_CURVE ( 'NONE', #9008, #26117, #26653, .T. ) ;
#7163 = FACE_OUTER_BOUND ( 'NONE', #9097, .T. ) ;
#7164 = VECTOR ( 'NONE', #10819, 1000.000000000000000 ) ;
#7165 = CARTESIAN_POINT ( 'NONE',  ( 26.18758235895636233, -4.355437658720127558, -18.53605802859044260 ) ) ;
#7166 = STYLED_ITEM ( 'NONE', ( #2299 ), #21992 ) ;
#7167 = VERTEX_POINT ( 'NONE', #3590 ) ;
#7168 = CARTESIAN_POINT ( 'NONE',  ( 157.0152310637605524, -4.999999999999975131, -1.743219247438260759E-14 ) ) ;
#7169 = LINE ( 'NONE', #11569, #4048 ) ;
#7170 = PLANE ( 'NONE',  #9696 ) ;
#7171 = CARTESIAN_POINT ( 'NONE',  ( 152.0152310637605808, -4.999999999999976907, -1.687708096207003248E-14 ) ) ;
#7172 = LINE ( 'NONE', #14167, #16766 ) ;
#7173 = CARTESIAN_POINT ( 'NONE',  ( 12.02823749386838514, 9.315180647891255106, -16.69125397286443047 ) ) ;
#7174 = CARTESIAN_POINT ( 'NONE',  ( 141.1922820468854525, -1.999999999999978684, -22.25671179336495697 ) ) ;
#7175 = CARTESIAN_POINT ( 'NONE',  ( 32.30218501430429967, -10.99871056796995816, -17.40035725849610060 ) ) ;
#7176 = ORIENTED_EDGE ( 'NONE', *, *, #2644, .T. ) ;
#7177 = CARTESIAN_POINT ( 'NONE',  ( 13.36610298980765776, 7.620062051554192806, -15.71863358442526781 ) ) ;
#7178 = EDGE_LOOP ( 'NONE', ( #5553, #17019, #2064, #5245 ) ) ;
#7179 = PLANE ( 'NONE',  #11938 ) ;
#7180 = CARTESIAN_POINT ( 'NONE',  ( 19.61192361542596529, -2.405681417800469291, -14.70675912396028906 ) ) ;
#7181 = CARTESIAN_POINT ( 'NONE',  ( 11.26126983089308098, 16.74534834773793790, -16.79273533431442900 ) ) ;
#7182 = CARTESIAN_POINT ( 'NONE',  ( 132.2287565553230024, -1.999999999999981348, -20.83012701892220164 ) ) ;
#7183 = ORIENTED_EDGE ( 'NONE', *, *, #24181, .F. ) ;
#7184 = AXIS2_PLACEMENT_3D ( 'NONE', #23322, #2436, #21031 ) ;
#7185 = CARTESIAN_POINT ( 'NONE',  ( 9.641404825192898542, 17.66864342279195199, -17.88841768828662282 ) ) ;
#7186 = CARTESIAN_POINT ( 'NONE',  ( 15.44827550661201876, -5.000000000000013323, -47.54490320444753593 ) ) ;
#7187 = CARTESIAN_POINT ( 'NONE',  ( 11.39177520167864266, 9.641221755901229429, -15.89445043910815336 ) ) ;
#7188 = DIRECTION ( 'NONE',  ( 0.000000000000000000, 0.000000000000000000, 1.000000000000000000 ) ) ;
#7189 = CARTESIAN_POINT ( 'NONE',  ( 1.660531772554315610, -3.660093687634890181, -2.449999999999980194 ) ) ;
#7190 = ORIENTED_EDGE ( 'NONE', *, *, #3033, .F. ) ;
#7191 = CARTESIAN_POINT ( 'NONE',  ( 4.339467034331203621, 6.732211846623402884, -3.988960492936253045E-15 ) ) ;
#7192 = ORIENTED_EDGE ( 'NONE', *, *, #4021, .F. ) ;
#7193 = CARTESIAN_POINT ( 'NONE',  ( 10.48212431696843439, 16.40585233633115436, -17.33062619162406293 ) ) ;
#7194 = EDGE_LOOP ( 'NONE', ( #29370, #3220, #22730, #21377, #18320 ) ) ;
#7195 = CARTESIAN_POINT ( 'NONE',  ( 32.76003276007612186, -9.647047962658168885, -18.46200315532429315 ) ) ;
#7196 = CARTESIAN_POINT ( 'NONE',  ( 14.55381231002303188, 10.26819836692386723, -15.14301692386319331 ) ) ;
#7197 = CARTESIAN_POINT ( 'NONE',  ( 28.06689949639850212, -8.111051215268487269, -13.49421662364394514 ) ) ;
#7198 = EDGE_CURVE ( 'NONE', #6766, #22598, #12734, .T. ) ;
#7199 = DIRECTION ( 'NONE',  ( 0.3090169943749475623, 8.338696094058001131E-17, 0.9510565162951536422 ) ) ;
#7200 = EDGE_CURVE ( 'NONE', #25128, #23660, #12881, .T. ) ;
#7201 = EDGE_CURVE ( 'NONE', #5593, #29734, #3305, .T. ) ;
#7202 = EDGE_CURVE ( 'NONE', #983, #17128, #5733, .T. ) ;
#7203 = CARTESIAN_POINT ( 'NONE',  ( 34.21937970685856101, -11.80343312934236089, -19.83772509046166732 ) ) ;
#7204 = CARTESIAN_POINT ( 'NONE',  ( 0.000000000000000000, 0.000000000000000000, 0.000000000000000000 ) ) ;
#7205 = CARTESIAN_POINT ( 'NONE',  ( 16.27660620799252911, 9.202420196601492464, -13.74949690087879439 ) ) ;
#7206 = CARTESIAN_POINT ( 'NONE',  ( 13.77718166750866224, 8.859676595473322536, -15.39100258941132715 ) ) ;
#7207 = VECTOR ( 'NONE', #10207, 999.9999999999998863 ) ;
#7208 = ORIENTED_EDGE ( 'NONE', *, *, #9204, .T. ) ;
#7209 = DIRECTION ( 'NONE',  ( -0.5877852522924731371, 0.000000000000000000, 0.8090169943749474513 ) ) ;
#7210 = CIRCLE ( 'NONE', #10130, 7.000000000000006217 ) ;
#7211 = ORIENTED_EDGE ( 'NONE', *, *, #18721, .T. ) ;
#7212 = CARTESIAN_POINT ( 'NONE',  ( 0.000000000000000000, 0.000000000000000000, 4.999999999999998224 ) ) ;
#7213 = VECTOR ( 'NONE', #19545, 1000.000000000000000 ) ;
#7214 = DIRECTION ( 'NONE',  ( -0.5877852522924731371, -1.586114251531760235E-16, 0.8090169943749474513 ) ) ;
#7215 = DIRECTION ( 'NONE',  ( 1.000000000000000000, 2.698458740408365879E-16, -1.110223024625156540E-16 ) ) ;
#7216 = CARTESIAN_POINT ( 'NONE',  ( 10.72113683966407294, 16.62961142682532767, -15.95405668885543982 ) ) ;
#7217 = CARTESIAN_POINT ( 'NONE',  ( 139.7287565553230309, -1.999999999999978684, -25.16025403784439973 ) ) ;
#7218 = ORIENTED_EDGE ( 'NONE', *, *, #4327, .F. ) ;
#7219 = LINE ( 'NONE', #23542, #15381 ) ;
#7220 = ORIENTED_EDGE ( 'NONE', *, *, #14443, .T. ) ;
#7221 = CARTESIAN_POINT ( 'NONE',  ( 9.917205744531459644, 16.40378525026516243, -16.50423678068149869 ) ) ;
#7222 = VERTEX_POINT ( 'NONE', #7714 ) ;
#7223 = AXIS2_PLACEMENT_3D ( 'NONE', #29606, #8767, #4353 ) ;
#7224 = CARTESIAN_POINT ( 'NONE',  ( 16.31265859067239532, 4.319332383768222705, -17.78589364095596892 ) ) ;
#7225 = CARTESIAN_POINT ( 'NONE',  ( 2.100000000000000977, 9.325873406851313362E-16, -2.450000000000000178 ) ) ;
#7226 = DIRECTION ( 'NONE',  ( 0.000000000000000000, -0.000000000000000000, 1.000000000000000000 ) ) ;
#7227 = CARTESIAN_POINT ( 'NONE',  ( 28.15048769591263067, -5.842385520647848551, -16.89978903947823241 ) ) ;
#7228 = VERTEX_POINT ( 'NONE', #19454 ) ;
#7229 = CARTESIAN_POINT ( 'NONE',  ( 138.6922820468854525, -1.999999999999979572, -17.92658477444275533 ) ) ;
#7230 = CARTESIAN_POINT ( 'NONE',  ( 11.27662090294977837, 16.67494637447927275, -16.78434760121053060 ) ) ;
#7231 = VERTEX_POINT ( 'NONE', #10596 ) ;
#7232 = AXIS2_PLACEMENT_3D ( 'NONE', #17835, #22741, #1854 ) ;
#7233 = CARTESIAN_POINT ( 'NONE',  ( 33.19002920664139111, -11.78337016499817658, -17.90800870513906773 ) ) ;
#7234 = DIRECTION ( 'NONE',  ( -0.9510565162951536422, -2.566386769018988323E-16, 0.3090169943749475623 ) ) ;
#7235 = ADVANCED_FACE ( 'NONE', ( #17023 ), #28514, .F. ) ;
#7236 = DIRECTION ( 'NONE',  ( -0.8090169943749474513, -2.183098979609982436E-16, 0.5877852522924731371 ) ) ;
#7237 = CARTESIAN_POINT ( 'NONE',  ( 23.31581686446907398, -5.989474659622321617, -13.63887547363156827 ) ) ;
#7238 = ADVANCED_FACE ( 'NONE', ( #26198 ), #3007, .T. ) ;
#7239 = EDGE_LOOP ( 'NONE', ( #9386, #2785, #25854, #20739 ) ) ;
#7240 = EDGE_CURVE ( 'NONE', #10075, #16811, #4186, .T. ) ;
#7241 = CARTESIAN_POINT ( 'NONE',  ( 0.000000000000000000, 0.000000000000000000, 23.00000000000000000 ) ) ;
#7242 = CARTESIAN_POINT ( 'NONE',  ( 16.95656709563420250, 3.789241241613106048, -19.64973185778705655 ) ) ;
#7243 = CARTESIAN_POINT ( 'NONE',  ( 17.65249788084269511, 8.387921445357553907, -19.05198057976592452 ) ) ;
#7244 = EDGE_LOOP ( 'NONE', ( #6040, #6141, #1950, #14525, #22457 ) ) ;
#7245 = VERTEX_POINT ( 'NONE', #1759 ) ;
#7246 = CARTESIAN_POINT ( 'NONE',  ( 154.7287565553229456, -1.999999999999974909, -7.839745962155603820 ) ) ;
#7247 = VECTOR ( 'NONE', #7923, 1000.000000000000000 ) ;
#7248 = DIRECTION ( 'NONE',  ( 0.5877852522924731371, 0.000000000000000000, 0.8090169943749474513 ) ) ;
#7249 = CARTESIAN_POINT ( 'NONE',  ( 8.000000000000010658, 4.618802153517005848, -5.000000000000000888 ) ) ;
#7250 = AXIS2_PLACEMENT_3D ( 'NONE', #28650, #1294, #5872 ) ;
#7251 = CARTESIAN_POINT ( 'NONE',  ( 139.7287565553230309, -10.00000000000000533, -7.839745962155603820 ) ) ;
#7252 = CARTESIAN_POINT ( 'NONE',  ( 4.000000000000001776, 1.776356839400249676E-15, 9.480888224575629408 ) ) ;
#7253 = CARTESIAN_POINT ( 'NONE',  ( 9.641350810849047548, 17.66889113945805789, -17.91752729848689185 ) ) ;
#7254 = CIRCLE ( 'NONE', #9169, 8.000000000000000000 ) ;
#7255 = CARTESIAN_POINT ( 'NONE',  ( 20.69116929084294298, -5.269815114589342819, -18.46063674707264468 ) ) ;
#7256 = CARTESIAN_POINT ( 'NONE',  ( 20.55949567978923298, 1.660703385868308235, -14.27713627412184039 ) ) ;
#7257 = ADVANCED_FACE ( 'NONE', ( #27116 ), #25096, .T. ) ;
#7258 = CARTESIAN_POINT ( 'NONE',  ( 36.54859390953724585, -23.18451583373416014, -17.22552805718784441 ) ) ;
#7259 = DIRECTION ( 'NONE',  ( -2.207829878515935943E-16, -1.000000000000000000, 0.000000000000000000 ) ) ;
#7260 = FACE_OUTER_BOUND ( 'NONE', #22754, .T. ) ;
#7261 = LINE ( 'NONE', #16560, #6349 ) ;
#7262 = CARTESIAN_POINT ( 'NONE',  ( 19.25048709941964376, 7.441878894999256921, -18.84525011105569803 ) ) ;
#7263 = DIRECTION ( 'NONE',  ( -2.698458740408365879E-16, 1.000000000000000000, 0.000000000000000000 ) ) ;
#7264 = CARTESIAN_POINT ( 'NONE',  ( 10.33811767156285555, 18.38618615532545064, -17.91197029530843565 ) ) ;
#7265 = VERTEX_POINT ( 'NONE', #11048 ) ;
#7266 = DIRECTION ( 'NONE',  ( -6.938893903907227392E-16, 0.000000000000000000, -1.000000000000000000 ) ) ;
#7267 = FACE_OUTER_BOUND ( 'NONE', #14179, .T. ) ;
#7268 = CARTESIAN_POINT ( 'NONE',  ( 16.57956996521092918, 4.788269978297743812, -19.71382457362092566 ) ) ;
#7269 = VERTEX_POINT ( 'NONE', #10892 ) ;
#7270 = CARTESIAN_POINT ( 'NONE',  ( 17.86674704105132605, 10.80914456302241788, -19.54358591003751755 ) ) ;
#7271 = ORIENTED_EDGE ( 'NONE', *, *, #23516, .T. ) ;
#7272 = CARTESIAN_POINT ( 'NONE',  ( 34.39741479528305490, -17.01287786994462792, -20.00997473120332515 ) ) ;
#7273 = AXIS2_PLACEMENT_3D ( 'NONE', #13315, #6458, #45 ) ;
#7274 = CARTESIAN_POINT ( 'NONE',  ( 23.28032035799162358, -0.8411909528121862545, -14.99295998388115869 ) ) ;
#7275 = CARTESIAN_POINT ( 'NONE',  ( 18.98834166481877972, 4.258514017552020192, -15.11364409576566459 ) ) ;
#7276 = VECTOR ( 'NONE', #19878, 1000.000000000000000 ) ;
#7277 = CARTESIAN_POINT ( 'NONE',  ( 29.37945295281542712, -10.41679561567529433, -17.92877087918597212 ) ) ;
#7278 = AXIS2_PLACEMENT_3D ( 'NONE', #974, #29399, #1129 ) ;
#7279 = EDGE_LOOP ( 'NONE', ( #23506, #14766, #26885, #7091 ) ) ;
#7280 = CARTESIAN_POINT ( 'NONE',  ( 133.7287565553229172, -4.999999999999982236, -36.50000000000000711 ) ) ;
#7281 = CARTESIAN_POINT ( 'NONE',  ( 159.7287565553229456, -1.999999999999973133, -16.50000000000000355 ) ) ;
#7282 = ORIENTED_EDGE ( 'NONE', *, *, #15931, .F. ) ;
#7283 = CARTESIAN_POINT ( 'NONE',  ( 173.6922820468853388, -9.999999999999994671, -23.73366926340167637 ) ) ;
#7284 = DIRECTION ( 'NONE',  ( 1.000000000000000000, 0.000000000000000000, -0.000000000000000000 ) ) ;
#7285 = ADVANCED_FACE ( 'NONE', ( #4040 ), #17612, .T. ) ;
#7286 = CARTESIAN_POINT ( 'NONE',  ( 36.35319451023849524, -20.30668983862152288, -19.44923342519521370 ) ) ;
#7287 = CARTESIAN_POINT ( 'NONE',  ( 9.641351021852148762, 17.66889017177091503, -17.91406276888456617 ) ) ;
#7288 = ADVANCED_FACE ( 'NONE', ( #22812 ), #2063, .T. ) ;
#7289 = ORIENTED_EDGE ( 'NONE', *, *, #6644, .F. ) ;
#7290 = PLANE ( 'NONE',  #20997 ) ;
#7291 = CARTESIAN_POINT ( 'NONE',  ( 114.0813507336719255, -4.999999999999986677, -82.88495296030824022 ) ) ;
#7292 = CARTESIAN_POINT ( 'NONE',  ( 12.03309083968702886, 9.293808706017943067, -16.68917936036902105 ) ) ;
#7293 = CARTESIAN_POINT ( 'NONE',  ( 153.6922820468854241, -1.999999999999975353, -32.39392330124607611 ) ) ;
#7294 = AXIS2_PLACEMENT_3D ( 'NONE', #29796, #27477, #6684 ) ;
#7295 = ORIENTED_EDGE ( 'NONE', *, *, #7370, .F. ) ;
#7296 = CARTESIAN_POINT ( 'NONE',  ( 3.999999999999999112, 0.7862748000878193588, -2.415527722372434738 ) ) ;
#7297 = ORIENTED_EDGE ( 'NONE', *, *, #6265, .T. ) ;
#7298 = FACE_OUTER_BOUND ( 'NONE', #19832, .T. ) ;
#7299 = DIRECTION ( 'NONE',  ( 1.000000000000000000, 2.698458740408365879E-16, -1.110223024625156540E-16 ) ) ;
#7300 = CARTESIAN_POINT ( 'NONE',  ( 175.7287565553229456, -4.999999999999970690, -4.785595155761523500 ) ) ;
#7301 = EDGE_LOOP ( 'NONE', ( #10063, #5825, #25193, #17553, #18197, #8967 ) ) ;
#7302 = CARTESIAN_POINT ( 'NONE',  ( 9.668378799564367299, 16.22503635135577227, -17.88486489230207965 ) ) ;
#7303 = CARTESIAN_POINT ( 'NONE',  ( 24.88525782559502630, -5.606924519715485111, -13.99218633471889817 ) ) ;
#7304 = CARTESIAN_POINT ( 'NONE',  ( 21.12965431673027794, -4.223434333162931154, -14.75790768142083031 ) ) ;
#7305 = DIRECTION ( 'NONE',  ( -1.000000000000000000, -2.698458740408365879E-16, -0.000000000000000000 ) ) ;
#7306 = PLANE ( 'NONE',  #27742 ) ;
#7307 = DIRECTION ( 'NONE',  ( -0.5877852522924731371, -1.586114251531760235E-16, 0.8090169943749474513 ) ) ;
#7308 = LINE ( 'NONE', #2737, #2067 ) ;
#7309 = AXIS2_PLACEMENT_3D ( 'NONE', #16750, #1337, #3772 ) ;
#7310 = CARTESIAN_POINT ( 'NONE',  ( 23.84106988684860440, -4.080291168153947545, -13.50610408985603250 ) ) ;
#7311 = ORIENTED_EDGE ( 'NONE', *, *, #10104, .F. ) ;
#7312 = VECTOR ( 'NONE', #11846, 1000.000000000000000 ) ;
#7313 = DIRECTION ( 'NONE',  ( -0.5877852522924731371, -1.586114251531760728E-16, -0.8090169943749474513 ) ) ;
#7314 = DIRECTION ( 'NONE',  ( -2.698458740408366372E-16, 1.000000000000000000, 0.000000000000000000 ) ) ;
#7315 = CARTESIAN_POINT ( 'NONE',  ( 175.7287565553229456, -4.999999999999970690, -10.89389676854971967 ) ) ;
#7316 = LINE ( 'NONE', #1, #11716 ) ;
#7317 = LINE ( 'NONE', #4719, #1670 ) ;
#7318 = VECTOR ( 'NONE', #5875, 1000.000000000000000 ) ;
#7319 = CARTESIAN_POINT ( 'NONE',  ( 10.47401950373780899, 16.44302204293020964, -17.33397781699859053 ) ) ;
#7320 = EDGE_CURVE ( 'NONE', #9337, #4351, #25890, .T. ) ;
#7321 = EDGE_CURVE ( 'NONE', #11139, #29174, #6482, .T. ) ;
#7322 = FACE_OUTER_BOUND ( 'NONE', #5935, .T. ) ;
#7323 = CARTESIAN_POINT ( 'NONE',  ( 167.0152310637604955, -1.999999999999970912, -26.04193191628311155 ) ) ;
#7324 = ORIENTED_EDGE ( 'NONE', *, *, #5043, .T. ) ;
#7325 = CIRCLE ( 'NONE', #27350, 13.00000000000000178 ) ;
#7326 = CARTESIAN_POINT ( 'NONE',  ( 8.944584683310379702, 16.95159276115599667, -17.95086732675816776 ) ) ;
#7327 = ADVANCED_FACE ( 'NONE', ( #1614, #11194 ), #13632, .T. ) ;
#7328 = VERTEX_POINT ( 'NONE', #20059 ) ;
#7329 = CARTESIAN_POINT ( 'NONE',  ( 177.2287565553228887, -9.999999999999994671, -20.83012701892220520 ) ) ;
#7330 = ADVANCED_FACE ( 'NONE', ( #29271 ), #29433, .T. ) ;
#7331 = CARTESIAN_POINT ( 'NONE',  ( 18.21616227284554057, 4.699354889203569918, -13.86658597208997179 ) ) ;
#7332 = CARTESIAN_POINT ( 'NONE',  ( 11.27425361364269563, 16.68580306500076915, -16.78535843524344173 ) ) ;
#7333 = FACE_BOUND ( 'NONE', #8697, .T. ) ;
#7334 = VERTEX_POINT ( 'NONE', #13192 ) ;
#7335 = AXIS2_PLACEMENT_3D ( 'NONE', #14968, #7963, #24016 ) ;
#7336 = ORIENTED_EDGE ( 'NONE', *, *, #21344, .T. ) ;
#7337 = CARTESIAN_POINT ( 'NONE',  ( 9.655099948573186097, 17.60583584124798051, -17.48406748397995614 ) ) ;
#7338 = LINE ( 'NONE', #16637, #23297 ) ;
#7339 = CARTESIAN_POINT ( 'NONE',  ( 9.644802874473198173, 17.65305953564175567, -17.69767226479352118 ) ) ;
#7340 = CARTESIAN_POINT ( 'NONE',  ( 138.6922820468854241, -1.999999999999979572, -15.07341522555727309 ) ) ;
#7341 = VERTEX_POINT ( 'NONE', #8898 ) ;
#7342 = PLANE ( 'NONE',  #4712 ) ;
#7343 = ORIENTED_EDGE ( 'NONE', *, *, #27360, .T. ) ;
#7344 = CARTESIAN_POINT ( 'NONE',  ( 10.47103768343372288, 16.45669705093847313, -17.33522727542475295 ) ) ;
#7345 = VERTEX_POINT ( 'NONE', #22514 ) ;
#7346 = CARTESIAN_POINT ( 'NONE',  ( 36.52322468491136220, -22.07054534594105988, -19.04503427665075321 ) ) ;
#7347 = CARTESIAN_POINT ( 'NONE',  ( 26.36224721256908410, -8.875037662531589433, -13.49479840426202948 ) ) ;
#7348 = CARTESIAN_POINT ( 'NONE',  ( 16.68567729567724456, 11.07888045854852876, -16.17353378320854418 ) ) ;
#7349 = ORIENTED_EDGE ( 'NONE', *, *, #62, .F. ) ;
#7350 = DIRECTION ( 'NONE',  ( 0.5877852522924731371, 0.000000000000000000, 0.8090169943749474513 ) ) ;
#7351 = DIRECTION ( 'NONE',  ( -0.8090169943749474513, -2.183098979609982436E-16, 0.5877852522924731371 ) ) ;
#7352 = AXIS2_PLACEMENT_3D ( 'NONE', #24691, #21628, #10472 ) ;
#7353 = CARTESIAN_POINT ( 'NONE',  ( -20.00000000000015632, 34.64101615137746393, -2.450000000000000622 ) ) ;
#7354 = CARTESIAN_POINT ( 'NONE',  ( 26.46413748225140594, -13.10274310649288942, -15.24000415025259692 ) ) ;
#7355 = AXIS2_PLACEMENT_3D ( 'NONE', #29384, #26919, #5981 ) ;
#7356 = CARTESIAN_POINT ( 'NONE',  ( 28.00362220295478721, -7.540254448315821811, -17.98007619878529439 ) ) ;
#7357 = ORIENTED_EDGE ( 'NONE', *, *, #25373, .T. ) ;
#7358 = VERTEX_POINT ( 'NONE', #18214 ) ;
#7359 = FACE_BOUND ( 'NONE', #22663, .T. ) ;
#7360 = AXIS2_PLACEMENT_3D ( 'NONE', #24100, #3203, #21805 ) ;
#7361 = DIRECTION ( 'NONE',  ( -1.110223024625156540E-16, 0.000000000000000000, -1.000000000000000000 ) ) ;
#7362 = CARTESIAN_POINT ( 'NONE',  ( 420.0000000000002274, 27.64101615137744972, 14.00000000000000178 ) ) ;
#7363 = DIRECTION ( 'NONE',  ( -2.698458740408365879E-16, 1.000000000000000000, 0.000000000000000000 ) ) ;
#7364 = EDGE_CURVE ( 'NONE', #19492, #29780, #13040, .T. ) ;
#7365 = FACE_OUTER_BOUND ( 'NONE', #30006, .T. ) ;
#7366 = UNCERTAINTY_MEASURE_WITH_UNIT (LENGTH_MEASURE( 1.000000000000000082E-05 ), #25150, 'distance_accuracy_value', 'NONE');
#7367 = EDGE_CURVE ( 'NONE', #18794, #27442, #20202, .T. ) ;
#7368 = ADVANCED_FACE ( 'NONE', ( #8306, #8601, #20350 ), #17901, .F. ) ;
#7369 = CARTESIAN_POINT ( 'NONE',  ( 10.33811712360892443, 18.38618866831204102, -17.91390369733608523 ) ) ;
#7370 = EDGE_CURVE ( 'NONE', #5507, #13972, #27427, .T. ) ;
#7372 = AXIS2_PLACEMENT_3D ( 'NONE', #27783, #16592, #25917 ) ;
#7371 = CARTESIAN_POINT ( 'NONE',  ( 0.000000000000000000, 55.00000000000000711, -18.00000000000000000 ) ) ;
#7373 = CARTESIAN_POINT ( 'NONE',  ( 172.2287565553229740, -4.999999999999970690, -29.49038105676660138 ) ) ;
#7374 = EDGE_LOOP ( 'NONE', ( #21615, #12842, #2058, #7766, #17510 ) ) ;
#7375 = AXIS2_PLACEMENT_3D ( 'NONE', #401, #9686, #16570 ) ;
#7376 = CARTESIAN_POINT ( 'NONE',  ( 9.957223259857686415, 16.22025982393231303, -16.48768813039480818 ) ) ;
#7377 = VERTEX_POINT ( 'NONE', #13924 ) ;
#7378 = CARTESIAN_POINT ( 'NONE',  ( 9.667856465286563505, 16.22743184293591057, -17.88508098240584587 ) ) ;
#7379 = CARTESIAN_POINT ( 'NONE',  ( 17.47084574460127371, 4.633898707001591788, -15.02533140066315198 ) ) ;
#7380 = DIRECTION ( 'NONE',  ( 0.000000000000000000, 0.000000000000000000, 1.000000000000000000 ) ) ;
#7381 = CARTESIAN_POINT ( 'NONE',  ( 171.1922820468853388, -4.999999999999971578, -22.25671179336496053 ) ) ;
#7382 = CARTESIAN_POINT ( 'NONE',  ( 27.20760296572909809, -8.488227175050779394, -13.35743234967312354 ) ) ;
#7383 = VERTEX_POINT ( 'NONE', #25694 ) ;
#7384 = CARTESIAN_POINT ( 'NONE',  ( 132.0152310637605808, -1.999999999999981348, -15.61832212156129351 ) ) ;
#7385 = CARTESIAN_POINT ( 'NONE',  ( 11.05545861061968083, 17.68922483874021978, -17.89384690447096560 ) ) ;
#7386 = ORIENTED_EDGE ( 'NONE', *, *, #26607, .T. ) ;
#7387 = CARTESIAN_POINT ( 'NONE',  ( 33.63121621376239290, -12.57075016180469262, -18.73605167971255980 ) ) ;
#7388 = CARTESIAN_POINT ( 'NONE',  ( 16.53304876882650731, 8.555045913257369961, -19.77053526944897754 ) ) ;
#7389 = FACE_OUTER_BOUND ( 'NONE', #25598, .T. ) ;
#7390 = CARTESIAN_POINT ( 'NONE',  ( 9.113211330545484046, 16.17824946203780456, -17.05444305708079966 ) ) ;
#7391 = CARTESIAN_POINT ( 'NONE',  ( 25.62874891556376511, -2.832145142407604510, -18.00902499482074148 ) ) ;
#7392 = EDGE_LOOP ( 'NONE', ( #8815, #16678 ) ) ;
#7393 = LINE ( 'NONE', #3125, #8128 ) ;
#7394 = CARTESIAN_POINT ( 'NONE',  ( 20.07445496384854877, 6.874260549971754841, -18.87959640166664954 ) ) ;
#7395 = CARTESIAN_POINT ( 'NONE',  ( 18.99253871878172717, 7.061292173911923875, -17.66947577672478431 ) ) ;
#7396 = ORIENTED_EDGE ( 'NONE', *, *, #29401, .F. ) ;
#7397 = FACE_OUTER_BOUND ( 'NONE', #19366, .T. ) ;
#7398 = ORIENTED_EDGE ( 'NONE', *, *, #26644, .F. ) ;
#7399 = EDGE_CURVE ( 'NONE', #24599, #17207, #23256, .T. ) ;
#7400 = LINE ( 'NONE', #16697, #8390 ) ;
#7401 = VECTOR ( 'NONE', #16248, 1000.000000000000000 ) ;
#7402 = CARTESIAN_POINT ( 'NONE',  ( 131.1922820468854241, -4.999999999999983125, -4.936203717676158398 ) ) ;
#7403 = DIRECTION ( 'NONE',  ( 0.000000000000000000, 0.000000000000000000, 1.000000000000000000 ) ) ;
#7404 = FACE_OUTER_BOUND ( 'NONE', #29379, .T. ) ;
#7405 = EDGE_CURVE ( 'NONE', #7041, #13256, #368, .T. ) ;
#7406 = DIRECTION ( 'NONE',  ( 0.9510565162951536422, 2.566386769018988816E-16, 0.3090169943749472292 ) ) ;
#7407 = EDGE_CURVE ( 'NONE', #13148, #11753, #25541, .T. ) ;
#7408 = CARTESIAN_POINT ( 'NONE',  ( 9.641351654859628084, 17.66888726871794191, -17.91235298298990841 ) ) ;
#7409 = ADVANCED_FACE ( 'NONE', ( #11485 ), #23558, .T. ) ;
#7410 = CARTESIAN_POINT ( 'NONE',  ( 27.16844481176636350, -11.11852963900163438, -17.34443814838110143 ) ) ;
#7411 = CARTESIAN_POINT ( 'NONE',  ( 20.75491211191951635, -1.144232541536293946, -14.27023797479654554 ) ) ;
#7413 = EDGE_LOOP ( 'NONE', ( #15394, #416, #26312, #21551, #27796 ) ) ;
#7412 = CARTESIAN_POINT ( 'NONE',  ( 33.15841575409167064, -12.44672528413413026, -20.67776857359057274 ) ) ;
#7414 = CARTESIAN_POINT ( 'NONE',  ( 63.44486372867149981, -20.00000000000000355, -15.00000000000000000 ) ) ;
#7415 = LINE ( 'NONE', #5268, #12124 ) ;
#7416 = LINE ( 'NONE', #16403, #17118 ) ;
#7417 = LINE ( 'NONE', #14557, #9015 ) ;
#7418 = CARTESIAN_POINT ( 'NONE',  ( 14.24706144987486667, 6.238427219560604087, -16.72753349211556184 ) ) ;
#7419 = EDGE_LOOP ( 'NONE', ( #23951, #20869, #23705, #11223, #18022 ) ) ;
#7420 = CARTESIAN_POINT ( 'NONE',  ( 143.6922820468854241, -10.00000000000000355, -9.266330736598359152 ) ) ;
#7421 = CARTESIAN_POINT ( 'NONE',  ( 10.38540050948072846, 18.16934103347302454, -16.97553146008864289 ) ) ;
#7422 = CARTESIAN_POINT ( 'NONE',  ( 139.5152310637605808, -1.999999999999978684, -13.05155085951651195 ) ) ;
#7423 = DIRECTION ( 'NONE',  ( -0.9510565162951536422, -2.566386769018988816E-16, -0.3090169943749472292 ) ) ;
#7424 = CARTESIAN_POINT ( 'NONE',  ( 14.73401617531889229, 6.408058468588501810, -15.60580005407095960 ) ) ;
#7425 = CARTESIAN_POINT ( 'NONE',  ( 30.75621536574076487, -10.42133643238263829, -12.14063830390948517 ) ) ;
#7426 = VERTEX_POINT ( 'NONE', #16071 ) ;
#7427 = CARTESIAN_POINT ( 'NONE',  ( 32.89062095351589932, -11.25267498498577723, -18.96775996542842435 ) ) ;
#7428 = CARTESIAN_POINT ( 'NONE',  ( 21.61496389699315657, -3.514534563429178249, -17.40323974765788506 ) ) ;
#7429 = CARTESIAN_POINT ( 'NONE',  ( 18.57704598647189798, -1.039939211366111005, -17.60664924018008293 ) ) ;
#7430 = ORIENTED_EDGE ( 'NONE', *, *, #5489, .T. ) ;
#7431 = CARTESIAN_POINT ( 'NONE',  ( 27.65280983889778810, -8.379432582749632985, -19.23476105915534973 ) ) ;
#7432 = ORIENTED_EDGE ( 'NONE', *, *, #16445, .F. ) ;
#7433 = VECTOR ( 'NONE', #27364, 1000.000000000000000 ) ;
#7434 = ORIENTED_EDGE ( 'NONE', *, *, #16179, .F. ) ;
#7435 = B_SPLINE_CURVE_WITH_KNOTS ( 'NONE', 3,
 ( #1438, #15454, #22490, #10270, #17295, #24476 ),
 .UNSPECIFIED., .F., .F.,
 ( 4, 2, 4 ),
 ( 0.008240550023493518894, 0.01057684187039405199, 0.01291313371729458509 ),
 .UNSPECIFIED. ) ;
#7436 = LINE ( 'NONE', #14578, #5021 ) ;
#7437 = DIRECTION ( 'NONE',  ( -0.9510565162951536422, 0.000000000000000000, -0.3090169943749472292 ) ) ;
#7438 = CARTESIAN_POINT ( 'NONE',  ( 159.7287565553229172, -10.00000000000000000, -7.839745962155603820 ) ) ;
#7439 = EDGE_CURVE ( 'NONE', #23755, #15731, #25399, .T. ) ;
#7440 = CARTESIAN_POINT ( 'NONE',  ( 141.1922820468854241, -1.999999999999978684, -2.083034168790677043 ) ) ;
#7441 = CARTESIAN_POINT ( 'NONE',  ( 36.53496835490201988, -21.12330343441383818, -18.71787618725911884 ) ) ;
#7442 = CARTESIAN_POINT ( 'NONE',  ( 9.643509238790151983, 17.65899231378470446, -17.74106871770035099 ) ) ;
#7443 = ORIENTED_EDGE ( 'NONE', *, *, #22242, .T. ) ;
#7444 = DIRECTION ( 'NONE',  ( -0.5877852522924731371, 0.000000000000000000, 0.8090169943749474513 ) ) ;
#7445 = DIRECTION ( 'NONE',  ( 0.3090169943749475623, 8.338696094058001131E-17, 0.9510565162951536422 ) ) ;
#7446 = CARTESIAN_POINT ( 'NONE',  ( 12.50603416232391929, 8.608717614871036261, -16.38042650914619358 ) ) ;
#7447 = CARTESIAN_POINT ( 'NONE',  ( 116.0854136719178200, -4.999999999999985789, -84.34098991374325749 ) ) ;
#7448 = DIRECTION ( 'NONE',  ( -0.9510565162951536422, -2.566386769018988323E-16, 0.3090169943749475623 ) ) ;
#7449 = ORIENTED_EDGE ( 'NONE', *, *, #9684, .F. ) ;
#7450 = DIRECTION ( 'NONE',  ( -1.000000000000000000, 0.000000000000000000, 0.000000000000000000 ) ) ;
#7452 = VERTEX_POINT ( 'NONE', #2659 ) ;
#7451 = VECTOR ( 'NONE', #14383, 1000.000000000000000 ) ;
#7453 = EDGE_LOOP ( 'NONE', ( #16835, #23521, #10468, #26752 ) ) ;
#7454 = PLANE ( 'NONE',  #19842 ) ;
#7455 = ORIENTED_EDGE ( 'NONE', *, *, #24913, .T. ) ;
#7456 = CARTESIAN_POINT ( 'NONE',  ( 11.18347232286468440, 9.276624323996792043, -17.25832042385608389 ) ) ;
#7457 = CARTESIAN_POINT ( 'NONE',  ( 23.39779239333391914, -5.936415184958717894, -17.60678703246490429 ) ) ;
#7458 = CARTESIAN_POINT ( 'NONE',  ( 20.61437924707763258, -4.384239709691692966, -16.09784705243023240 ) ) ;
#7459 = CARTESIAN_POINT ( 'NONE',  ( 24.19664217352669766, -5.000000000000010658, -74.46960727238361244 ) ) ;
#7460 = CARTESIAN_POINT ( 'NONE',  ( 173.6922820468853672, -1.999999999999969358, -35.24709285013155835 ) ) ;
#7461 = FACE_OUTER_BOUND ( 'NONE', #13404, .T. ) ;
#7462 = ADVANCED_FACE ( 'NONE', ( #25857 ), #18079, .T. ) ;
#7463 = CARTESIAN_POINT ( 'NONE',  ( 164.7287565553229172, -9.999999999999998224, -16.50000000000000355 ) ) ;
#7464 = CARTESIAN_POINT ( 'NONE',  ( 5.000000000000000000, 6.123233995736766282E-16, -18.00000000000000000 ) ) ;
#7465 = B_SPLINE_CURVE_WITH_KNOTS ( 'NONE', 3,
 ( #11349, #4790, #4639, #16076, #4494, #14080 ),
 .UNSPECIFIED., .F., .F.,
 ( 4, 2, 4 ),
 ( 0.004120275011746841846, 0.005288420935197130079, 0.006456566858647419180 ),
 .UNSPECIFIED. ) ;
#7466 = FACE_BOUND ( 'NONE', #8430, .T. ) ;
#7467 = CARTESIAN_POINT ( 'NONE',  ( 163.6922820468853104, -4.999999999999973355, -6.413161187712876909 ) ) ;
#7468 = DIRECTION ( 'NONE',  ( 0.000000000000000000, 0.000000000000000000, 1.000000000000000000 ) ) ;
#7469 = VECTOR ( 'NONE', #6387, 1000.000000000000000 ) ;
#7470 = CARTESIAN_POINT ( 'NONE',  ( 10.47325967749744180, 16.44650670292386607, -17.33429203187744250 ) ) ;
#7471 = CARTESIAN_POINT ( 'NONE',  ( 163.6922820468853672, -4.999999999999973355, -23.73366926340167637 ) ) ;
#7472 = CARTESIAN_POINT ( 'NONE',  ( 35.03938282813840743, -19.89690018161999419, -20.20402626681843117 ) ) ;
#7473 = VERTEX_POINT ( 'NONE', #18974 ) ;
#7474 = CARTESIAN_POINT ( 'NONE',  ( 13.38031868501602872, 7.626265983139092874, -15.70730939156535655 ) ) ;
#7475 = LINE ( 'NONE', #19359, #16364 ) ;
#7476 = CARTESIAN_POINT ( 'NONE',  ( 21.19279910686179846, 4.720633506281588510, -19.26595127233560234 ) ) ;
#7477 = CARTESIAN_POINT ( 'NONE',  ( 12.82818608578791064, 9.559270667424515366, -16.14272081857926366 ) ) ;
#7478 = LINE ( 'NONE', #28276, #29795 ) ;
#7479 = ORIENTED_EDGE ( 'NONE', *, *, #9275, .T. ) ;
#7480 = CARTESIAN_POINT ( 'NONE',  ( 11.47395765415086188, 9.264374527449886543, -15.86046114005151075 ) ) ;
#7481 = CARTESIAN_POINT ( 'NONE',  ( 139.5152310637605808, -10.00000000000000533, -30.37205893520530964 ) ) ;
#7482 = CARTESIAN_POINT ( 'NONE',  ( 9.643509238790151983, 17.65899231378470446, -17.74106871770035099 ) ) ;
#7483 = CARTESIAN_POINT ( 'NONE',  ( 137.0152310637605808, -10.00000000000000533, -17.38167787843870826 ) ) ;
#7484 = ORIENTED_EDGE ( 'NONE', *, *, #1630, .T. ) ;
#7485 = CARTESIAN_POINT ( 'NONE',  ( -2.678494666091076226, -3.072372537026388351, -0.03421028094655393509 ) ) ;
#7486 = VERTEX_POINT ( 'NONE', #23108 ) ;
#7487 = CARTESIAN_POINT ( 'NONE',  ( 10.47193650065820592, 16.45257496057443802, -17.33483926051624735 ) ) ;
#7488 = ORIENTED_EDGE ( 'NONE', *, *, #22566, .T. ) ;
#7489 = CARTESIAN_POINT ( 'NONE',  ( 31.73602415849877900, -9.487789691486469223, -15.56998832973926916 ) ) ;
#7490 = CARTESIAN_POINT ( 'NONE',  ( 14.03447742461322534, 10.03307406631979326, -15.27079475659193086 ) ) ;
#7491 = CARTESIAN_POINT ( 'NONE',  ( 14.55381231002303188, 10.26819836692386723, -15.14301692386319331 ) ) ;
#7492 = LINE ( 'NONE', #2932, #12549 ) ;
#7493 = VECTOR ( 'NONE', #22528, 1000.000000000000000 ) ;
#7494 = EDGE_LOOP ( 'NONE', ( #20241, #12259, #4263, #10973 ) ) ;
#7495 = LINE ( 'NONE', #635, #23012 ) ;
#7496 = ITEM_DEFINED_TRANSFORMATION ( 'NONE', 'NONE', #4858,  #13190 ) ;
#7497 = EDGE_CURVE ( 'NONE', #16007, #18552, #18363, .T. ) ;
#7498 = EDGE_CURVE ( 'NONE', #20489, #23153, #16227, .T. ) ;
#7499 = CARTESIAN_POINT ( 'NONE',  ( 19.13053735399196142, -0.4946192386601480084, -18.78456443592403602 ) ) ;
#7500 = ADVANCED_FACE ( 'NONE', ( #28176 ), #4634, .T. ) ;
#7501 = CARTESIAN_POINT ( 'NONE',  ( 29.32553208039167458, -8.962988822949116141, -16.84503999589972523 ) ) ;
#7502 = ADVANCED_FACE ( 'NONE', ( #11935 ), #20655, .T. ) ;
#7503 = FACE_BOUND ( 'NONE', #25300, .T. ) ;
#7504 = DIRECTION ( 'NONE',  ( -0.8090169943749474513, -2.183098979609982436E-16, 0.5877852522924731371 ) ) ;
#7505 = CARTESIAN_POINT ( 'NONE',  ( 168.6922820468852819, -1.999999999999972244, -0.6060766987539614181 ) ) ;
#7506 = CARTESIAN_POINT ( 'NONE',  ( -5.000000000000006217, -2.220446049250313870E-15, -4.974599999999998801 ) ) ;
#7507 = CARTESIAN_POINT ( 'NONE',  ( 149.7287565553229740, -4.999999999999977796, -7.839745962155614478 ) ) ;
#7508 = AXIS2_PLACEMENT_3D ( 'NONE', #24711, #12940, #22413 ) ;
#7509 = CARTESIAN_POINT ( 'NONE',  ( 12.27643783485070372, 9.496802808135052842, -15.31088501640310540 ) ) ;
#7510 = CARTESIAN_POINT ( 'NONE',  ( 132.0152310637605808, -10.00000000000000711, -15.61832212156129351 ) ) ;
#7511 = CARTESIAN_POINT ( 'NONE',  ( 5.637851296924623057E-15, 9.237604307034036566, -0.7145311798163362926 ) ) ;
#7512 = EDGE_LOOP ( 'NONE', ( #26690, #21240, #11293, #26764, #8709 ) ) ;
#7513 = CARTESIAN_POINT ( 'NONE',  ( 11.47029057985033340, 9.281140223223081520, -15.86198156829250117 ) ) ;
#7514 = VERTEX_POINT ( 'NONE', #3601 ) ;
#7515 = CARTESIAN_POINT ( 'NONE',  ( 18.89783927354708837, -1.194421563772924078, -19.46960211947776287 ) ) ;
#7516 = FACE_OUTER_BOUND ( 'NONE', #19751, .T. ) ;
#7517 = LINE ( 'NONE', #9488, #21794 ) ;
#7518 = DIRECTION ( 'NONE',  ( -0.5877852522924731371, 0.000000000000000000, 0.8090169943749474513 ) ) ;
#7519 = ORIENTED_EDGE ( 'NONE', *, *, #22279, .T. ) ;
#7520 = DIRECTION ( 'NONE',  ( -1.000000000000000000, 0.000000000000000000, 0.000000000000000000 ) ) ;
#7521 = CARTESIAN_POINT ( 'NONE',  ( 11.29637638519941589, 16.58434521464408817, -16.77617801436024081 ) ) ;
#7522 = EDGE_LOOP ( 'NONE', ( #5232, #10645, #14926 ) ) ;
#7523 = CARTESIAN_POINT ( 'NONE',  ( 35.50545599541538877, -20.99072003637593653, -18.92103158260024642 ) ) ;
#7524 = CARTESIAN_POINT ( 'NONE',  ( 18.69974902744413470, 8.051839821468062652, -15.50866580261103955 ) ) ;
#7525 = DIRECTION ( 'NONE',  ( 0.3090169943749475623, 8.338696094058001131E-17, 0.9510565162951536422 ) ) ;
#7526 = CARTESIAN_POINT ( 'NONE',  ( 9.128787768473113573, 16.10681393216777835, -17.04800165206417972 ) ) ;
#7527 = CARTESIAN_POINT ( 'NONE',  ( 29.60951380729897764, -9.700310021160106544, -19.83312561509874783 ) ) ;
#7528 = ORIENTED_EDGE ( 'NONE', *, *, #13557, .T. ) ;
#7529 = DIRECTION ( 'NONE',  ( 0.000000000000000000, 0.000000000000000000, 1.000000000000000000 ) ) ;
#7530 = SURFACE_STYLE_FILL_AREA ( #9661 ) ;
#7531 = EDGE_CURVE ( 'NONE', #6950, #23457, #5898, .T. ) ;
#7532 = CARTESIAN_POINT ( 'NONE',  ( 19.92565466131104301, 6.686648131885553958, -19.16379146452587179 ) ) ;
#7533 = EDGE_CURVE ( 'NONE', #16634, #5625, #10453, .T. ) ;
#7534 = CARTESIAN_POINT ( 'NONE',  ( 17.24236049518817282, 9.271217979531970244, -15.28210331290996571 ) ) ;
#7535 = EDGE_CURVE ( 'NONE', #19917, #27081, #19756, .T. ) ;
#7536 = VECTOR ( 'NONE', #9551, 1000.000000000000000 ) ;
#7537 = ORIENTED_EDGE ( 'NONE', *, *, #548, .T. ) ;
#7538 = CARTESIAN_POINT ( 'NONE',  ( -5.000000000000000000, 0.000000000000000000, 18.00000000000000000 ) ) ;
#7539 = EDGE_CURVE ( 'NONE', #16400, #1424, #6967, .T. ) ;
#7540 = EDGE_LOOP ( 'NONE', ( #23721, #23587, #2764, #24605 ) ) ;
#7541 = ORIENTED_EDGE ( 'NONE', *, *, #4465, .F. ) ;
#7542 = DIRECTION ( 'NONE',  ( -1.000000000000000000, -4.440892098500622217E-16, 0.000000000000000000 ) ) ;
#7543 = CARTESIAN_POINT ( 'NONE',  ( 148.6922820468853956, -10.00000000000000178, -9.266330736598359152 ) ) ;
#7544 = ORIENTED_EDGE ( 'NONE', *, *, #26020, .T. ) ;
#7545 = CARTESIAN_POINT ( 'NONE',  ( -4.683753385137379155E-14, -9.237604307034027684, -0.7145311798163362926 ) ) ;
#7546 = LINE ( 'NONE', #28195, #12614 ) ;
#7547 = DIRECTION ( 'NONE',  ( 0.9510565162951536422, 2.566386769018988816E-16, 0.3090169943749472292 ) ) ;
#7548 = CARTESIAN_POINT ( 'NONE',  ( 9.641350835837977584, 17.66889102485563612, -17.91507476468484938 ) ) ;
#7549 = CARTESIAN_POINT ( 'NONE',  ( 26.65048721414892086, -11.67344998524500355, -15.88597958324129777 ) ) ;
#7550 = CARTESIAN_POINT ( 'NONE',  ( 19.39248696316839116, -1.610358169686434193, -16.91126230894791860 ) ) ;
#7552 = ORIENTED_EDGE ( 'NONE', *, *, #10343, .F. ) ;
#7551 = CARTESIAN_POINT ( 'NONE',  ( 34.92716911317440065, -20.39278340154575631, -21.20741747040485592 ) ) ;
#7553 = DIRECTION ( 'NONE',  ( -1.000000000000000000, -1.226925503391459338E-16, -0.000000000000000000 ) ) ;
#7554 = PLANE ( 'NONE',  #29316 ) ;
#7555 = AXIS2_PLACEMENT_3D ( 'NONE', #10082, #26442, #14210 ) ;
#7556 = DIRECTION ( 'NONE',  ( 1.000000000000000000, 0.000000000000000000, 0.000000000000000000 ) ) ;
#7557 = LINE ( 'NONE', #3001, #27603 ) ;
#7558 = CARTESIAN_POINT ( 'NONE',  ( 16.34386185847872142, 4.569898679961749366, -19.52586945278800812 ) ) ;
#7559 = ORIENTED_EDGE ( 'NONE', *, *, #14772, .F. ) ;
#7560 = DIRECTION ( 'NONE',  ( -2.698458740408365879E-16, 1.000000000000000000, 0.000000000000000000 ) ) ;
#7561 = CARTESIAN_POINT ( 'NONE',  ( 10.41323547201801958, 18.04168634714536168, -16.76531574090561350 ) ) ;
#7562 = DIRECTION ( 'NONE',  ( 1.000000000000000000, 0.000000000000000000, 0.000000000000000000 ) ) ;
#7563 = CARTESIAN_POINT ( 'NONE',  ( -24.99999999999998934, 60.00000000000000711, 29.99999999999999289 ) ) ;
#7564 = CARTESIAN_POINT ( 'NONE',  ( 19.25048709941964376, 7.441878894999256921, -18.84525011105569803 ) ) ;
#7565 = CARTESIAN_POINT ( 'NONE',  ( 25.64452216564459164, -12.66255397501067570, -13.70049860994083701 ) ) ;
#7566 = ORIENTED_EDGE ( 'NONE', *, *, #9277, .F. ) ;
#7567 = CARTESIAN_POINT ( 'NONE',  ( 35.16668739017224965, -20.46881214373840763, -20.22602438870426766 ) ) ;
#7568 = CARTESIAN_POINT ( 'NONE',  ( 21.82606822486871323, 1.157895394498012154, -14.17951425939655508 ) ) ;
#7569 = EDGE_CURVE ( 'NONE', #12418, #8151, #29282, .T. ) ;
#7570 = CARTESIAN_POINT ( 'NONE',  ( 16.83868323617221208, 3.350830693655540315, -16.91447790370928672 ) ) ;
#7571 = EDGE_CURVE ( 'NONE', #17394, #11963, #17626, .T. ) ;
#7572 = EDGE_CURVE ( 'NONE', #5536, #14016, #27438, .T. ) ;
#7573 = EDGE_CURVE ( 'NONE', #18112, #6899, #15321, .T. ) ;
#7574 = CARTESIAN_POINT ( 'NONE',  ( 29.25075025305862653, -5.797754334661411768, -14.89650002867986878 ) ) ;
#7575 = TOROIDAL_SURFACE ( 'NONE', #15837, 4.000000000000000000, 0.2500000000000000000 ) ;
#7576 = EDGE_LOOP ( 'NONE', ( #26297, #12404, #9246, #17697 ) ) ;
#7577 = DIRECTION ( 'NONE',  ( -0.5877852522924731371, 0.000000000000000000, 0.8090169943749474513 ) ) ;
#7578 = DIRECTION ( 'NONE',  ( 0.000000000000000000, 0.000000000000000000, 1.000000000000000000 ) ) ;
#7579 = CARTESIAN_POINT ( 'NONE',  ( 164.7287565553229172, -1.999999999999971800, -16.50000000000000355 ) ) ;
#7580 = FACE_OUTER_BOUND ( 'NONE', #27334, .T. ) ;
#7581 = VECTOR ( 'NONE', #9374, 1000.000000000000000 ) ;
#7582 = CARTESIAN_POINT ( 'NONE',  ( 33.68917633736438688, -10.64779379647620949, -18.96437360758372748 ) ) ;
#7583 = CARTESIAN_POINT ( 'NONE',  ( 9.641350810849047548, 17.66889113945805789, -17.98596209335946128 ) ) ;
#7584 = VECTOR ( 'NONE', #1681, 1000.000000000000000 ) ;
#7585 = PLANE ( 'NONE',  #27392 ) ;
#7586 = CARTESIAN_POINT ( 'NONE',  ( 159.5152310637604387, -4.999999999999974243, -1.770974823053888411E-14 ) ) ;
#7587 = CARTESIAN_POINT ( 'NONE',  ( 12.98644063677341798, 8.526496012441747041, -16.01999686492960961 ) ) ;
#7588 = DIRECTION ( 'NONE',  ( -2.698458740408365879E-16, 1.000000000000000000, -0.000000000000000000 ) ) ;
#7589 = CARTESIAN_POINT ( 'NONE',  ( 4.000000000000000000, 1.557668341133518819, -2.290303434304245211 ) ) ;
#7590 = ORIENTED_EDGE ( 'NONE', *, *, #15755, .F. ) ;
#7591 = VECTOR ( 'NONE', #23857, 1000.000000000000000 ) ;
#7592 = PLANE ( 'NONE',  #16355 ) ;
#7593 = VECTOR ( 'NONE', #18842, 1000.000000000000000 ) ;
#7594 = FACE_OUTER_BOUND ( 'NONE', #8691, .T. ) ;
#7595 = ORIENTED_EDGE ( 'NONE', *, *, #2565, .F. ) ;
#7596 = ORIENTED_EDGE ( 'NONE', *, *, #15085, .F. ) ;
#7597 = CARTESIAN_POINT ( 'NONE',  ( 11.23996880139866761, 9.021883543159612273, -17.23462466665071346 ) ) ;
#7598 = CARTESIAN_POINT ( 'NONE',  ( 24.17451698631213475, -5.926886182136407832, -14.25952201372300365 ) ) ;
#7599 = EDGE_CURVE ( 'NONE', #27188, #13402, #29901, .T. ) ;
#7600 = CARTESIAN_POINT ( 'NONE',  ( 19.39950943988042553, -1.649204456521256246, -16.58530004841527727 ) ) ;
#7601 = DIRECTION ( 'NONE',  ( -0.8090169943749474513, -2.183098979609982436E-16, 0.5877852522924731371 ) ) ;
#7602 = CARTESIAN_POINT ( 'NONE',  ( 177.2287565553228319, -1.999999999999969358, -3.509618943233403510 ) ) ;
#7603 = EDGE_CURVE ( 'NONE', #24131, #11059, #16237, .T. ) ;
#7604 = FACE_OUTER_BOUND ( 'NONE', #928, .T. ) ;
#7605 = EDGE_CURVE ( 'NONE', #27678, #14364, #8762, .T. ) ;
#7606 = VECTOR ( 'NONE', #9226, 1000.000000000000000 ) ;
#7607 = CARTESIAN_POINT ( 'NONE',  ( 174.5152310637603819, -4.999999999999970690, -4.391296821672111328 ) ) ;
#7608 = CARTESIAN_POINT ( 'NONE',  ( 141.1922820468854525, -4.999999999999979572, -19.40354224447947473 ) ) ;
#7609 = DIRECTION ( 'NONE',  ( 0.000000000000000000, 0.000000000000000000, 1.000000000000000000 ) ) ;
#7610 = VECTOR ( 'NONE', #12878, 1000.000000000000000 ) ;
#7611 = PLANE ( 'NONE',  #23433 ) ;
#7613 = CARTESIAN_POINT ( 'NONE',  ( 175.7287565553229456, -4.999999999999970690, -10.89389676854972322 ) ) ;
#7612 = VECTOR ( 'NONE', #26956, 999.9999999999998863 ) ;
#7614 = CARTESIAN_POINT ( 'NONE',  ( 12.02780084644370007, 9.317182744227245905, -16.69143457430396893 ) ) ;
#7615 = CARTESIAN_POINT ( 'NONE',  ( -28.20515957282649921, 30.94299554780361206, 4.999999999999998224 ) ) ;
#7616 = CARTESIAN_POINT ( 'NONE',  ( 32.45272648307624053, -11.02157468472264412, -17.82583700188536824 ) ) ;
#7617 = ORIENTED_EDGE ( 'NONE', *, *, #14091, .T. ) ;
#7618 = CARTESIAN_POINT ( 'NONE',  ( 13.37597118643279970, 7.624349635725309327, -15.71077405172158947 ) ) ;
#7619 = DIRECTION ( 'NONE',  ( 1.000000000000000000, 2.698458740408365879E-16, -1.110223024625156540E-16 ) ) ;
#7620 = CARTESIAN_POINT ( 'NONE',  ( 18.97268594440662426, -2.511067197207834667, -17.06021009607598415 ) ) ;
#7621 = CARTESIAN_POINT ( 'NONE',  ( 12.86662121207793241, 9.515397394723519753, -16.11672893869402756 ) ) ;
#7622 = DIRECTION ( 'NONE',  ( -1.000000000000000000, 0.000000000000000000, 0.000000000000000000 ) ) ;
#7623 = EDGE_CURVE ( 'NONE', #26798, #6983, #9052, .T. ) ;
#7624 = ORIENTED_EDGE ( 'NONE', *, *, #14855, .T. ) ;
#7625 = CARTESIAN_POINT ( 'NONE',  ( 10.95411528722473626, 11.64838591225006859, -16.07543820933196699 ) ) ;
#7626 = DIRECTION ( 'NONE',  ( -0.000000000000000000, 0.000000000000000000, 1.000000000000000000 ) ) ;
#7627 = CIRCLE ( 'NONE', #21771, 8.000000000000007105 ) ;
#7628 = CARTESIAN_POINT ( 'NONE',  ( 9.926830210242822972, 16.35964622367879784, -16.50025672554925293 ) ) ;
#7629 = DIRECTION ( 'NONE',  ( -0.5877852522924731371, -1.586114251531760728E-16, -0.8090169943749474513 ) ) ;
#7630 = ORIENTED_EDGE ( 'NONE', *, *, #18418, .T. ) ;
#7631 = CARTESIAN_POINT ( 'NONE',  ( 138.6922820468854241, -1.999999999999980016, -0.6060766987539614181 ) ) ;
#7632 = EDGE_LOOP ( 'NONE', ( #28419, #17135, #19042, #10992, #21715 ) ) ;
#7633 = CARTESIAN_POINT ( 'NONE',  ( 12.06596557120094992, 9.177570865404522493, -16.67295095431955332 ) ) ;
#7634 = ORIENTED_EDGE ( 'NONE', *, *, #3607, .F. ) ;
#7636 = CARTESIAN_POINT ( 'NONE',  ( 33.34778169882233811, -10.20066162918134367, -19.85315749909214844 ) ) ;
#7635 = VECTOR ( 'NONE', #28016, 1000.000000000000000 ) ;
#7637 = CARTESIAN_POINT ( 'NONE',  ( 16.60417661732421735, 9.954854064686266213, -19.72231676211552909 ) ) ;
#7638 = CARTESIAN_POINT ( 'NONE',  ( 26.57062215293289498, -11.41726559881178638, -18.09730928560479057 ) ) ;
#7639 = EDGE_LOOP ( 'NONE', ( #4819, #20533, #8842, #11972 ) ) ;
#7640 = AXIS2_PLACEMENT_3D ( 'NONE', #9790, #13910, #26143 ) ;
#7641 = DIRECTION ( 'NONE',  ( -0.8090169943749474513, -2.183098979609982436E-16, 0.5877852522924731371 ) ) ;
#7642 = EDGE_LOOP ( 'NONE', ( #19937, #26511, #5293, #15205, #27545 ) ) ;
#7643 = VERTEX_POINT ( 'NONE', #8910 ) ;
#7644 = ADVANCED_FACE ( 'NONE', ( #11649 ), #18227, .T. ) ;
#7645 = CARTESIAN_POINT ( 'NONE',  ( 33.42826320546385688, -10.41623213582910523, -18.33855703361424361 ) ) ;
#7646 = ITEM_DEFINED_TRANSFORMATION ( 'NONE', 'NONE', #9243,  #13190 ) ;
#7647 = CARTESIAN_POINT ( 'NONE',  ( 18.37740474667574730, 3.980509343919368614, -15.11632106699347844 ) ) ;
#7648 = VECTOR ( 'NONE', #14695, 1000.000000000000000 ) ;
#7649 = CARTESIAN_POINT ( 'NONE',  ( 28.43808809371321189, -7.037065510061861318, -17.41003659457544117 ) ) ;
#7650 = ORIENTED_EDGE ( 'NONE', *, *, #19817, .F. ) ;
#7651 = CARTESIAN_POINT ( 'NONE',  ( 0.000000000000000000, 0.000000000000000000, -15.00000000000000000 ) ) ;
#7652 = FACE_BOUND ( 'NONE', #15216, .T. ) ;
#7653 = VECTOR ( 'NONE', #20342, 1000.000000000000000 ) ;
#7654 = CARTESIAN_POINT ( 'NONE',  ( 168.6922820468853104, -1.999999999999971800, -6.413161187712876909 ) ) ;
#7655 = CARTESIAN_POINT ( 'NONE',  ( 0.000000000000000000, 0.000000000000000000, -5.000000000000000888 ) ) ;
#7656 = CARTESIAN_POINT ( 'NONE',  ( 158.6922820468853672, -4.999999999999975131, -15.07341522555727664 ) ) ;
#7657 = AXIS2_PLACEMENT_3D ( 'NONE', #27201, #24881, #18140 ) ;
#7658 = FACE_OUTER_BOUND ( 'NONE', #20832, .T. ) ;
#7659 = CARTESIAN_POINT ( 'NONE',  ( 10.85049725708738855, 16.03634806290433801, -15.90056160573019284 ) ) ;
#7660 = DIRECTION ( 'NONE',  ( -0.5877852522924731371, -1.586114251531760728E-16, -0.8090169943749474513 ) ) ;
#7661 = ADVANCED_FACE ( 'NONE', ( #29753 ), #18078, .T. ) ;
#7662 = CARTESIAN_POINT ( 'NONE',  ( 3.678949249685231848, 0.000000000000000000, 0.000000000000000000 ) ) ;
#7663 = EDGE_LOOP ( 'NONE', ( #9264, #4387, #21242, #26418, #3509, #10254 ) ) ;
#7664 = CARTESIAN_POINT ( 'NONE',  ( 12.48799528366842360, 8.565546312597838607, -15.13973160209665991 ) ) ;
#7665 = EDGE_CURVE ( 'NONE', #29884, #8986, #1926, .T. ) ;
#7666 = CARTESIAN_POINT ( 'NONE',  ( 18.18253756980838531, -1.899343836538245789, -17.94647550410194370 ) ) ;
#7667 = PLANE ( 'NONE',  #2510 ) ;
#7668 = SURFACE_STYLE_USAGE ( .BOTH. , #5075 ) ;
#7669 = CARTESIAN_POINT ( 'NONE',  ( 162.2287565553229740, -4.999999999999973355, -29.49038105676660138 ) ) ;
#7670 = ORIENTED_EDGE ( 'NONE', *, *, #30124, .F. ) ;
#7671 = CARTESIAN_POINT ( 'NONE',  ( 177.2287565553228603, -9.999999999999994671, -12.16987298107780369 ) ) ;
#7672 = CARTESIAN_POINT ( 'NONE',  ( 12.85916040382217318, 9.514151651470600157, -16.12251888295402580 ) ) ;
#7673 = ORIENTED_EDGE ( 'NONE', *, *, #26824, .F. ) ;
#7674 = CARTESIAN_POINT ( 'NONE',  ( 35.05137900175546406, -18.95079263513605028, -19.16533087415493952 ) ) ;
#7675 = CARTESIAN_POINT ( 'NONE',  ( 16.89609864265585060, 4.102175112930991574, -14.31125941877678720 ) ) ;
#7676 = ORIENTED_EDGE ( 'NONE', *, *, #17141, .T. ) ;
#7677 = AXIS2_PLACEMENT_3D ( 'NONE', #4595, #13883, #21519 ) ;
#7678 = DIRECTION ( 'NONE',  ( 0.3090169943749472292, 8.338696094057992503E-17, -0.9510565162951536422 ) ) ;
#7679 = CARTESIAN_POINT ( 'NONE',  ( 15.33641899704135980, 5.898237403637139664, -14.35162154369138676 ) ) ;
#7680 = ORIENTED_EDGE ( 'NONE', *, *, #2177, .T. ) ;
#7681 = CARTESIAN_POINT ( 'NONE',  ( 131.1922820468854241, -10.00000000000000888, -30.91696583120935671 ) ) ;
#7682 = CARTESIAN_POINT ( 'NONE',  ( 22.34648740292275093, -2.602002351270185532, -19.46322174391540116 ) ) ;
#7683 = AXIS2_PLACEMENT_3D ( 'NONE', #10441, #17464, #10754 ) ;
#7684 = CARTESIAN_POINT ( 'NONE',  ( 18.98827506421364575, 7.203492520304279445, -17.17051369180543929 ) ) ;
#7685 = LINE ( 'NONE', #19275, #29935 ) ;
#7686 = ORIENTED_EDGE ( 'NONE', *, *, #22977, .T. ) ;
#7687 = DIRECTION ( 'NONE',  ( -0.000000000000000000, -0.000000000000000000, -1.000000000000000000 ) ) ;
#7688 = AXIS2_PLACEMENT_3D ( 'NONE', #25829, #4912, #14208 ) ;
#7689 = CARTESIAN_POINT ( 'NONE',  ( 131.1922820468854241, -10.00000000000000888, -2.083034168790677043 ) ) ;
#7690 = CARTESIAN_POINT ( 'NONE',  ( 4.000000000000008882, -6.928203230275510549, 0.000000000000000000 ) ) ;
#7691 = CARTESIAN_POINT ( 'NONE',  ( 176.1922820468853104, -9.999999999999994671, -19.40354224447947828 ) ) ;
#7692 = LINE ( 'NONE', #17004, #24617 ) ;
#7693 = VECTOR ( 'NONE', #18054, 1000.000000000000000 ) ;
#7694 = CARTESIAN_POINT ( 'NONE',  ( 11.47372892693763902, 9.265404009280679531, -15.86055721330185619 ) ) ;
#7695 = CARTESIAN_POINT ( 'NONE',  ( 28.09155340820903390, -11.11649160481613130, -13.74484337247343824 ) ) ;
#7696 = CARTESIAN_POINT ( 'NONE',  ( 22.09907825138052218, -7.445301066569870230, -16.29136317631293807 ) ) ;
#7697 = EDGE_CURVE ( 'NONE', #11977, #23167, #27581, .T. ) ;
#7699 = ORIENTED_EDGE ( 'NONE', *, *, #3171, .F. ) ;
#7698 = CARTESIAN_POINT ( 'NONE',  ( 33.17819505895439391, -11.78846528140086924, -19.49437495119144259 ) ) ;
#7700 = LINE ( 'NONE', #7414, #16851 ) ;
#7701 = AXIS2_PLACEMENT_3D ( 'NONE', #3704, #17577, #26934 ) ;
#7702 = CARTESIAN_POINT ( 'NONE',  ( 156.1922820468854241, -10.00000000000000000, -28.06379628232387802 ) ) ;
#7703 = LINE ( 'NONE', #1282, #22372 ) ;
#7704 = DIRECTION ( 'NONE',  ( -2.698458740408366372E-16, 1.000000000000000000, 0.000000000000000000 ) ) ;
#7705 = EDGE_CURVE ( 'NONE', #5343, #15277, #18376, .T. ) ;
#7706 = FACE_OUTER_BOUND ( 'NONE', #18007, .T. ) ;
#7707 = CARTESIAN_POINT ( 'NONE',  ( 175.7287565553229456, -4.999999999999969802, -19.55415080639413006 ) ) ;
#7708 = ADVANCED_FACE ( 'NONE', ( #20967 ), #13644, .T. ) ;
#7709 = CARTESIAN_POINT ( 'NONE',  ( 17.21692058948253035, 4.245457944912791604, -14.13226496128363863 ) ) ;
#7710 = ORIENTED_EDGE ( 'NONE', *, *, #10100, .F. ) ;
#7711 = CARTESIAN_POINT ( 'NONE',  ( 5.000000000000005329, 2.220446049250313475E-15, 0.000000000000000000 ) ) ;
#7712 = CARTESIAN_POINT ( 'NONE',  ( 10.72094366404044408, 16.63049735485946101, -15.95413657539408980 ) ) ;
#7713 = FACE_OUTER_BOUND ( 'NONE', #29899, .T. ) ;
#7714 = CARTESIAN_POINT ( 'NONE',  ( 5.000000000000000000, -6.123233995736766282E-16, -23.00000000000000000 ) ) ;
#7715 = CARTESIAN_POINT ( 'NONE',  ( 19.25770813156441008, -2.543370271471735222, -15.40753146551623587 ) ) ;
#7716 = CARTESIAN_POINT ( 'NONE',  ( 32.47832896513632761, -9.914179286496517918, -13.92895715894296771 ) ) ;
#7717 = ORIENTED_EDGE ( 'NONE', *, *, #10620, .F. ) ;
#7718 = CARTESIAN_POINT ( 'NONE',  ( 35.53434814243864537, -22.12051714835155281, -18.84852710552948096 ) ) ;
#7719 = CARTESIAN_POINT ( 'NONE',  ( 26.06151603483908019, -7.281686956891486595, -19.93845510724469960 ) ) ;
#7720 = CARTESIAN_POINT ( 'NONE',  ( 18.73405575602592776, 1.888441813480535414, -14.99786396448725156 ) ) ;
#7721 = VECTOR ( 'NONE', #12368, 1000.000000000000000 ) ;
#7722 = ORIENTED_EDGE ( 'NONE', *, *, #411, .F. ) ;
#7723 = CARTESIAN_POINT ( 'NONE',  ( 137.2287565553230309, -1.999999999999979572, -12.16987298107780013 ) ) ;
#7724 = AXIS2_PLACEMENT_3D ( 'NONE', #20880, #2736, #25827 ) ;
#7725 = EDGE_CURVE ( 'NONE', #19562, #2080, #25262, .T. ) ;
#7726 = VECTOR ( 'NONE', #28716, 1000.000000000000000 ) ;
#7727 = DIRECTION ( 'NONE',  ( -2.698458740408365879E-16, 1.000000000000000000, 0.000000000000000000 ) ) ;
#7728 = CARTESIAN_POINT ( 'NONE',  ( 144.5152310637606092, -1.999999999999977129, -19.94844914048349693 ) ) ;
#7729 = LINE ( 'NONE', #22075, #4592 ) ;
#7730 = DIRECTION ( 'NONE',  ( -0.5877852522924731371, -1.586114251531760728E-16, -0.8090169943749474513 ) ) ;
#7731 = CARTESIAN_POINT ( 'NONE',  ( 36.54859390953724585, -22.18451583373416014, -17.99055332684694974 ) ) ;
#7732 = CARTESIAN_POINT ( 'NONE',  ( 9.981537699549546616, 16.10875070413535681, -16.47763325427154868 ) ) ;
#7733 = EDGE_CURVE ( 'NONE', #13894, #27247, #16389, .T. ) ;
#7734 = DIRECTION ( 'NONE',  ( 0.000000000000000000, 0.000000000000000000, 1.000000000000000000 ) ) ;
#7735 = CARTESIAN_POINT ( 'NONE',  ( 162.2287565553229740, -9.999999999999998224, -29.49038105676660493 ) ) ;
#7736 = EDGE_CURVE ( 'NONE', #3555, #23467, #11211, .T. ) ;
#7737 = ADVANCED_FACE ( 'NONE', ( #18533 ), #29300, .F. ) ;
#7738 = CARTESIAN_POINT ( 'NONE',  ( 12.02609123740286101, 9.325023229212996867, -16.69214155778140096 ) ) ;
#7739 = PLANE ( 'NONE',  #16078 ) ;
#7740 = ADVANCED_FACE ( 'NONE', ( #1774 ), #11060, .T. ) ;
#7741 = DIRECTION ( 'NONE',  ( 0.9510565162951536422, 0.000000000000000000, -0.3090169943749475623 ) ) ;
#7742 = ORIENTED_EDGE ( 'NONE', *, *, #26602, .T. ) ;
#7743 = VECTOR ( 'NONE', #2989, 1000.000000000000000 ) ;
#7744 = CARTESIAN_POINT ( 'NONE',  ( 130.7287565553229456, -10.00000000000000888, -10.89389676854976408 ) ) ;
#7745 = DIRECTION ( 'NONE',  ( 1.110223024625156540E-16, 2.995891024602366092E-32, 1.000000000000000000 ) ) ;
#7746 = DIRECTION ( 'NONE',  ( -2.698458740408365879E-16, 1.000000000000000000, 0.000000000000000000 ) ) ;
#7747 = ORIENTED_EDGE ( 'NONE', *, *, #14093, .F. ) ;
#7748 = VECTOR ( 'NONE', #23901, 1000.000000000000000 ) ;
#7749 = ORIENTED_EDGE ( 'NONE', *, *, #23254, .F. ) ;
#7750 = CARTESIAN_POINT ( 'NONE',  ( 11.32192133241855103, 8.753083428987814330, -17.19257025691282337 ) ) ;
#7751 = VERTEX_POINT ( 'NONE', #26321 ) ;
#7752 = CARTESIAN_POINT ( 'NONE',  ( 23.84753192840887337, -5.516882280943989691, -18.03677479665242345 ) ) ;
#7753 = CARTESIAN_POINT ( 'NONE',  ( 23.74924978780510898, -3.048960050427876656, -13.27477993493952191 ) ) ;
#7754 = CARTESIAN_POINT ( 'NONE',  ( 144.7287565553230309, -10.00000000000000355, -33.82050807568879947 ) ) ;
#7755 = DIRECTION ( 'NONE',  ( 0.5877852522924731371, 1.586114251531760728E-16, -0.8090169943749474513 ) ) ;
#7756 = CARTESIAN_POINT ( 'NONE',  ( 142.0152310637605524, -10.00000000000000533, 1.702185954127501066 ) ) ;
#7757 = LINE ( 'NONE', #19647, #16731 ) ;
#7758 = CARTESIAN_POINT ( 'NONE',  ( 164.7287565553228887, -1.999999999999972689, 0.8205080756887930260 ) ) ;
#7759 = VECTOR ( 'NONE', #14802, 1000.000000000000000 ) ;
#7760 = DIRECTION ( 'NONE',  ( -2.698458740408365879E-16, 1.000000000000000000, 0.000000000000000000 ) ) ;
#7761 = DIRECTION ( 'NONE',  ( -1.000000000000000000, 0.000000000000000000, 0.000000000000000000 ) ) ;
#7762 = CARTESIAN_POINT ( 'NONE',  ( 174.7287565553228603, -4.999999999999970690, -7.839745962155600267 ) ) ;
#7763 = VECTOR ( 'NONE', #9096, 1000.000000000000000 ) ;
#7764 = CARTESIAN_POINT ( 'NONE',  ( 12.02001262747988797, 9.352900509162292764, -16.69465527681230199 ) ) ;
#7765 = CARTESIAN_POINT ( 'NONE',  ( 33.80310782676656345, -13.34297147354166135, -18.78800844379110302 ) ) ;
#7766 = ORIENTED_EDGE ( 'NONE', *, *, #29045, .T. ) ;
#7767 = CARTESIAN_POINT ( 'NONE',  ( 8.944584683310379702, 16.95159276115599667, -17.97192418671890835 ) ) ;
#7768 = EDGE_CURVE ( 'NONE', #19382, #18123, #9820, .T. ) ;
#7769 = DIRECTION ( 'NONE',  ( 0.000000000000000000, 0.000000000000000000, -1.000000000000000000 ) ) ;
#7770 = CARTESIAN_POINT ( 'NONE',  ( 22.86252235622482587, -0.9498377794471745128, -13.29674124224850118 ) ) ;
#7771 = EDGE_CURVE ( 'NONE', #5490, #952, #19988, .T. ) ;
#7772 = CARTESIAN_POINT ( 'NONE',  ( 12.67014222779069854, 10.28407994610609144, -16.20807751338157843 ) ) ;
#7773 = LINE ( 'NONE', #3065, #4372 ) ;
#7774 = EDGE_CURVE ( 'NONE', #27148, #28906, #3132, .T. ) ;
#7775 = ORIENTED_EDGE ( 'NONE', *, *, #27930, .F. ) ;
#7776 = CARTESIAN_POINT ( 'NONE',  ( 9.957223259857686415, 16.22025982393231303, -16.48768813039480818 ) ) ;
#7777 = LINE ( 'NONE', #17088, #7247 ) ;
#7778 = CARTESIAN_POINT ( 'NONE',  ( 9.910898653440767703, 16.43271037397421708, -16.50709950392603531 ) ) ;
#7779 = CARTESIAN_POINT ( 'NONE',  ( 174.7287565553229456, -4.999999999999969802, -25.16025403784439973 ) ) ;
#7780 = ORIENTED_EDGE ( 'NONE', *, *, #14816, .F. ) ;
#7781 = DIRECTION ( 'NONE',  ( -2.698458740408365879E-16, 1.000000000000000000, 0.000000000000000000 ) ) ;
#7782 = ORIENTED_EDGE ( 'NONE', *, *, #24701, .T. ) ;
#7783 =( GEOMETRIC_REPRESENTATION_CONTEXT ( 3 ) GLOBAL_UNCERTAINTY_ASSIGNED_CONTEXT ( ( #11622 ) ) GLOBAL_UNIT_ASSIGNED_CONTEXT ( ( #29747, #27726, #4342 ) ) REPRESENTATION_CONTEXT ( 'NONE', 'WORKASPACE' ) );
#7784 = CARTESIAN_POINT ( 'NONE',  ( 11.98759337455738816, 9.501579335558542283, -16.70806177831036976 ) ) ;
#7785 = EDGE_LOOP ( 'NONE', ( #30150, #6671, #14835, #7282 ) ) ;
#7786 = VECTOR ( 'NONE', #10957, 1000.000000000000000 ) ;
#7787 = CARTESIAN_POINT ( 'NONE',  ( 36.54859390954302967, -23.18451583373416014, -15.55638201429745848 ) ) ;
#7788 = CARTESIAN_POINT ( 'NONE',  ( 29.82081855766934453, -7.722587238354316597, -15.76009366473342332 ) ) ;
#7789 = CARTESIAN_POINT ( 'NONE',  ( 17.30683543869610119, 10.98570342618945617, -17.92154440881979482 ) ) ;
#7790 = VERTEX_POINT ( 'NONE', #5249 ) ;
#7791 = CARTESIAN_POINT ( 'NONE',  ( 133.7287565553229456, -9.999999999999980460, 0.5000000000000029976 ) ) ;
#7792 = ORIENTED_EDGE ( 'NONE', *, *, #5121, .F. ) ;
#7793 = AXIS2_PLACEMENT_3D ( 'NONE', #15564, #21995, #8244 ) ;
#7794 = AXIS2_PLACEMENT_3D ( 'NONE', #16881, #24219, #3605 ) ;
#7795 = DIRECTION ( 'NONE',  ( -1.000000000000000000, 0.000000000000000000, 0.000000000000000000 ) ) ;
#7796 = SHAPE_DEFINITION_REPRESENTATION ( #24716, #18708 ) ;
#7797 = VERTEX_POINT ( 'NONE', #380 ) ;
#7798 = CARTESIAN_POINT ( 'NONE',  ( 19.81827328964134338, 3.502454073897792952, -18.79004964864563476 ) ) ;
#7799 = CARTESIAN_POINT ( 'NONE',  ( 17.85084670134855145, 5.929878015568476712, -20.08862479909851828 ) ) ;
#7800 = ORIENTED_EDGE ( 'NONE', *, *, #16308, .T. ) ;
#7801 = LINE ( 'NONE', #5518, #15405 ) ;
#7802 = EDGE_CURVE ( 'NONE', #23532, #11745, #23416, .T. ) ;
#7803 = CARTESIAN_POINT ( 'NONE',  ( 2.500000000000000444, 0.000000000000000000, 0.000000000000000000 ) ) ;
#7804 = CARTESIAN_POINT ( 'NONE',  ( 15.04976660853063741, -5.000000000000013323, -46.31841892940461491 ) ) ;
#7805 = DIRECTION ( 'NONE',  ( 0.9510565162951535312, 2.566386769018988816E-16, -0.3090169943749475623 ) ) ;
#7806 = CIRCLE ( 'NONE', #7335, 5.999999999999977796 ) ;
#7807 = CARTESIAN_POINT ( 'NONE',  ( 172.0152310637604955, -1.999999999999969580, -24.27857615940569502 ) ) ;
#7808 = DIRECTION ( 'NONE',  ( 0.000000000000000000, 0.000000000000000000, 1.000000000000000000 ) ) ;
#7809 = AXIS2_PLACEMENT_3D ( 'NONE', #5099, #17147, #7542 ) ;
#7810 = CARTESIAN_POINT ( 'NONE',  ( 12.26606010314042017, 9.512972848517913249, -15.31757320754432605 ) ) ;
#7811 = EDGE_CURVE ( 'NONE', #19672, #20712, #12110, .T. ) ;
#7812 = LINE ( 'NONE', #19396, #28035 ) ;
#7813 = CARTESIAN_POINT ( 'NONE',  ( 4.681481898397010788, -6.534749472788171865, -4.999999999999988454 ) ) ;
#7814 = ORIENTED_EDGE ( 'NONE', *, *, #23522, .T. ) ;
#7815 = CARTESIAN_POINT ( 'NONE',  ( 12.51757296969303290, 8.578467993704791184, -15.11616904564172792 ) ) ;
#7816 = CARTESIAN_POINT ( 'NONE',  ( 19.38139026969670553, 5.460277215109251792, -15.14974238112136540 ) ) ;
#7817 = DIRECTION ( 'NONE',  ( -1.110223024625156540E-16, 0.000000000000000000, -1.000000000000000000 ) ) ;
#7818 = LINE ( 'NONE', #17126, #15941 ) ;
#7819 = DIRECTION ( 'NONE',  ( -0.9510565162951536422, -2.566386769018988816E-16, -0.3090169943749472292 ) ) ;
#7820 = ORIENTED_EDGE ( 'NONE', *, *, #3951, .F. ) ;
#7821 = CARTESIAN_POINT ( 'NONE',  ( 137.0152310637606092, -10.00000000000000533, -6.958068083716895558 ) ) ;
#7822 = ORIENTED_EDGE ( 'NONE', *, *, #29687, .F. ) ;
#7823 = CARTESIAN_POINT ( 'NONE',  ( 12.67014222779069854, 10.28407994610609144, -16.20807751338157843 ) ) ;
#7824 = VECTOR ( 'NONE', #8787, 1000.000000000000000 ) ;
#7825 = ORIENTED_EDGE ( 'NONE', *, *, #10213, .F. ) ;
#7826 = CARTESIAN_POINT ( 'NONE',  ( 36.44623027834506956, -20.72465026231317253, -19.27049969669971929 ) ) ;
#7827 = CARTESIAN_POINT ( 'NONE',  ( 21.66440995182641416, 5.535554982823286174, -17.57621636221614025 ) ) ;
#7828 = ORIENTED_EDGE ( 'NONE', *, *, #19070, .T. ) ;
#7829 = CARTESIAN_POINT ( 'NONE',  ( 147.2287565553230024, -10.00000000000000355, -12.16987298107780369 ) ) ;
#7830 = CARTESIAN_POINT ( 'NONE',  ( 26.89114594638229505, -13.18314149429672000, -12.91981678032827041 ) ) ;
#7831 = EDGE_LOOP ( 'NONE', ( #20505, #12348, #11044, #24446 ) ) ;
#7832 = FACE_OUTER_BOUND ( 'NONE', #23497, .T. ) ;
#7833 = CARTESIAN_POINT ( 'NONE',  ( 26.78588127033857091, -2.187643107580064861, -16.18476928258297676 ) ) ;
#7834 = CARTESIAN_POINT ( 'NONE',  ( 20.65939765650831461, 5.541921473274042498, -17.57530766875797568 ) ) ;
#7835 = CARTESIAN_POINT ( 'NONE',  ( 147.0152310637605524, -1.999999999999977129, -6.958068083716895558 ) ) ;
#7836 = ORIENTED_EDGE ( 'NONE', *, *, #4864, .T. ) ;
#7837 = EDGE_CURVE ( 'NONE', #13174, #1647, #19279, .T. ) ;
#7838 = CARTESIAN_POINT ( 'NONE',  ( 159.5152310637604671, -1.999999999999974021, -2.627941064794695691 ) ) ;
#7839 = PRODUCT_DEFINITION ( 'UNKNOWN', '', #19498, #20779 ) ;
#7840 = CARTESIAN_POINT ( 'NONE',  ( 94.69354921296734062, -4.999999999999992006, 68.79889063098933377 ) ) ;
#7841 = FACE_OUTER_BOUND ( 'NONE', #19911, .T. ) ;
#7842 = CARTESIAN_POINT ( 'NONE',  ( 131.1922820468854241, -10.00000000000000888, -13.59645775552055547 ) ) ;
#7843 = VECTOR ( 'NONE', #27676, 1000.000000000000114 ) ;
#7844 = DIRECTION ( 'NONE',  ( -0.8090169943749474513, -2.183098979609982436E-16, 0.5877852522924731371 ) ) ;
#7845 = CARTESIAN_POINT ( 'NONE',  ( 11.58682163191119230, 8.958038730125363003, -15.79767441425272345 ) ) ;
#7846 = CARTESIAN_POINT ( 'NONE',  ( 29.29611939376944107, -10.57052713796966081, -13.72407686852593400 ) ) ;
#7847 = CARTESIAN_POINT ( 'NONE',  ( 28.50411217586706769, -6.135108760518566129, -18.55796808427148648 ) ) ;
#7849 = ORIENTED_EDGE ( 'NONE', *, *, #10581, .T. ) ;
#7848 = CARTESIAN_POINT ( 'NONE',  ( 35.54859390954303677, -23.18451583373416014, -15.55638201429745848 ) ) ;
#7850 = DIRECTION ( 'NONE',  ( -1.000000000000000000, -4.440892098500622217E-16, 0.000000000000000000 ) ) ;
#7851 = FACE_OUTER_BOUND ( 'NONE', #8377, .T. ) ;
#7852 = CARTESIAN_POINT ( 'NONE',  ( -0.6554360035617876612, 4.240386000424035906, -0.1586754815284892317 ) ) ;
#7853 = CARTESIAN_POINT ( 'NONE',  ( 13.00000000000000178, 0.000000000000000000, 15.00000000000000000 ) ) ;
#7854 = DIRECTION ( 'NONE',  ( 0.000000000000000000, 0.000000000000000000, 1.000000000000000000 ) ) ;
#7855 = CARTESIAN_POINT ( 'NONE',  ( 173.6922820468853672, -1.999999999999969358, -35.24709285013155835 ) ) ;
#7856 = CARTESIAN_POINT ( 'NONE',  ( 16.89609864265585060, 4.102175112930991574, -14.31125941877678720 ) ) ;
#7857 = EDGE_LOOP ( 'NONE', ( #9513, #21111, #18313, #5976 ) ) ;
#7858 = DIRECTION ( 'NONE',  ( 6.938893903907227392E-16, -0.000000000000000000, 1.000000000000000000 ) ) ;
#7859 = CARTESIAN_POINT ( 'NONE',  ( 12.14726737398757095, 10.08919500705755645, -15.36430154580878593 ) ) ;
#7860 = DIRECTION ( 'NONE',  ( -0.000000000000000000, 1.000000000000000000, 0.000000000000000000 ) ) ;
#7861 = DIRECTION ( 'NONE',  ( -2.698458740408365879E-16, 1.000000000000000000, 0.000000000000000000 ) ) ;
#7862 = CARTESIAN_POINT ( 'NONE',  ( 24.92864811393110358, -0.2441600445015326137, -14.78813717129899885 ) ) ;
#7863 = CARTESIAN_POINT ( 'NONE',  ( 20.91577097522866424, 8.170114823437694795, -18.25116917207579093 ) ) ;
#7864 = ORIENTED_EDGE ( 'NONE', *, *, #22670, .T. ) ;
#7866 = VECTOR ( 'NONE', #16716, 1000.000000000000000 ) ;
#7865 = CARTESIAN_POINT ( 'NONE',  ( 33.96943610671532809, -15.09019632882451134, -19.88060704079178720 ) ) ;
#7867 = CARTESIAN_POINT ( 'NONE',  ( 28.50845745928996067, -4.315366227951761502, -16.60164569054668604 ) ) ;
#7868 = AXIS2_PLACEMENT_3D ( 'NONE', #14112, #2556, #28216 ) ;
#7869 = CARTESIAN_POINT ( 'NONE',  ( 21.02038916656773182, -4.531596735700774481, -13.49074533895851147 ) ) ;
#7870 = EDGE_LOOP ( 'NONE', ( #20717, #19940, #386, #30 ) ) ;
#7871 = EDGE_CURVE ( 'NONE', #29710, #11366, #28490, .T. ) ;
#7872 = EDGE_CURVE ( 'NONE', #10756, #11518, #21267, .T. ) ;
#7873 = CARTESIAN_POINT ( 'NONE',  ( 21.54098841764929873, -5.100688324319140321, -15.19385678519978633 ) ) ;
#7874 = EDGE_CURVE ( 'NONE', #20344, #21061, #26172, .T. ) ;
#7875 = ORIENTED_EDGE ( 'NONE', *, *, #4980, .F. ) ;
#7876 = EDGE_CURVE ( 'NONE', #29420, #11271, #21427, .T. ) ;
#7877 = LINE ( 'NONE', #21766, #25996 ) ;
#7878 = EDGE_LOOP ( 'NONE', ( #10834, #9568, #19147, #28544 ) ) ;
#7879 = ORIENTED_EDGE ( 'NONE', *, *, #22493, .F. ) ;
#7880 = CARTESIAN_POINT ( 'NONE',  ( 90.15252717933853432, -4.999999999999992895, 65.49964500294863967 ) ) ;
#7881 = CARTESIAN_POINT ( 'NONE',  ( 156.1922820468853672, -10.00000000000000000, -13.59645775552055902 ) ) ;
#7882 = CARTESIAN_POINT ( 'NONE',  ( 174.7287565553229172, -9.999999999999994671, -25.16025403784440329 ) ) ;
#7883 = LINE ( 'NONE', #1032, #14116 ) ;
#7884 = CARTESIAN_POINT ( 'NONE',  ( 34.33515578781254618, -12.24072284059296933, -19.92088757525016973 ) ) ;
#7885 = CARTESIAN_POINT ( 'NONE',  ( 9.776119957569173735, 17.05082265352876547, -16.72288386497739765 ) ) ;
#7886 = LINE ( 'NONE', #28991, #28853 ) ;
#7887 = DIRECTION ( 'NONE',  ( 0.5877852522924731371, 1.586114251531760728E-16, -0.8090169943749474513 ) ) ;
#7888 = CARTESIAN_POINT ( 'NONE',  ( 12.02001262747988797, 9.352900509162292764, -16.69465527681230199 ) ) ;
#7889 = DIRECTION ( 'NONE',  ( 0.000000000000000000, 0.000000000000000000, -1.000000000000000000 ) ) ;
#7890 = CARTESIAN_POINT ( 'NONE',  ( 36.04859390953723874, -22.18451583373416014, -18.00000000000000000 ) ) ;
#7891 = ORIENTED_EDGE ( 'NONE', *, *, #20653, .T. ) ;
#7892 = CARTESIAN_POINT ( 'NONE',  ( 173.6922820468853672, -9.999999999999994671, -35.24709285013155835 ) ) ;
#7893 = CARTESIAN_POINT ( 'NONE',  ( 139.5152310637605808, -4.999999999999980460, -2.627941064794695691 ) ) ;
#7894 = AXIS2_PLACEMENT_3D ( 'NONE', #1433, #5705, #19876 ) ;
#7895 = FACE_OUTER_BOUND ( 'NONE', #18960, .T. ) ;
#7896 = ORIENTED_EDGE ( 'NONE', *, *, #8903, .F. ) ;
#7897 = ORIENTED_EDGE ( 'NONE', *, *, #7871, .F. ) ;
#7898 = ORIENTED_EDGE ( 'NONE', *, *, #22074, .F. ) ;
#7899 = CARTESIAN_POINT ( 'NONE',  ( 11.22408442728515077, 9.090372555205103566, -17.24152585048573982 ) ) ;
#7900 = CARTESIAN_POINT ( 'NONE',  ( 13.78422571733443647, 6.778978001458615843, -20.29761332830707232 ) ) ;
#7901 = CARTESIAN_POINT ( 'NONE',  ( 21.56383972367567736, -3.323709001909281202, -18.92284382192250192 ) ) ;
#7902 = CARTESIAN_POINT ( 'NONE',  ( 152.0152310637604671, -10.00000000000000178, -17.38167787843870826 ) ) ;
#7903 = LINE ( 'NONE', #5622, #23818 ) ;
#7904 = DIRECTION ( 'NONE',  ( 0.9510565162951535312, 2.566386769018988816E-16, -0.3090169943749475623 ) ) ;
#7905 = EDGE_CURVE ( 'NONE', #10263, #29352, #6448, .T. ) ;
#7906 = ORIENTED_EDGE ( 'NONE', *, *, #27177, .F. ) ;
#7907 = EDGE_CURVE ( 'NONE', #13441, #21824, #23886, .T. ) ;
#7908 = LINE ( 'NONE', #14462, #10833 ) ;
#7909 = CARTESIAN_POINT ( 'NONE',  ( 139.7287565553230309, -10.00000000000000533, -25.16025403784439973 ) ) ;
#7910 = DIRECTION ( 'NONE',  ( 0.000000000000000000, 0.000000000000000000, 1.000000000000000000 ) ) ;
#7911 = VECTOR ( 'NONE', #16309, 1000.000000000000000 ) ;
#7912 = LINE ( 'NONE', #22254, #11224 ) ;
#7913 = DIRECTION ( 'NONE',  ( -0.8116843969807016057, -0.5840962589317576503, 0.000000000000000000 ) ) ;
#7914 = CARTESIAN_POINT ( 'NONE',  ( 13.12553198385420927, 8.571700941790735939, -15.91037888968202552 ) ) ;
#7915 = CARTESIAN_POINT ( 'NONE',  ( 35.52583876341286384, -22.08228901593173177, -18.97221062538168113 ) ) ;
#7916 = EDGE_LOOP ( 'NONE', ( #6326, #406, #13974, #29488, #22260, #3696 ) ) ;
#7917 = CARTESIAN_POINT ( 'NONE',  ( 9.068088202150136112, 16.38518988071972871, -17.09785080524718381 ) ) ;
#7918 = AXIS2_PLACEMENT_3D ( 'NONE', #16695, #16993, #13824 ) ;
#7919 = CARTESIAN_POINT ( 'NONE',  ( 24.43075134246613800, -6.859861339260811874, -14.00379227226492951 ) ) ;
#7920 = CARTESIAN_POINT ( 'NONE',  ( 12.83230269852989203, 9.540395929213350001, -16.14101810565610151 ) ) ;
#7921 = FACE_BOUND ( 'NONE', #13384, .T. ) ;
#7922 = ORIENTED_EDGE ( 'NONE', *, *, #24814, .F. ) ;
#7923 = DIRECTION ( 'NONE',  ( -2.698458740408365879E-16, 1.000000000000000000, 0.000000000000000000 ) ) ;
#7924 = CARTESIAN_POINT ( 'NONE',  ( 11.47511325496290624, 9.259230714725578792, -15.85997136665693041 ) ) ;
#7925 = DIRECTION ( 'NONE',  ( 1.000000000000000000, 2.698458740408365879E-16, -1.110223024625156540E-16 ) ) ;
#7926 = ORIENTED_EDGE ( 'NONE', *, *, #22453, .F. ) ;
#7927 = CARTESIAN_POINT ( 'NONE',  ( 171.1922820468853104, -9.999999999999996447, -10.74328820663507678 ) ) ;
#7928 = ORIENTED_EDGE ( 'NONE', *, *, #15442, .T. ) ;
#7929 = CARTESIAN_POINT ( 'NONE',  ( 12.02841764901576838, 9.314357472305010432, -16.69117924060192948 ) ) ;
#7930 = VERTEX_POINT ( 'NONE', #14693 ) ;
#7931 = CARTESIAN_POINT ( 'NONE',  ( 22.08592964957147586, 4.518037853963432049, -19.67680751601638889 ) ) ;
#7932 = CARTESIAN_POINT ( 'NONE',  ( 13.34169928452473819, 6.621333031661079005, -16.53230918748570488 ) ) ;
#7933 = CONICAL_SURFACE ( 'NONE', #13143, 2.055000000000000160, 0.7853981633974721488 ) ;
#7934 = LINE ( 'NONE', #29041, #16981 ) ;
#7935 = VERTEX_POINT ( 'NONE', #21120 ) ;
#7936 = CARTESIAN_POINT ( 'NONE',  ( 36.54222296954648641, -22.15589457513855010, -18.69601260479128513 ) ) ;
#7937 = PRODUCT_CONTEXT ( 'NONE', #3641, 'mechanical' ) ;
#7938 = CARTESIAN_POINT ( 'NONE',  ( 20.59924605810746101, 4.422246688411098248, -17.72709849028201035 ) ) ;
#7939 = CARTESIAN_POINT ( 'NONE',  ( 16.75072914628186282, 8.771658487634226731, -19.67538163746542779 ) ) ;
#7940 = ADVANCED_FACE ( 'NONE', ( #24034 ), #21717, .T. ) ;
#7941 = EDGE_CURVE ( 'NONE', #12834, #2206, #28795, .T. ) ;
#7942 = VECTOR ( 'NONE', #4093, 1000.000000000000000 ) ;
#7943 = EDGE_CURVE ( 'NONE', #846, #11701, #16545, .T. ) ;
#7944 =( NAMED_UNIT ( * ) SI_UNIT ( $, .STERADIAN. ) SOLID_ANGLE_UNIT ( ) );
#7945 = EDGE_CURVE ( 'NONE', #24305, #6528, #25867, .T. ) ;
#7946 = FACE_BOUND ( 'NONE', #11596, .T. ) ;
#7947 = LINE ( 'NONE', #497, #5283 ) ;
#7948 = DIRECTION ( 'NONE',  ( 1.000000000000000000, 2.698458740408365879E-16, -1.110223024625156540E-16 ) ) ;
#7949 = CARTESIAN_POINT ( 'NONE',  ( 17.43705417884378051, -5.000000000000013323, -53.66573458306050526 ) ) ;
#7950 = VERTEX_POINT ( 'NONE', #28346 ) ;
#7951 = DIRECTION ( 'NONE',  ( 0.5877852522924731371, 0.000000000000000000, 0.8090169943749474513 ) ) ;
#7952 = CARTESIAN_POINT ( 'NONE',  ( 12.27691367651725862, 9.494620545951883983, -15.31068823849801319 ) ) ;
#7953 = PLANE ( 'NONE',  #9903 ) ;
#7954 = CARTESIAN_POINT ( 'NONE',  ( 0.000000000000000000, -2.357898499370430834, 3.469446951953614189E-15 ) ) ;
#7955 = ORIENTED_EDGE ( 'NONE', *, *, #16701, .F. ) ;
#7956 = CARTESIAN_POINT ( 'NONE',  ( 12.60945047077962933, 8.619070305187777947, -15.04294105552940231 ) ) ;
#7957 = ORIENTED_EDGE ( 'NONE', *, *, #14402, .F. ) ;
#7958 = CIRCLE ( 'NONE', #11381, 3.000000000000002665 ) ;
#7959 = CARTESIAN_POINT ( 'NONE',  ( 10.66878845912243534, 9.044174962973633214, -16.41115715542894193 ) ) ;
#7960 = DIRECTION ( 'NONE',  ( 0.000000000000000000, 0.000000000000000000, 1.000000000000000000 ) ) ;
#7961 = CARTESIAN_POINT ( 'NONE',  ( 171.1922820468853104, -9.999999999999996447, -10.74328820663507678 ) ) ;
#7962 = ORIENTED_EDGE ( 'NONE', *, *, #14270, .F. ) ;
#7963 = DIRECTION ( 'NONE',  ( -2.698458740408365879E-16, 1.000000000000000000, 0.000000000000000000 ) ) ;
#7964 = CARTESIAN_POINT ( 'NONE',  ( 20.00000000000017053, 27.64101615137744972, 10.00000000000000178 ) ) ;
#7965 = ORIENTED_EDGE ( 'NONE', *, *, #4771, .T. ) ;
#7966 = CARTESIAN_POINT ( 'NONE',  ( 12.83097211533594439, 9.546493580781078236, -16.14156869735677446 ) ) ;
#7967 = ORIENTED_EDGE ( 'NONE', *, *, #6013, .T. ) ;
#7968 = CARTESIAN_POINT ( 'NONE',  ( 34.47095863366522650, -11.93304594944324926, -18.87179757263150037 ) ) ;
#7969 = CARTESIAN_POINT ( 'NONE',  ( 16.21960234321935701, 7.070186740785398882, -14.59618053200276044 ) ) ;
#7970 = ORIENTED_EDGE ( 'NONE', *, *, #10245, .F. ) ;
#7971 = EDGE_LOOP ( 'NONE', ( #3587, #21904, #24806 ) ) ;
#7972 = DIRECTION ( 'NONE',  ( 0.000000000000000000, 0.000000000000000000, 1.000000000000000000 ) ) ;
#7973 = CARTESIAN_POINT ( 'NONE',  ( 25.64694198568010819, -13.68525919019184300, -15.02544717525507778 ) ) ;
#7974 = PLANE ( 'NONE',  #1911 ) ;
#7975 = DIRECTION ( 'NONE',  ( -0.5877852522924731371, -1.586114251531760728E-16, -0.8090169943749474513 ) ) ;
#7976 = VECTOR ( 'NONE', #28685, 1000.000000000000000 ) ;
#7977 = CARTESIAN_POINT ( 'NONE',  ( 23.93603600111211804, 0.1510904554606163908, -14.93755387302875448 ) ) ;
#7978 = CARTESIAN_POINT ( 'NONE',  ( 20.46796597391333350, 5.758383238370681667, -16.38968713894368534 ) ) ;
#7979 = ORIENTED_EDGE ( 'NONE', *, *, #26926, .F. ) ;
#7980 = EDGE_CURVE ( 'NONE', #8557, #6680, #7400, .T. ) ;
#7982 = VERTEX_POINT ( 'NONE', #14987 ) ;
#7981 = ADVANCED_FACE ( 'NONE', ( #23725 ), #2827, .T. ) ;
#7983 = CARTESIAN_POINT ( 'NONE',  ( 176.1922820468852819, -9.999999999999994671, -10.74328820663507678 ) ) ;
#7984 = AXIS2_PLACEMENT_3D ( 'NONE', #5020, #7468, #22636 ) ;
#7985 = CARTESIAN_POINT ( 'NONE',  ( 169.5152310637604671, -9.999999999999996447, -21.71180489736091346 ) ) ;
#7986 = DIRECTION ( 'NONE',  ( -0.7071067811865480168, 0.7071067811865470176, 0.000000000000000000 ) ) ;
#7987 = DIRECTION ( 'NONE',  ( -0.9510565162951536422, 0.000000000000000000, -0.3090169943749472292 ) ) ;
#7988 = FACE_OUTER_BOUND ( 'NONE', #14792, .T. ) ;
#7989 = CARTESIAN_POINT ( 'NONE',  ( 11.97192087863669663, 8.579774655713777065, -15.53257280409644991 ) ) ;
#7990 = CARTESIAN_POINT ( 'NONE',  ( 28.00362220295478721, -7.540254448315821811, -17.98007619878529439 ) ) ;
#7991 = CARTESIAN_POINT ( 'NONE',  ( 26.68443370873975340, -2.140902173977853540, -15.79004130932784555 ) ) ;
#7992 = EDGE_LOOP ( 'NONE', ( #13638, #4628, #7595, #24514 ) ) ;
#7993 = CARTESIAN_POINT ( 'NONE',  ( 161.1922820468853388, -1.999999999999973577, -13.59645775552055902 ) ) ;
#7994 = DIRECTION ( 'NONE',  ( 1.000000000000000000, 4.440892098500622217E-16, 0.000000000000000000 ) ) ;
#7995 = LINE ( 'NONE', #17014, #16526 ) ;
#7996 = CARTESIAN_POINT ( 'NONE',  ( 24.55500000000002103, 3.061616997868384620E-16, -2.500000000000001332 ) ) ;
#7997 = DIRECTION ( 'NONE',  ( 1.110223024625156540E-16, 2.995891024602366092E-32, 1.000000000000000000 ) ) ;
#7998 = CARTESIAN_POINT ( 'NONE',  ( 137.0152310637605524, -4.999999999999980460, -0.06116980274991495881 ) ) ;
#8000 = VERTEX_POINT ( 'NONE', #28946 ) ;
#7999 = CARTESIAN_POINT ( 'NONE',  ( 19.02541433733466647, 1.263421280649871248, -13.57496312174407826 ) ) ;
#8001 = ORIENTED_EDGE ( 'NONE', *, *, #21041, .F. ) ;
#8002 = CARTESIAN_POINT ( 'NONE',  ( 154.5152310637605240, -4.999999999999976019, -1.715463671822631530E-14 ) ) ;
#8003 = CARTESIAN_POINT ( 'NONE',  ( 12.27643783485070372, 9.496802808135052842, -15.31088501640310540 ) ) ;
#8004 = EDGE_CURVE ( 'NONE', #22761, #2119, #15287, .T. ) ;
#8005 = PLANE ( 'NONE',  #29615 ) ;
#8006 = LINE ( 'NONE', #24202, #10787 ) ;
#8007 = CARTESIAN_POINT ( 'NONE',  ( 19.68115760211910725, 3.144890361740488860, -20.29587546762095940 ) ) ;
#8008 = VECTOR ( 'NONE', #1935, 1000.000000000000000 ) ;
#8009 = CARTESIAN_POINT ( 'NONE',  ( 75.00000000000000000, 5.000000000000000000, -1.084202172485504434E-15 ) ) ;
#8010 = CARTESIAN_POINT ( 'NONE',  ( 21.96101381878726500, 3.467707295883769802, -19.37612211972275844 ) ) ;
#8011 = VERTEX_POINT ( 'NONE', #10571 ) ;
#8012 = DIRECTION ( 'NONE',  ( -0.5877852522924731371, -1.586114251531760235E-16, 0.8090169943749474513 ) ) ;
#8013 = CARTESIAN_POINT ( 'NONE',  ( 23.66316133457650750, -10.02594615916883392, -14.11990577516520595 ) ) ;
#8014 = CARTESIAN_POINT ( 'NONE',  ( 24.92117679868390923, -7.366661744264540346, -12.55155079749028779 ) ) ;
#8015 = EDGE_CURVE ( 'NONE', #27929, #29924, #24778, .T. ) ;
#8016 = EDGE_LOOP ( 'NONE', ( #15611, #15860, #6685, #17348, #3836, #17449, #8403, #22392, #11122, #8252, #1086, #21290, #25803, #22005, #9192, #808, #10050, #4346, #15757, #122, #1197, #28020, #6374, #13520, #7965, #13013, #18906, #22555, #18244, #14896, #15842, #7680, #29090, #28010, #1167, #544, #19403, #18129, #27669, #13287, #298, #21755, #16921, #21063 ) ) ;
#8017 = CARTESIAN_POINT ( 'NONE',  ( 24.68825858685077179, -9.385095155728059524, -16.92495907518576104 ) ) ;
#8018 = DIRECTION ( 'NONE',  ( 0.9510565162951536422, 0.000000000000000000, -0.3090169943749475623 ) ) ;
#8019 = ORIENTED_EDGE ( 'NONE', *, *, #12892, .T. ) ;
#8020 = VERTEX_POINT ( 'NONE', #22329 ) ;
#8021 = CARTESIAN_POINT ( 'NONE',  ( 142.0152310637606092, -10.00000000000000355, -15.61832212156129707 ) ) ;
#8022 = FACE_OUTER_BOUND ( 'NONE', #761, .T. ) ;
#8023 = AXIS2_PLACEMENT_3D ( 'NONE', #12116, #28950, #9672 ) ;
#8024 = LINE ( 'NONE', #8174, #2452 ) ;
#8025 = CARTESIAN_POINT ( 'NONE',  ( 33.33685173283005554, -10.38074443705513161, -18.09276096107157628 ) ) ;
#8026 = CARTESIAN_POINT ( 'NONE',  ( 10.56508425215480074, 13.43253182900300402, -16.23631622730588830 ) ) ;
#8027 = LINE ( 'NONE', #17336, #14162 ) ;
#8028 = DIRECTION ( 'NONE',  ( 0.3090169943749475623, 8.338696094058001131E-17, 0.9510565162951536422 ) ) ;
#8029 = CARTESIAN_POINT ( 'NONE',  ( 9.661885998671275289, 16.25481316389105402, -17.91482063482849441 ) ) ;
#8030 = CARTESIAN_POINT ( 'NONE',  ( 167.0152310637604387, -9.999999999999998224, -8.721423840594312082 ) ) ;
#8031 = ORIENTED_EDGE ( 'NONE', *, *, #7599, .T. ) ;
#8032 = DIRECTION ( 'NONE',  ( 0.9510565162951536422, 2.566386769018988816E-16, 0.3090169943749472292 ) ) ;
#8033 = ADVANCED_FACE ( 'NONE', ( #6001 ), #24621, .T. ) ;
#8034 = EDGE_CURVE ( 'NONE', #7222, #27929, #20072, .T. ) ;
#8035 = VERTEX_POINT ( 'NONE', #10721 ) ;
#8036 = CARTESIAN_POINT ( 'NONE',  ( 144.5152310637606092, -4.999999999999978684, -19.94844914048349693 ) ) ;
#8037 = DIRECTION ( 'NONE',  ( -1.000000000000000000, -0.000000000000000000, -0.000000000000000000 ) ) ;
#8038 = EDGE_CURVE ( 'NONE', #29180, #10203, #13014, .T. ) ;
#8039 = DIRECTION ( 'NONE',  ( -0.9510565162951536422, -2.566386769018988816E-16, -0.3090169943749472292 ) ) ;
#8040 = ORIENTED_EDGE ( 'NONE', *, *, #1414, .T. ) ;
#8041 = VERTEX_POINT ( 'NONE', #21873 ) ;
#8042 = CARTESIAN_POINT ( 'NONE',  ( 13.35290877858212255, 7.614465999429414822, -15.72913170295453966 ) ) ;
#8043 = CARTESIAN_POINT ( 'NONE',  ( 13.23210690081759111, 9.952263081781872245, -14.54667289943505004 ) ) ;
#8044 = CARTESIAN_POINT ( 'NONE',  ( 26.06583011202948441, -9.749651170145462231, -12.94692625511877182 ) ) ;
#8045 = CARTESIAN_POINT ( 'NONE',  ( 137.2287565553230309, -1.999999999999979572, -20.83012701892220164 ) ) ;
#8046 = DIRECTION ( 'NONE',  ( 0.9510565162951535312, 2.566386769018988816E-16, -0.3090169943749475623 ) ) ;
#8047 = AXIS2_PLACEMENT_3D ( 'NONE', #3988, #3838, #13130 ) ;
#8048 = CARTESIAN_POINT ( 'NONE',  ( 174.7287565553228319, -9.999999999999996447, 0.8205080756887930260 ) ) ;
#8049 = ORIENTED_EDGE ( 'NONE', *, *, #20921, .F. ) ;
#8050 = ORIENTED_EDGE ( 'NONE', *, *, #4948, .T. ) ;
#8051 = DIRECTION ( 'NONE',  ( -2.698458740408365879E-16, 1.000000000000000000, 0.000000000000000000 ) ) ;
#8052 = LINE ( 'NONE', #22101, #17976 ) ;
#8053 = CARTESIAN_POINT ( 'NONE',  ( -19.99999999999999645, 55.00000000000000711, -30.00000000000000711 ) ) ;
#8054 = CARTESIAN_POINT ( 'NONE',  ( 13.00000000000000178, -2.870178842070716726E-15, -23.00000000000000000 ) ) ;
#8055 = CARTESIAN_POINT ( 'NONE',  ( 12.98644063677341798, 8.526496012441747041, -16.01999686492960961 ) ) ;
#8056 = ORIENTED_EDGE ( 'NONE', *, *, #18721, .F. ) ;
#8057 = CARTESIAN_POINT ( 'NONE',  ( 35.54859390953724585, -22.18451583373416014, -17.99055332684694974 ) ) ;
#8058 = EDGE_LOOP ( 'NONE', ( #16856, #11635, #22345, #5630 ) ) ;
#8059 = VECTOR ( 'NONE', #3686, 1000.000000000000000 ) ;
#8060 = CARTESIAN_POINT ( 'NONE',  ( 9.112135424753279977, 16.18318370314694832, -17.05489040841110437 ) ) ;
#8061 = VECTOR ( 'NONE', #14100, 1000.000000000000000 ) ;
#8062 = CARTESIAN_POINT ( 'NONE',  ( 26.61709978538234012, -3.831456866606135492, -17.85214630790261836 ) ) ;
#8063 = CARTESIAN_POINT ( 'NONE',  ( 12.83225436833568089, 9.540613290865683993, -16.14103841883858337 ) ) ;
#8064 = FACE_BOUND ( 'NONE', #15416, .T. ) ;
#8065 = EDGE_CURVE ( 'NONE', #30101, #11857, #5855, .T. ) ;
#8066 = ORIENTED_EDGE ( 'NONE', *, *, #23169, .F. ) ;
#8067 = FACE_OUTER_BOUND ( 'NONE', #14591, .T. ) ;
#8068 = ADVANCED_FACE ( 'NONE', ( #3418 ), #22029, .T. ) ;
#8069 = CARTESIAN_POINT ( 'NONE',  ( 12.49664108868010182, 8.569232744350554043, -15.13285098609708790 ) ) ;
#8070 = CARTESIAN_POINT ( 'NONE',  ( 152.0152310637605808, -4.999999999999976019, -24.27857615940569502 ) ) ;
#8071 = EDGE_CURVE ( 'NONE', #26570, #29971, #29242, .T. ) ;
#8072 = ORIENTED_EDGE ( 'NONE', *, *, #7802, .F. ) ;
#8073 = CARTESIAN_POINT ( 'NONE',  ( 169.5152310637605240, -1.999999999999970024, -28.60870317832789667 ) ) ;
#8074 = VERTEX_POINT ( 'NONE', #17731 ) ;
#8075 = CARTESIAN_POINT ( 'NONE',  ( 12.03623766312057519, 9.280706639558555793, -16.68777662621714342 ) ) ;
#8076 = AXIS2_PLACEMENT_3D ( 'NONE', #5911, #11077, #22990 ) ;
#8077 = ORIENTED_EDGE ( 'NONE', *, *, #6372, .T. ) ;
#8078 = CARTESIAN_POINT ( 'NONE',  ( 15.44177808481316383, 7.494736869644298416, -14.00399691429678306 ) ) ;
#8079 = CARTESIAN_POINT ( 'NONE',  ( 18.26079443319284934, -0.1287745640203900310, -14.06839115638798354 ) ) ;
#8080 = VECTOR ( 'NONE', #19332, 1000.000000000000000 ) ;
#8081 = CARTESIAN_POINT ( 'NONE',  ( 98.03139517864238428, -4.999999999999991118, -71.22397767698338100 ) ) ;
#8082 = CARTESIAN_POINT ( 'NONE',  ( 36.02474454408307736, -19.83113812547715682, -20.43161669954002591 ) ) ;
#8083 = PRODUCT_CONTEXT ( 'NONE', #12991, 'mechanical' ) ;
#8084 = CARTESIAN_POINT ( 'NONE',  ( 20.92249676953290916, 2.861121271339598593, -14.71414025844469720 ) ) ;
#8085 = VECTOR ( 'NONE', #6512, 1000.000000000000000 ) ;
#8086 = CARTESIAN_POINT ( 'NONE',  ( 19.52227536296714305, 7.868296793410291201, -18.00468392081665669 ) ) ;
#8087 = CARTESIAN_POINT ( 'NONE',  ( 146.1922820468853956, -4.999999999999978684, -4.936203717676158398 ) ) ;
#8088 = FACE_BOUND ( 'NONE', #22615, .T. ) ;
#8089 = AXIS2_PLACEMENT_3D ( 'NONE', #30199, #11657, #12113 ) ;
#8090 = ORIENTED_EDGE ( 'NONE', *, *, #12799, .F. ) ;
#8091 = FACE_OUTER_BOUND ( 'NONE', #764, .T. ) ;
#8092 = CARTESIAN_POINT ( 'NONE',  ( 173.6922820468853672, -4.999999999999969802, -32.39392330124607611 ) ) ;
#8093 = FACE_OUTER_BOUND ( 'NONE', #17562, .T. ) ;
#8094 = CARTESIAN_POINT ( 'NONE',  ( 13.00000000000000178, 0.000000000000000000, 4.999999999999998224 ) ) ;
#8095 = AXIS2_PLACEMENT_3D ( 'NONE', #28513, #14111, #23443 ) ;
#8096 = CARTESIAN_POINT ( 'NONE',  ( 11.75823633891744535, 11.87334092381181883, -15.52517956378672359 ) ) ;
#8097 = LINE ( 'NONE', #15112, #1694 ) ;
#8098 = ORIENTED_EDGE ( 'NONE', *, *, #10062, .F. ) ;
#8099 = CARTESIAN_POINT ( 'NONE',  ( 159.5152310637604671, -10.00000000000000000, -2.627941064794695691 ) ) ;
#8100 = EDGE_LOOP ( 'NONE', ( #10433, #9885, #5203, #23276 ) ) ;
#8101 = CIRCLE ( 'NONE', #25184, 5.000000000000000888 ) ;
#8102 = CARTESIAN_POINT ( 'NONE',  ( 11.47652547240386944, 9.253065934422213701, -15.85936358228339316 ) ) ;
#8103 = VERTEX_POINT ( 'NONE', #8276 ) ;
#8104 = EDGE_CURVE ( 'NONE', #17985, #22052, #27091, .T. ) ;
#8105 = VECTOR ( 'NONE', #3881, 1000.000000000000000 ) ;
#8106 = CARTESIAN_POINT ( 'NONE',  ( 10.66857885413002727, 9.045135741668604012, -16.41124387233542592 ) ) ;
#8107 = DIRECTION ( 'NONE',  ( 1.000000000000000000, 0.000000000000000000, -0.000000000000000000 ) ) ;
#8108 = DIRECTION ( 'NONE',  ( 0.000000000000000000, -2.775557561562890735E-17, 1.000000000000000000 ) ) ;
#8109 = ADVANCED_FACE ( 'NONE', ( #12708 ), #26783, .T. ) ;
#8110 = ADVANCED_FACE ( 'NONE', ( #10416 ), #22485, .T. ) ;
#8111 = EDGE_LOOP ( 'NONE', ( #9253, #20031, #28862, #22428 ) ) ;
#8112 = CARTESIAN_POINT ( 'NONE',  ( 138.6922820468854525, -10.00000000000000533, -6.413161187712876909 ) ) ;
#8113 = ADVANCED_FACE ( 'NONE', ( #8130 ), #11779, .T. ) ;
#8114 = ORIENTED_EDGE ( 'NONE', *, *, #24105, .F. ) ;
#8115 = CARTESIAN_POINT ( 'NONE',  ( 12.82210747586494293, 9.587147947373788170, -16.14523453761016825 ) ) ;
#8116 = ORIENTED_EDGE ( 'NONE', *, *, #15206, .F. ) ;
#8117 = CARTESIAN_POINT ( 'NONE',  ( 36.14373538984320078, -19.36570096427324827, -19.42526322947885475 ) ) ;
#8118 = CARTESIAN_POINT ( 'NONE',  ( 19.68115760211910725, 3.144890361740488860, -20.29587546762095940 ) ) ;
#8119 = EDGE_LOOP ( 'NONE', ( #16741, #18322, #16776, #6025 ) ) ;
#8120 = PRODUCT_DEFINITION_SHAPE ( 'NONE', 'NONE',  #30272 ) ;
#8121 = CARTESIAN_POINT ( 'NONE',  ( 139.7287565553230309, -1.999999999999978684, -16.50000000000000000 ) ) ;
#8122 = CARTESIAN_POINT ( 'NONE',  ( 26.55441479597953247, -12.51626325376082249, -18.99724541349076645 ) ) ;
#8123 = FACE_OUTER_BOUND ( 'NONE', #16841, .T. ) ;
#8124 = CARTESIAN_POINT ( 'NONE',  ( 163.6922820468853388, -9.999999999999998224, -15.07341522555727664 ) ) ;
#8125 = ORIENTED_EDGE ( 'NONE', *, *, #2218, .T. ) ;
#8126 = CARTESIAN_POINT ( 'NONE',  ( 20.31878617967674217, -0.6648838724932636390, -18.90140657046049455 ) ) ;
#8127 = CARTESIAN_POINT ( 'NONE',  ( 22.27366892561238387, -0.4200048385588530664, -12.54648181008633934 ) ) ;
#8128 = VECTOR ( 'NONE', #4939, 1000.000000000000000 ) ;
#8129 = VERTEX_POINT ( 'NONE', #10867 ) ;
#8130 = FACE_OUTER_BOUND ( 'NONE', #24364, .T. ) ;
#8131 = VECTOR ( 'NONE', #17860, 1000.000000000000000 ) ;
#8132 = CARTESIAN_POINT ( 'NONE',  ( 148.6922820468854241, -1.999999999999977129, -23.73366926340167637 ) ) ;
#8133 = AXIS2_PLACEMENT_3D ( 'NONE', #5456, #14143, #5149 ) ;
#8134 = CARTESIAN_POINT ( 'NONE',  ( 2.500000000000000444, 0.000000000000000000, 2.041999999999999815 ) ) ;
#8135 = CARTESIAN_POINT ( 'NONE',  ( 136.1922820468854241, -1.999999999999980016, -10.74328820663507322 ) ) ;
#8136 = CARTESIAN_POINT ( 'NONE',  ( -4.000000000000020428, -6.928203230275511437, -5.000000000000000888 ) ) ;
#8137 = CARTESIAN_POINT ( 'NONE',  ( -20.00000000000017053, 34.64101615137744972, -10.00000000000000000 ) ) ;
#8138 = CARTESIAN_POINT ( 'NONE',  ( 10.24089172292967298, 14.91932009296530559, -16.37038124228770997 ) ) ;
#8139 = CARTESIAN_POINT ( 'NONE',  ( 15.46244301724551740, 3.702889819443702990, -17.82701508041758842 ) ) ;
#8140 = CARTESIAN_POINT ( 'NONE',  ( 26.68716238812262631, -2.792712658874448639, -18.04699283665395981 ) ) ;
#8141 = VERTEX_POINT ( 'NONE', #17589 ) ;
#8142 = CYLINDRICAL_SURFACE ( 'NONE', #21760, 2.000000000000000000 ) ;
#8143 = FACE_OUTER_BOUND ( 'NONE', #19526, .T. ) ;
#8144 = DIRECTION ( 'NONE',  ( -2.698458740408365879E-16, 1.000000000000000000, 0.000000000000000000 ) ) ;
#8145 = LINE ( 'NONE', #3583, #23924 ) ;
#8146 = ADVANCED_FACE ( 'NONE', ( #29557 ), #29410, .T. ) ;
#8147 = MECHANICAL_DESIGN_GEOMETRIC_PRESENTATION_REPRESENTATION (  '', ( #28653 ), #25224 ) ;
#8148 = CARTESIAN_POINT ( 'NONE',  ( 0.000000000000000000, 0.000000000000000000, 9.999999999999998224 ) ) ;
#8149 = EDGE_CURVE ( 'NONE', #26798, #27886, #19579, .T. ) ;
#8150 = CARTESIAN_POINT ( 'NONE',  ( 22.89472691350227507, 1.279074496056108901, -19.72372301458170796 ) ) ;
#8151 = VERTEX_POINT ( 'NONE', #15599 ) ;
#8152 = CARTESIAN_POINT ( 'NONE',  ( 129.5152310637605524, -10.00000000000000888, -13.05155085951650840 ) ) ;
#8153 = EDGE_CURVE ( 'NONE', #29449, #13920, #22941, .T. ) ;
#8154 = CARTESIAN_POINT ( 'NONE',  ( 12.27549906412561675, 9.499463866199420181, -15.31139863700699344 ) ) ;
#8155 = VECTOR ( 'NONE', #24611, 1000.000000000000000 ) ;
#8156 = DIRECTION ( 'NONE',  ( 1.000000000000000000, 2.698458740408365879E-16, -1.110223024625156540E-16 ) ) ;
#8157 = CARTESIAN_POINT ( 'NONE',  ( 144.5152310637606092, -10.00000000000000178, -19.94844914048349693 ) ) ;
#8158 = CARTESIAN_POINT ( 'NONE',  ( 21.40051611374530793, -0.1690565882708310874, -20.18282279970310000 ) ) ;
#8159 = CARTESIAN_POINT ( 'NONE',  ( 166.1922820468853672, -1.999999999999971356, -30.91696583120936026 ) ) ;
#8160 = CARTESIAN_POINT ( 'NONE',  ( 19.48958755759471728, 3.937961857331544469, -13.19130291127160959 ) ) ;
#8161 = ORIENTED_EDGE ( 'NONE', *, *, #26597, .T. ) ;
#8162 = DIRECTION ( 'NONE',  ( 1.000000000000000000, 4.440892098500622217E-16, 0.000000000000000000 ) ) ;
#8163 = CARTESIAN_POINT ( 'NONE',  ( 25.29949251596307036, -5.094144391296384633, -13.01082609127739076 ) ) ;
#8164 = CARTESIAN_POINT ( 'NONE',  ( 22.29950228926167100, 0.3472756386405770335, -13.33132414558515677 ) ) ;
#8165 = CARTESIAN_POINT ( 'NONE',  ( 26.92971693216691165, -8.617903733377630715, -13.36642543767191427 ) ) ;
#8166 = VECTOR ( 'NONE', #12807, 1000.000000000000000 ) ;
#8167 = DIRECTION ( 'NONE',  ( -2.908569913943825554E-16, 1.000000000000000000, -0.000000000000000000 ) ) ;
#8168 = EDGE_CURVE ( 'NONE', #12771, #18151, #4012, .T. ) ;
#8169 = ORIENTED_EDGE ( 'NONE', *, *, #11209, .F. ) ;
#8170 = VECTOR ( 'NONE', #19417, 1000.000000000000000 ) ;
#8171 = DIRECTION ( 'NONE',  ( 0.000000000000000000, 0.000000000000000000, -1.000000000000000000 ) ) ;
#8172 = DIRECTION ( 'NONE',  ( -2.698458740408365879E-16, 1.000000000000000000, 0.000000000000000000 ) ) ;
#8173 = DIRECTION ( 'NONE',  ( -2.698458740408365879E-16, 1.000000000000000000, 0.000000000000000000 ) ) ;
#8174 = CARTESIAN_POINT ( 'NONE',  ( 90.99818021113283351, -4.999999999999992895, 66.11404789448386055 ) ) ;
#8175 = CARTESIAN_POINT ( 'NONE',  ( 36.21530066971708095, -20.68720585756345187, -20.37220581101806971 ) ) ;
#8176 = CARTESIAN_POINT ( 'NONE',  ( 9.924804006935172396, 16.36893865032855899, -16.50109463189289016 ) ) ;
#8177 = CARTESIAN_POINT ( 'NONE',  ( 161.1922820468853104, -4.999999999999973355, -2.083034168790677043 ) ) ;
#8178 = CARTESIAN_POINT ( 'NONE',  ( 46.75000000000000000, -1.387778780781445676E-16, 5.000000000000000888 ) ) ;
#8179 = CARTESIAN_POINT ( 'NONE',  ( 13.12425544150138279, 8.571136816377206813, -15.91139631635614471 ) ) ;
#8180 = DIRECTION ( 'NONE',  ( -2.698458740408365879E-16, 1.000000000000000000, 0.000000000000000000 ) ) ;
#8181 = ORIENTED_EDGE ( 'NONE', *, *, #23456, .F. ) ;
#8182 = DIRECTION ( 'NONE',  ( 0.9510565162951536422, 2.566386769018988816E-16, 0.3090169943749472292 ) ) ;
#8183 = ORIENTED_EDGE ( 'NONE', *, *, #28413, .F. ) ;
#8184 = CARTESIAN_POINT ( 'NONE',  ( 169.5152310637604955, -1.999999999999970468, -19.94844914048349693 ) ) ;
#8185 = CARTESIAN_POINT ( 'NONE',  ( 142.0152310637605808, -1.999999999999978018, -34.70218595412750773 ) ) ;
#8186 = ORIENTED_EDGE ( 'NONE', *, *, #12796, .T. ) ;
#8187 = AXIS2_PLACEMENT_3D ( 'NONE', #12075, #7504, #24139 ) ;
#8188 = DIRECTION ( 'NONE',  ( 0.9510565162951536422, 2.566386769018988816E-16, 0.3090169943749472292 ) ) ;
#8189 = ORIENTED_EDGE ( 'NONE', *, *, #15408, .F. ) ;
#8190 = ORIENTED_EDGE ( 'NONE', *, *, #4435, .F. ) ;
#8191 = EDGE_LOOP ( 'NONE', ( #6884, #5679, #11382, #14263 ) ) ;
#8192 = CARTESIAN_POINT ( 'NONE',  ( 13.51537010444165254, 7.685947621549766851, -15.59967102646339043 ) ) ;
#8193 = AXIS2_PLACEMENT_3D ( 'NONE', #14601, #3046, #1057 ) ;
#8194 = CARTESIAN_POINT ( 'NONE',  ( 12.96291568738609890, 5.695260009123724210, -16.43886026595064109 ) ) ;
#8195 = CARTESIAN_POINT ( 'NONE',  ( 28.73289915209718615, -4.972737245092835323, -15.12275039236161689 ) ) ;
#8196 = DIRECTION ( 'NONE',  ( -2.698458740408365879E-16, 1.000000000000000000, 0.000000000000000000 ) ) ;
#8197 = DIRECTION ( 'NONE',  ( -2.698458740408365879E-16, 1.000000000000000000, 0.000000000000000000 ) ) ;
#8198 = LINE ( 'NONE', #5930, #15227 ) ;
#8199 = ORIENTED_EDGE ( 'NONE', *, *, #6496, .T. ) ;
#8200 = LINE ( 'NONE', #27476, #4531 ) ;
#8201 = EDGE_CURVE ( 'NONE', #28125, #20055, #30159, .T. ) ;
#8203 = VERTEX_POINT ( 'NONE', #11320 ) ;
#8202 = DIRECTION ( 'NONE',  ( -0.5877852522924731371, -1.586114251531760728E-16, -0.8090169943749474513 ) ) ;
#8204 = DIRECTION ( 'NONE',  ( -0.5877852522924731371, 0.000000000000000000, 0.8090169943749474513 ) ) ;
#8205 = DIRECTION ( 'NONE',  ( -2.698458740408365879E-16, 1.000000000000000000, 0.000000000000000000 ) ) ;
#8206 = CARTESIAN_POINT ( 'NONE',  ( 13.11714404544056656, 8.568033937426095648, -15.91706119101506545 ) ) ;
#8207 = ORIENTED_EDGE ( 'NONE', *, *, #22743, .F. ) ;
#8208 = CARTESIAN_POINT ( 'NONE',  ( 33.71394559998177698, -12.94241281914233355, -18.76105684162217457 ) ) ;
#8209 = VECTOR ( 'NONE', #29634, 1000.000000000000000 ) ;
#8210 = EDGE_LOOP ( 'NONE', ( #28858, #15511, #26210, #23590 ) ) ;
#8211 = CARTESIAN_POINT ( 'NONE',  ( 10.34450975306715570, 10.53135794231081057, -16.54525784588868120 ) ) ;
#8212 = ORIENTED_EDGE ( 'NONE', *, *, #2645, .T. ) ;
#8213 = CARTESIAN_POINT ( 'NONE',  ( 22.90372073960079646, -4.505259139820817715, -13.75793632099288111 ) ) ;
#8214 = CARTESIAN_POINT ( 'NONE',  ( 12.86826794643883609, 9.516041646402381815, -16.11542282846662388 ) ) ;
#8215 = FACE_BOUND ( 'NONE', #10855, .T. ) ;
#8216 = VECTOR ( 'NONE', #3344, 1000.000000000000000 ) ;
#8217 = ORIENTED_EDGE ( 'NONE', *, *, #6826, .F. ) ;
#8218 = VECTOR ( 'NONE', #11818, 1000.000000000000000 ) ;
#8219 = EDGE_LOOP ( 'NONE', ( #28152, #19450, #21967, #27077 ) ) ;
#8220 = DIRECTION ( 'NONE',  ( -0.5877852522924731371, 0.000000000000000000, 0.8090169943749474513 ) ) ;
#8221 = CARTESIAN_POINT ( 'NONE',  ( 12.49977518293622758, 8.570603418560722275, -15.13035415120363325 ) ) ;
#8222 = LINE ( 'NONE', #12955, #6721 ) ;
#8223 = ORIENTED_EDGE ( 'NONE', *, *, #12974, .F. ) ;
#8224 = DIRECTION ( 'NONE',  ( 0.3090169943749472292, 8.338696094057992503E-17, -0.9510565162951536422 ) ) ;
#8225 = ORIENTED_EDGE ( 'NONE', *, *, #21094, .T. ) ;
#8226 = CARTESIAN_POINT ( 'NONE',  ( 13.06976498004312326, 8.549601185932660385, -15.95463209657921055 ) ) ;
#8227 = ORIENTED_EDGE ( 'NONE', *, *, #8456, .F. ) ;
#8228 = CARTESIAN_POINT ( 'NONE',  ( 13.97862894411929879, 7.467096638697104716, -19.56757695884047621 ) ) ;
#8229 = CARTESIAN_POINT ( 'NONE',  ( 14.77169846916584461, 3.272981165966227568, -18.54959716842853723 ) ) ;
#8230 = DIRECTION ( 'NONE',  ( 0.000000000000000000, 0.000000000000000000, -1.000000000000000000 ) ) ;
#8231 = EDGE_LOOP ( 'NONE', ( #1418, #5947, #25909, #26495, #5041 ) ) ;
#8232 = CARTESIAN_POINT ( 'NONE',  ( 36.44920892064849482, -21.73803172434679354, -19.68085951391205057 ) ) ;
#8233 = AXIS2_PLACEMENT_3D ( 'NONE', #4016, #9327, #11176 ) ;
#8234 = CARTESIAN_POINT ( 'NONE',  ( 17.95327243003904982, 7.812726124483462264, -14.88485059575767266 ) ) ;
#8235 = EDGE_LOOP ( 'NONE', ( #6189, #25865, #26058, #24971, #5509, #13845 ) ) ;
#8236 = VECTOR ( 'NONE', #1001, 1000.000000000000000 ) ;
#8237 = DIRECTION ( 'NONE',  ( -0.5877852522924731371, 0.000000000000000000, 0.8090169943749474513 ) ) ;
#8238 = ADVANCED_FACE ( 'NONE', ( #13455 ), #30007, .F. ) ;
#8239 = FACE_BOUND ( 'NONE', #3954, .T. ) ;
#8240 = EDGE_CURVE ( 'NONE', #6979, #134, #25071, .T. ) ;
#8241 = ADVANCED_FACE ( 'NONE', ( #27698 ), #20478, .T. ) ;
#8242 = EDGE_CURVE ( 'NONE', #13963, #29180, #18190, .T. ) ;
#8243 = ORIENTED_EDGE ( 'NONE', *, *, #12552, .T. ) ;
#8244 = DIRECTION ( 'NONE',  ( -0.5877852522924731371, 0.000000000000000000, 0.8090169943749474513 ) ) ;
#8245 = CARTESIAN_POINT ( 'NONE',  ( 32.12153525177792091, -10.97127362787143312, -16.88978156643115724 ) ) ;
#8246 = DIRECTION ( 'NONE',  ( 0.000000000000000000, -1.000000000000000000, 0.000000000000000000 ) ) ;
#8247 = ORIENTED_EDGE ( 'NONE', *, *, #4090, .T. ) ;
#8248 = DIRECTION ( 'NONE',  ( 1.000000000000000000, 2.908569913943825554E-16, -6.938893903907227392E-16 ) ) ;
#8249 = CARTESIAN_POINT ( 'NONE',  ( 11.05541542350396256, 17.68942290035798237, -17.91468072056456862 ) ) ;
#8250 = ORIENTED_EDGE ( 'NONE', *, *, #15791, .F. ) ;
#8251 = CYLINDRICAL_SURFACE ( 'NONE', #3698, 13.00000000000000178 ) ;
#8252 = ORIENTED_EDGE ( 'NONE', *, *, #20668, .F. ) ;
#8253 = CARTESIAN_POINT ( 'NONE',  ( 141.1922820468854241, -10.00000000000000533, -2.083034168790677043 ) ) ;
#8254 = ORIENTED_EDGE ( 'NONE', *, *, #16529, .F. ) ;
#8255 = CARTESIAN_POINT ( 'NONE',  ( 12.62682997171803123, 7.576475742438638861, -15.02849783152220908 ) ) ;
#8256 = FACE_OUTER_BOUND ( 'NONE', #19531, .T. ) ;
#8257 = CARTESIAN_POINT ( 'NONE',  ( -1.310841663519413114, 0.000000000000000000, 0.000000000000000000 ) ) ;
#8258 = CIRCLE ( 'NONE', #26821, 5.000000000000000000 ) ;
#8259 = ORIENTED_EDGE ( 'NONE', *, *, #5599, .F. ) ;
#8260 = LINE ( 'NONE', #12536, #25654 ) ;
#8261 = VERTEX_POINT ( 'NONE', #11017 ) ;
#8262 = CARTESIAN_POINT ( 'NONE',  ( 12.83227036137552446, 9.540540802112166929, -16.14103173976383587 ) ) ;
#8263 = CARTESIAN_POINT ( 'NONE',  ( 33.90312036197754963, -11.11655558909185615, -17.69153855583423862 ) ) ;
#8264 = CARTESIAN_POINT ( 'NONE',  ( 22.90372073960079646, -4.505259139820817715, -13.75793632099288111 ) ) ;
#8265 = ORIENTED_EDGE ( 'NONE', *, *, #11109, .T. ) ;
#8266 = ORIENTED_EDGE ( 'NONE', *, *, #18637, .T. ) ;
#8267 = CARTESIAN_POINT ( 'NONE',  ( 5.000000000000002665, 0.000000000000000000, -2.700000000000001066 ) ) ;
#8268 = CARTESIAN_POINT ( 'NONE',  ( 15.17188473929424930, 6.803351907998973935, -20.50413427079521256 ) ) ;
#8269 = VERTEX_POINT ( 'NONE', #16045 ) ;
#8270 = LINE ( 'NONE', #5995, #4238 ) ;
#8271 = EDGE_CURVE ( 'NONE', #11681, #15913, #29868, .T. ) ;
#8272 = CARTESIAN_POINT ( 'NONE',  ( 19.60850488237918654, -1.635242255716521820, -15.65509664672261003 ) ) ;
#8273 = CARTESIAN_POINT ( 'NONE',  ( 23.16986854814090080, 3.028408164773654931, -18.83379972368585342 ) ) ;
#8274 = PRESENTATION_LAYER_ASSIGNMENT (  '', '', ( #20957 ) ) ;
#8275 = ORIENTED_EDGE ( 'NONE', *, *, #24701, .F. ) ;
#8276 = CARTESIAN_POINT ( 'NONE',  ( -2.928571428571429713, -9.419004090963149730E-16, 1.700000000000000178 ) ) ;
#8277 = AXIS2_PLACEMENT_3D ( 'NONE', #17789, #15951, #18243 ) ;
#8278 = ADVANCED_FACE ( 'NONE', ( #27253 ), #2189, .T. ) ;
#8279 = CARTESIAN_POINT ( 'NONE',  ( 142.0152310637605240, -4.999999999999979572, -1.576685793744486963E-14 ) ) ;
#8280 = EDGE_CURVE ( 'NONE', #13743, #3391, #5478, .T. ) ;
#8281 = EDGE_CURVE ( 'NONE', #25250, #16634, #6600, .T. ) ;
#8282 = AXIS2_PLACEMENT_3D ( 'NONE', #2269, #25306, #29942 ) ;
#8283 = CARTESIAN_POINT ( 'NONE',  ( 174.5152310637604955, -9.999999999999994671, -28.60870317832789667 ) ) ;
#8284 = EDGE_CURVE ( 'NONE', #28008, #29920, #4311, .T. ) ;
#8285 = CARTESIAN_POINT ( 'NONE',  ( 146.1922820468854525, -1.999999999999977129, -22.25671179336496053 ) ) ;
#8286 = DIRECTION ( 'NONE',  ( -0.000000000000000000, -0.000000000000000000, -1.000000000000000000 ) ) ;
#8287 = CARTESIAN_POINT ( 'NONE',  ( 151.1922820468853672, -10.00000000000000178, -2.083034168790677043 ) ) ;
#8288 = CARTESIAN_POINT ( 'NONE',  ( 11.21994398240249957, 9.109360644301018439, -17.24323810967081982 ) ) ;
#8289 = CARTESIAN_POINT ( 'NONE',  ( 11.47310491742633687, 9.268236560789974376, -15.86081749295074594 ) ) ;
#8291 = VECTOR ( 'NONE', #841, 1000.000000000000000 ) ;
#8290 = CARTESIAN_POINT ( 'NONE',  ( 30.07542022419311678, -8.155067017681195907, -14.09159111155252120 ) ) ;
#8292 = ORIENTED_EDGE ( 'NONE', *, *, #11151, .F. ) ;
#8293 = DIRECTION ( 'NONE',  ( 0.3090169943749475623, 8.338696094058001131E-17, 0.9510565162951536422 ) ) ;
#8294 = DIRECTION ( 'NONE',  ( -1.110223024625156540E-16, 0.000000000000000000, -1.000000000000000000 ) ) ;
#8295 = CARTESIAN_POINT ( 'NONE',  ( 152.0152310637604671, -4.999999999999976907, -17.38167787843870826 ) ) ;
#8296 = AXIS2_PLACEMENT_3D ( 'NONE', #17892, #22347, #17605 ) ;
#8297 = CARTESIAN_POINT ( 'NONE',  ( 148.6922820468854525, -10.00000000000000178, -32.39392330124607611 ) ) ;
#8298 = DIRECTION ( 'NONE',  ( 0.9510565162951536422, 2.566386769018988816E-16, 0.3090169943749472292 ) ) ;
#8299 =( NAMED_UNIT ( * ) SI_UNIT ( $, .STERADIAN. ) SOLID_ANGLE_UNIT ( ) );
#8300 = CARTESIAN_POINT ( 'NONE',  ( 18.34549112274340033, 0.9605221043122941227, -13.99314825615798341 ) ) ;
#8301 = VERTEX_POINT ( 'NONE', #11458 ) ;
#8302 = LINE ( 'NONE', #17757, #27129 ) ;
#8303 = CARTESIAN_POINT ( 'NONE',  ( 10.85049725708738855, 16.03634806290433801, -15.90056160573019284 ) ) ;
#8304 = VECTOR ( 'NONE', #25486, 1000.000000000000000 ) ;
#8305 = CARTESIAN_POINT ( 'NONE',  ( 125.7287565553229740, -84.33034373659255323, 0.5000000000000143219 ) ) ;
#8306 = FACE_OUTER_BOUND ( 'NONE', #20012, .T. ) ;
#8307 = ORIENTED_EDGE ( 'NONE', *, *, #7157, .F. ) ;
#8308 = CARTESIAN_POINT ( 'NONE',  ( 20.52488529563827058, 3.974637744936419637, -19.97762432673833288 ) ) ;
#8309 = DIRECTION ( 'NONE',  ( 0.9510565162951535312, 2.566386769018988816E-16, -0.3090169943749475623 ) ) ;
#8310 = CARTESIAN_POINT ( 'NONE',  ( 15.95545008109832530, 6.956385541780823800, -13.20154910664163950 ) ) ;
#8311 = ORIENTED_EDGE ( 'NONE', *, *, #16565, .T. ) ;
#8312 = LINE ( 'NONE', #3451, #10535 ) ;
#8313 = FILL_AREA_STYLE_COLOUR ( '', #13662 ) ;
#8314 = CARTESIAN_POINT ( 'NONE',  ( 27.35338705259445646, -4.307586880325415812, -13.99634582963401996 ) ) ;
#8315 = CARTESIAN_POINT ( 'NONE',  ( 27.86916612644401425, -2.348388412649441648, -16.97020329177912501 ) ) ;
#8316 =( REPRESENTATION_RELATIONSHIP ('NONE','NONE', #5250, #19847 ) REPRESENTATION_RELATIONSHIP_WITH_TRANSFORMATION ( #7646 )SHAPE_REPRESENTATION_RELATIONSHIP( ) );
#8317 = ORIENTED_EDGE ( 'NONE', *, *, #4317, .F. ) ;
#8318 = AXIS2_PLACEMENT_3D ( 'NONE', #28696, #12770, #22088 ) ;
#8319 = DIRECTION ( 'NONE',  ( 1.110223024625156540E-16, 2.995891024602366092E-32, 1.000000000000000000 ) ) ;
#8320 = VECTOR ( 'NONE', #22087, 1000.000000000000000 ) ;
#8321 = EDGE_CURVE ( 'NONE', #23103, #9904, #18495, .T. ) ;
#8322 = ADVANCED_FACE ( 'NONE', ( #17874 ), #27404, .T. ) ;
#8323 = EDGE_CURVE ( 'NONE', #11701, #27580, #23047, .T. ) ;
#8324 = LINE ( 'NONE', #25712, #27026 ) ;
#8325 = EDGE_CURVE ( 'NONE', #24130, #13154, #1734, .T. ) ;
#8326 =( GEOMETRIC_REPRESENTATION_CONTEXT ( 3 ) GLOBAL_UNCERTAINTY_ASSIGNED_CONTEXT ( ( #18658 ) ) GLOBAL_UNIT_ASSIGNED_CONTEXT ( ( #15634, #16691, #18824 ) ) REPRESENTATION_CONTEXT ( 'NONE', 'WORKASPACE' ) );
#8327 = CARTESIAN_POINT ( 'NONE',  ( 152.2287565553230309, -1.999999999999974465, -29.49038105676660493 ) ) ;
#8328 = DIRECTION ( 'NONE',  ( -1.110223024625156540E-16, 0.000000000000000000, -1.000000000000000000 ) ) ;
#8329 = LINE ( 'NONE', #22533, #6561 ) ;
#8330 = DIRECTION ( 'NONE',  ( 0.000000000000000000, 0.000000000000000000, 1.000000000000000000 ) ) ;
#8331 = CARTESIAN_POINT ( 'NONE',  ( 25.86774690167791135, -3.337865513817628749, -16.68124922160397006 ) ) ;
#8332 = CARTESIAN_POINT ( 'NONE',  ( 15.10175627602374249, 9.741420229655037843, -13.89989488922661742 ) ) ;
#8333 = CARTESIAN_POINT ( 'NONE',  ( 33.94449656094377588, -11.59990251341361933, -20.77871222707083376 ) ) ;
#8334 = CARTESIAN_POINT ( 'NONE',  ( 144.5152310637605808, -10.00000000000000178, -21.71180489736091346 ) ) ;
#8335 = CARTESIAN_POINT ( 'NONE',  ( 9.921764701973689426, 16.38287729030320250, -16.50235149140834778 ) ) ;
#8336 = CARTESIAN_POINT ( 'NONE',  ( 0.000000000000000000, 0.000000000000000000, -4.449444346342715129 ) ) ;
#8337 = LINE ( 'NONE', #20229, #25619 ) ;
#8338 = CARTESIAN_POINT ( 'NONE',  ( 13.12553198385420927, 8.571700941790735939, -15.91037888968202552 ) ) ;
#8339 = DIRECTION ( 'NONE',  ( -0.5877852522924731371, 0.000000000000000000, 0.8090169943749474513 ) ) ;
#8340 = CARTESIAN_POINT ( 'NONE',  ( 0.000000000000000000, 0.000000000000000000, -2.450000000000000178 ) ) ;
#8341 = CARTESIAN_POINT ( 'NONE',  ( 11.47304865262203499, 9.268493388164605662, -15.86084085272616484 ) ) ;
#8342 = VERTEX_POINT ( 'NONE', #13609 ) ;
#8343 = VECTOR ( 'NONE', #1307, 1000.000000000000000 ) ;
#8344 = FACE_OUTER_BOUND ( 'NONE', #12117, .T. ) ;
#8345 = CARTESIAN_POINT ( 'NONE',  ( 139.5152310637605808, -4.999999999999980460, -1.548930218128858680E-14 ) ) ;
#8346 = DIRECTION ( 'NONE',  ( 0.000000000000000000, 0.000000000000000000, 1.000000000000000000 ) ) ;
#8347 = EDGE_LOOP ( 'NONE', ( #5767, #24125, #26984, #59, #20659 ) ) ;
#8348 = CARTESIAN_POINT ( 'NONE',  ( 17.72817910449685996, 9.547663288818908356, -12.24198789229035533 ) ) ;
#8349 = CARTESIAN_POINT ( 'NONE',  ( 31.68531546575670532, -10.25520638109567173, -17.65856934995331784 ) ) ;
#8350 = VERTEX_POINT ( 'NONE', #18795 ) ;
#8351 = CARTESIAN_POINT ( 'NONE',  ( 30.15790919126650138, -6.784097790808209183, -15.35074926656157324 ) ) ;
#8352 = CARTESIAN_POINT ( 'NONE',  ( 23.54468722040186890, -6.934586491718037315, -13.40271233150634878 ) ) ;
#8353 = CARTESIAN_POINT ( 'NONE',  ( 177.2287565553229172, -1.999999999999968026, -29.49038105676660493 ) ) ;
#8354 = CARTESIAN_POINT ( 'NONE',  ( 8.000000000000000000, -4.618802153517027165, -0.7145311798163362926 ) ) ;
#8355 = CARTESIAN_POINT ( 'NONE',  ( 120.2036091896494980, -4.999999999999985789, -87.33303409601636247 ) ) ;
#8356 = ORIENTED_EDGE ( 'NONE', *, *, #19860, .F. ) ;
#8357 = EDGE_CURVE ( 'NONE', #22145, #6733, #16350, .T. ) ;
#8358 = ORIENTED_EDGE ( 'NONE', *, *, #4154, .T. ) ;
#8359 = CARTESIAN_POINT ( 'NONE',  ( 154.7287565553230309, -1.999999999999973577, -33.82050807568879947 ) ) ;
#8360 = EDGE_CURVE ( 'NONE', #20122, #27640, #21538, .T. ) ;
#8361 = AXIS2_PLACEMENT_3D ( 'NONE', #3435, #12727, #10285 ) ;
#8362 = CARTESIAN_POINT ( 'NONE',  ( 153.6922820468853672, -10.00000000000000178, -9.266330736598359152 ) ) ;
#8363 = CARTESIAN_POINT ( 'NONE',  ( 159.7287565553229456, -10.00000000000000000, -16.50000000000000355 ) ) ;
#8364 = CARTESIAN_POINT ( 'NONE',  ( 12.11773132146483789, 9.045882004348337446, -16.64348121447567053 ) ) ;
#8365 = CARTESIAN_POINT ( 'NONE',  ( 35.54859569580823830, -22.18452385850428499, -18.27063337037174762 ) ) ;
#8366 = ORIENTED_EDGE ( 'NONE', *, *, #7725, .T. ) ;
#8367 = CARTESIAN_POINT ( 'NONE',  ( 8.945901566930443138, 16.94555336501101550, -17.80918358208353069 ) ) ;
#8368 = ORIENTED_EDGE ( 'NONE', *, *, #28876, .T. ) ;
#8369 = CARTESIAN_POINT ( 'NONE',  ( 26.18758235895636233, -4.355437658720127558, -18.53605802859044260 ) ) ;
#8370 = CARTESIAN_POINT ( 'NONE',  ( 12.86833691348896203, 9.516071730297785081, -16.11536789055087837 ) ) ;
#8371 = FACE_BOUND ( 'NONE', #17114, .T. ) ;
#8372 = ORIENTED_EDGE ( 'NONE', *, *, #23136, .T. ) ;
#8373 = LINE ( 'NONE', #6094, #27624 ) ;
#8374 = CARTESIAN_POINT ( 'NONE',  ( 11.58682163191119230, 8.958038730125363003, -15.79767441425272345 ) ) ;
#8376 = DIRECTION ( 'NONE',  ( -1.000000000000000000, 0.000000000000000000, 1.734723475976807587E-16 ) ) ;
#8375 = VECTOR ( 'NONE', #20623, 1000.000000000000000 ) ;
#8377 = EDGE_LOOP ( 'NONE', ( #6621, #9394, #12062, #28286 ) ) ;
#8378 = DIRECTION ( 'NONE',  ( -2.698458740408365879E-16, 1.000000000000000000, 0.000000000000000000 ) ) ;
#8379 = ORIENTED_EDGE ( 'NONE', *, *, #29365, .F. ) ;
#8380 = CARTESIAN_POINT ( 'NONE',  ( 13.12216094266758581, 8.570213704404382682, -15.91306547940487448 ) ) ;
#8381 = ADVANCED_FACE ( 'NONE', ( #28153 ), #27998, .T. ) ;
#8382 = EDGE_LOOP ( 'NONE', ( #27558, #23623, #20555, #18508 ) ) ;
#8383 = CARTESIAN_POINT ( 'NONE',  ( 16.51977620067554042, 7.986930271725532826, -13.83285890266734519 ) ) ;
#8384 = CARTESIAN_POINT ( 'NONE',  ( 17.64024190839899120, 8.465516882244152441, -14.08803959672746586 ) ) ;
#8385 = PRODUCT_RELATED_PRODUCT_CATEGORY ( 'part', '', ( #1575 ) ) ;
#8386 = DIRECTION ( 'NONE',  ( -1.110223024625156540E-16, 0.000000000000000000, -1.000000000000000000 ) ) ;
#8387 = VERTEX_POINT ( 'NONE', #18651 ) ;
#8388 = CARTESIAN_POINT ( 'NONE',  ( 129.5152310637605524, -10.00000000000000888, -30.37205893520530964 ) ) ;
#8389 = CARTESIAN_POINT ( 'NONE',  ( 20.22088415693689356, -1.238650738454883493, -19.72259765018230482 ) ) ;
#8390 = VECTOR ( 'NONE', #14386, 1000.000000000000000 ) ;
#8391 = FACE_OUTER_BOUND ( 'NONE', #24400, .T. ) ;
#8392 = DIRECTION ( 'NONE',  ( -2.908569913943825554E-16, 1.000000000000000000, -6.826925868028084042E-18 ) ) ;
#8393 = VECTOR ( 'NONE', #30227, 1000.000000000000000 ) ;
#8394 = EDGE_LOOP ( 'NONE', ( #13823, #24088, #27029, #9633 ) ) ;
#8395 = DIRECTION ( 'NONE',  ( 1.000000000000000000, 2.908569913943825554E-16, -6.938893903907227392E-16 ) ) ;
#8396 = CARTESIAN_POINT ( 'NONE',  ( 34.39741479528305490, -17.01287786994462792, -20.00997473120332515 ) ) ;
#8397 = CARTESIAN_POINT ( 'NONE',  ( 13.15390973649967599, 8.859676595473322536, -14.60899741038990562 ) ) ;
#8398 = ORIENTED_EDGE ( 'NONE', *, *, #26935, .T. ) ;
#8399 = PLANE ( 'NONE',  #15360 ) ;
#8400 = CARTESIAN_POINT ( 'NONE',  ( 12.26214823032917778, 9.523620991859985452, -15.31974707146758341 ) ) ;
#8401 = CARTESIAN_POINT ( 'NONE',  ( 34.96958981470057637, -20.58335714263341387, -21.20026138435576613 ) ) ;
#8402 = DIRECTION ( 'NONE',  ( 0.5877852522924731371, 1.586114251531760728E-16, -0.8090169943749474513 ) ) ;
#8403 = ORIENTED_EDGE ( 'NONE', *, *, #14272, .T. ) ;
#8404 = CARTESIAN_POINT ( 'NONE',  ( -7.372574772901430151E-15, -9.237604307034054330, -5.000000000000000888 ) ) ;
#8405 = EDGE_LOOP ( 'NONE', ( #23698, #5404, #24121, #21265 ) ) ;
#8406 = VECTOR ( 'NONE', #4428, 1000.000000000000000 ) ;
#8407 = CARTESIAN_POINT ( 'NONE',  ( 10.83941243988239833, 8.530520621650927282, -16.32009337531726345 ) ) ;
#8408 = CARTESIAN_POINT ( 'NONE',  ( 131.1922820468854241, -10.00000000000000888, -30.91696583120935671 ) ) ;
#8409 = CARTESIAN_POINT ( 'NONE',  ( 138.6922820468854525, -4.999999999999980460, -35.24709285013155835 ) ) ;
#8410 = CARTESIAN_POINT ( 'NONE',  ( 163.6922820468853672, -9.999999999999998224, -23.73366926340167637 ) ) ;
#8411 = ORIENTED_EDGE ( 'NONE', *, *, #1207, .F. ) ;
#8412 = CARTESIAN_POINT ( 'NONE',  ( 12.87010724449035415, 9.516853939945930208, -16.11395691550788101 ) ) ;
#8413 = EDGE_CURVE ( 'NONE', #12010, #10075, #9781, .T. ) ;
#8414 = ADVANCED_FACE ( 'NONE', ( #16502 ), #23685, .T. ) ;
#8415 = CARTESIAN_POINT ( 'NONE',  ( 36.31991209326969283, -20.15716956937155047, -19.46864736847591359 ) ) ;
#8416 = CARTESIAN_POINT ( 'NONE',  ( 19.40121574091639189, 1.432572567346982240, -13.43353846741550406 ) ) ;
#8417 = ORIENTED_EDGE ( 'NONE', *, *, #27618, .T. ) ;
#8418 = ADVANCED_FACE ( 'NONE', ( #16657, #24001, #3097, #9631, #12224, #12366, #16956, #21230, #7652, #26285, #2943, #18950, #11768, #14347, #14049, #21389, #5367, #14207, #2636, #343, #21086, #21679, #4758, #7056, #640, #9473, #28302, #9325, #23376, #7359, #5058, #12069, #495, #19095, #16802, #28450, #2499, #192, #7503, #26134, #23843, #9925, #19240, #5519, #14799, #7946, #6112, #1102, #8239, #15407, #29368, #15102, #21837, #17396, #10529, #22288, #21990, #12822, #10379, #3382, #24436, #5668, #1395, #10076, #24137, #19997, #3239, #19689, #15255, #12517, #19836, #943, #29051, #3674, #13123, #8088, #10228, #26744 ), #5966, .T. ) ;
#8419 = ORIENTED_EDGE ( 'NONE', *, *, #18340, .F. ) ;
#8420 = DIRECTION ( 'NONE',  ( 0.5877852522924731371, 1.586114251531760728E-16, 0.8090169943749474513 ) ) ;
#8421 = VECTOR ( 'NONE', #18870, 1000.000000000000000 ) ;
#8422 = EDGE_CURVE ( 'NONE', #30027, #11898, #26584, .T. ) ;
#8423 = CARTESIAN_POINT ( 'NONE',  ( 157.2287565553229740, -4.999999999999975131, -20.83012701892221585 ) ) ;
#8424 = FACE_OUTER_BOUND ( 'NONE', #21010, .T. ) ;
#8425 = FILL_AREA_STYLE ('',( #20473 ) ) ;
#8426 = CARTESIAN_POINT ( 'NONE',  ( 28.92999000670439713, -5.550862855971650411, -17.57004703619191943 ) ) ;
#8427 = CARTESIAN_POINT ( 'NONE',  ( 18.72855672543857608, 2.184447897796080174, -13.82944682127929426 ) ) ;
#8428 = ORIENTED_EDGE ( 'NONE', *, *, #12170, .F. ) ;
#8429 = VERTEX_POINT ( 'NONE', #14948 ) ;
#8430 = EDGE_LOOP ( 'NONE', ( #12068, #10052 ) ) ;
#8431 = CARTESIAN_POINT ( 'NONE',  ( 152.0152310637605240, -10.00000000000000178, -6.958068083716895558 ) ) ;
#8432 = CARTESIAN_POINT ( 'NONE',  ( 98.38891821480183353, -4.999999999999990230, 71.48373336749482121 ) ) ;
#8433 = DIRECTION ( 'NONE',  ( 0.000000000000000000, 0.000000000000000000, -1.000000000000000000 ) ) ;
#8434 = CARTESIAN_POINT ( 'NONE',  ( 2.500000000000000444, 2.500728763858895382E-16, -2.041999999999999815 ) ) ;
#8435 = DIRECTION ( 'NONE',  ( -0.8090169943749474513, -2.183098979609982436E-16, -0.5877852522924731371 ) ) ;
#8436 = CARTESIAN_POINT ( 'NONE',  ( 142.0152310637605808, -1.999999999999978462, -6.958068083716895558 ) ) ;
#8437 = CONICAL_SURFACE ( 'NONE', #2151, 4.000000000000003553, 1.047197551196597853 ) ;
#8438 = CARTESIAN_POINT ( 'NONE',  ( 11.22446318822032296, 9.088639264749929225, -17.24136893309019669 ) ) ;
#8439 = CARTESIAN_POINT ( 'NONE',  ( 10.33811693838771717, 18.38618951776012267, -17.91752729848688830 ) ) ;
#8440 = CARTESIAN_POINT ( 'NONE',  ( 30.50670359208957905, -8.903545733563623443, -17.67935522427464079 ) ) ;
#8441 = ORIENTED_EDGE ( 'NONE', *, *, #12974, .T. ) ;
#8442 = DIRECTION ( 'NONE',  ( -0.5877852522924731371, -1.586114251531760235E-16, 0.8090169943749474513 ) ) ;
#8443 = CARTESIAN_POINT ( 'NONE',  ( 163.6922820468853672, -9.999999999999998224, -26.58683881228715862 ) ) ;
#8444 = ORIENTED_EDGE ( 'NONE', *, *, #15367, .F. ) ;
#8445 = CYLINDRICAL_SURFACE ( 'NONE', #9821, 13.00000000000000178 ) ;
#8446 = PLANE ( 'NONE',  #8296 ) ;
#8447 = CARTESIAN_POINT ( 'NONE',  ( 159.7287565553228887, -10.00000000000000000, 0.8205080756887930260 ) ) ;
#8448 = CARTESIAN_POINT ( 'NONE',  ( 26.04489551603160180, -6.130266781319400948, -13.71289979607875154 ) ) ;
#8449 = DIRECTION ( 'NONE',  ( -2.698458740408365879E-16, 1.000000000000000000, 0.000000000000000000 ) ) ;
#8450 = CARTESIAN_POINT ( 'NONE',  ( 12.27129069473257239, 9.507470051170034964, -15.31400031939534045 ) ) ;
#8451 = AXIS2_PLACEMENT_3D ( 'NONE', #20417, #18583, #2426 ) ;
#8452 = EDGE_CURVE ( 'NONE', #14013, #21320, #10687, .T. ) ;
#8453 = CARTESIAN_POINT ( 'NONE',  ( 32.77977724007769211, -11.13765286058784554, -18.71157503069099448 ) ) ;
#8454 = CARTESIAN_POINT ( 'NONE',  ( -4.000000000000003553, -0.7779732554280804901, -0.03354435108168069002 ) ) ;
#8455 = ADVANCED_FACE ( 'NONE', ( #24743 ), #17696, .T. ) ;
#8456 = EDGE_CURVE ( 'NONE', #27422, #2121, #785, .T. ) ;
#8457 = CARTESIAN_POINT ( 'NONE',  ( 26.58455406938135468, -5.910422570377376950, -13.89432871846328688 ) ) ;
#8458 = DIRECTION ( 'NONE',  ( -2.698458740408365879E-16, 1.000000000000000000, 0.000000000000000000 ) ) ;
#8459 = EDGE_CURVE ( 'NONE', #10839, #28670, #21579, .T. ) ;
#8460 = CARTESIAN_POINT ( 'NONE',  ( 18.26618351132839280, 3.382507019981081164, -13.19753224271465797 ) ) ;
#8461 = ORIENTED_EDGE ( 'NONE', *, *, #11576, .F. ) ;
#8462 = LINE ( 'NONE', #15319, #14904 ) ;
#8463 = ORIENTED_EDGE ( 'NONE', *, *, #23522, .F. ) ;
#8464 = ORIENTED_EDGE ( 'NONE', *, *, #13351, .F. ) ;
#8465 =( LENGTH_UNIT ( ) NAMED_UNIT ( * ) SI_UNIT ( .MILLI., .METRE. ) );
#8466 = CARTESIAN_POINT ( 'NONE',  ( 28.90796184913828171, -12.27476343136570414, -11.88515153054143347 ) ) ;
#8467 = CARTESIAN_POINT ( 'NONE',  ( 23.45579420008465732, -3.438291973250592992, -12.29892528769388349 ) ) ;
#8468 = VECTOR ( 'NONE', #6534, 1000.000000000000000 ) ;
#8469 = ORIENTED_EDGE ( 'NONE', *, *, #11209, .T. ) ;
#8470 = CARTESIAN_POINT ( 'NONE',  ( -1.313474075707253608, -8.479269695850879529, -0.3167204509598532947 ) ) ;
#8471 = LINE ( 'NONE', #17327, #4080 ) ;
#8472 = ORIENTED_EDGE ( 'NONE', *, *, #14473, .F. ) ;
#8473 = DIRECTION ( 'NONE',  ( -0.8660254037844375974, 0.5000000000000017764, -0.000000000000000000 ) ) ;
#8474 = CARTESIAN_POINT ( 'NONE',  ( 148.6922820468854525, -1.999999999999975797, -32.39392330124607611 ) ) ;
#8475 = LINE ( 'NONE', #17775, #26544 ) ;
#8476 = CARTESIAN_POINT ( 'NONE',  ( 132.0152310637605524, -10.00000000000000711, -26.04193191628310800 ) ) ;
#8477 = CARTESIAN_POINT ( 'NONE',  ( 25.47886751038978304, -3.221426504603704277, -15.37741025701318698 ) ) ;
#8478 = CARTESIAN_POINT ( 'NONE',  ( 49.00000000000000000, 6.779440132085338567E-16, -4.513000000000000789 ) ) ;
#8479 = CARTESIAN_POINT ( 'NONE',  ( 35.65609946332594404, -19.17501105436304343, -21.36250568352834378 ) ) ;
#8480 = CARTESIAN_POINT ( 'NONE',  ( 0.6554360035617698976, -4.240386000424092749, -0.1586754815285197906 ) ) ;
#8481 = CARTESIAN_POINT ( 'NONE',  ( 12.49271550807400999, 8.567542729147559655, -15.13597632865050535 ) ) ;
#8482 = AXIS2_PLACEMENT_3D ( 'NONE', #4505, #14092, #30201 ) ;
#8483 = LINE ( 'NONE', #20377, #3472 ) ;
#8484 = PLANE ( 'NONE',  #22714 ) ;
#8485 = CARTESIAN_POINT ( 'NONE',  ( 9.661894807476521407, 16.25477276558749296, -17.91386948909976695 ) ) ;
#8486 = CARTESIAN_POINT ( 'NONE',  ( 3.660532965668829686, -7.124194613927646635, -4.999999999999990230 ) ) ;
#8487 = DIRECTION ( 'NONE',  ( -0.9510565162951536422, -2.566386769018988816E-16, -0.3090169943749472292 ) ) ;
#8488 = CARTESIAN_POINT ( 'NONE',  ( 10.56508425215480074, 13.43253182900300402, -16.23631622730588830 ) ) ;
#8489 = ORIENTED_EDGE ( 'NONE', *, *, #5119, .T. ) ;
#8490 = CARTESIAN_POINT ( 'NONE',  ( 5.000000000000004441, 0.000000000000000000, 0.000000000000000000 ) ) ;
#8491 = DIRECTION ( 'NONE',  ( 0.000000000000000000, 0.000000000000000000, 1.000000000000000000 ) ) ;
#8492 = EDGE_CURVE ( 'NONE', #12774, #10367, #28759, .T. ) ;
#8493 = EDGE_CURVE ( 'NONE', #4135, #18869, #15652, .T. ) ;
#8494 = DIRECTION ( 'NONE',  ( -2.698458740408365879E-16, 1.000000000000000000, 0.000000000000000000 ) ) ;
#8495 = ADVANCED_FACE ( 'NONE', ( #17551 ), #6269, .T. ) ;
#8496 = ORIENTED_EDGE ( 'NONE', *, *, #19774, .F. ) ;
#8497 = EDGE_CURVE ( 'NONE', #12877, #9720, #19608, .T. ) ;
#8498 = CARTESIAN_POINT ( 'NONE',  ( 13.39626964006587428, 7.633314995549595139, -15.69459619883729928 ) ) ;
#8499 = CARTESIAN_POINT ( 'NONE',  ( 32.00851579392290347, -10.30430276118739918, -18.57203464379605151 ) ) ;
#8500 = CARTESIAN_POINT ( 'NONE',  ( 18.20609423209794642, 11.47008825724650549, -18.02705416172272734 ) ) ;
#8501 = CARTESIAN_POINT ( 'NONE',  ( 24.40455984355908114, -10.10244183743681035, -17.68366952546245585 ) ) ;
#8502 = LINE ( 'NONE', #13380, #29226 ) ;
#8503 = DIRECTION ( 'NONE',  ( -0.8090169943749474513, -2.183098979609982436E-16, -0.5877852522924731371 ) ) ;
#8504 = DIRECTION ( 'NONE',  ( 0.9510565162951535312, 2.566386769018988816E-16, -0.3090169943749475623 ) ) ;
#8505 = VECTOR ( 'NONE', #22178, 1000.000000000000000 ) ;
#8506 = VERTEX_POINT ( 'NONE', #20141 ) ;
#8507 = ORIENTED_EDGE ( 'NONE', *, *, #10268, .T. ) ;
#8508 = FACE_OUTER_BOUND ( 'NONE', #16650, .T. ) ;
#8509 = ORIENTED_EDGE ( 'NONE', *, *, #1042, .T. ) ;
#8510 = CARTESIAN_POINT ( 'NONE',  ( -20.00000000000017053, 34.64101615137744972, 4.999999999999998224 ) ) ;
#8511 = ORIENTED_EDGE ( 'NONE', *, *, #26826, .F. ) ;
#8512 = DIRECTION ( 'NONE',  ( 2.908569913943825554E-16, -1.000000000000000000, 0.000000000000000000 ) ) ;
#8513 = CARTESIAN_POINT ( 'NONE',  ( 13.34161425493533315, 8.667191563245470576, -15.73815750552000381 ) ) ;
#8514 = ORIENTED_EDGE ( 'NONE', *, *, #18561, .F. ) ;
#8515 = CARTESIAN_POINT ( 'NONE',  ( 35.54824714876834690, -21.18295802128256611, -18.40066978570660083 ) ) ;
#8516 = ORIENTED_EDGE ( 'NONE', *, *, #25043, .F. ) ;
#8517 = CARTESIAN_POINT ( 'NONE',  ( 9.112400085652602399, 16.18196993452624355, -17.05477891849903926 ) ) ;
#8518 = EDGE_LOOP ( 'NONE', ( #10959, #4477, #137, #18115, #14886 ) ) ;
#8519 = CARTESIAN_POINT ( 'NONE',  ( 28.12266609392075267, -5.599633216697744942, -16.00068813756295327 ) ) ;
#8520 = CARTESIAN_POINT ( 'NONE',  ( 10.35864918915110877, 16.97212501191939538, -17.95086732675817132 ) ) ;
#8521 = DIRECTION ( 'NONE',  ( 1.000000000000000000, 2.698458740408365879E-16, -1.110223024625156540E-16 ) ) ;
#8522 = ORIENTED_EDGE ( 'NONE', *, *, #12371, .F. ) ;
#8523 = LINE ( 'NONE', #15545, #22207 ) ;
#8524 = EDGE_CURVE ( 'NONE', #9448, #23002, #18298, .T. ) ;
#8525 = AXIS2_PLACEMENT_3D ( 'NONE', #10421, #27259, #5715 ) ;
#8526 = FACE_OUTER_BOUND ( 'NONE', #9267, .T. ) ;
#8527 = DIRECTION ( 'NONE',  ( -0.5877852522924731371, 0.000000000000000000, 0.8090169943749474513 ) ) ;
#8528 = CARTESIAN_POINT ( 'NONE',  ( 142.0152310637606092, -1.999999999999978018, -32.93883019725009120 ) ) ;
#8529 = ORIENTED_EDGE ( 'NONE', *, *, #18596, .T. ) ;
#8530 = EDGE_CURVE ( 'NONE', #22161, #19955, #27810, .T. ) ;
#8531 = CARTESIAN_POINT ( 'NONE',  ( 9.661883355341293722, 16.25482528653935077, -17.91547504436015004 ) ) ;
#8532 = CARTESIAN_POINT ( 'NONE',  ( 18.76724195421386554, 7.045283186750163296, -20.62625128596355495 ) ) ;
#8533 = CARTESIAN_POINT ( 'NONE',  ( 15.09088459799990822, 3.595497735170159803, -19.35696164441904443 ) ) ;
#8534 = DIRECTION ( 'NONE',  ( 0.9510565162951536422, 2.566386769018988816E-16, 0.3090169943749472292 ) ) ;
#8535 = ORIENTED_EDGE ( 'NONE', *, *, #29953, .T. ) ;
#8536 = CARTESIAN_POINT ( 'NONE',  ( 154.5152310637604671, -1.999999999999975353, -4.391296821672111328 ) ) ;
#8537 = CARTESIAN_POINT ( 'NONE',  ( 16.89369580670022941, 0.5033910033923695293, -17.32063897790030893 ) ) ;
#8538 = FACE_OUTER_BOUND ( 'NONE', #8058, .T. ) ;
#8539 = CARTESIAN_POINT ( 'NONE',  ( 132.0152310637605808, -10.00000000000000711, -32.93883019725009120 ) ) ;
#8540 = VECTOR ( 'NONE', #8547, 1000.000000000000000 ) ;
#8541 = ORIENTED_EDGE ( 'NONE', *, *, #29687, .T. ) ;
#8542 = EDGE_CURVE ( 'NONE', #16524, #12515, #20589, .T. ) ;
#8543 = DIRECTION ( 'NONE',  ( -6.938893903907227392E-16, 0.000000000000000000, -1.000000000000000000 ) ) ;
#8544 = CARTESIAN_POINT ( 'NONE',  ( 35.09336438560361415, -20.13941072448723801, -20.22035334018532637 ) ) ;
#8545 = DIRECTION ( 'NONE',  ( 0.9510565162951536422, 2.566386769018988816E-16, 0.3090169943749472292 ) ) ;
#8546 = ORIENTED_EDGE ( 'NONE', *, *, #20208, .T. ) ;
#8547 = DIRECTION ( 'NONE',  ( -0.5877852522924731371, -1.586114251531760235E-16, 0.8090169943749474513 ) ) ;
#8548 = CARTESIAN_POINT ( 'NONE',  ( 11.05541531668977662, 17.68942339022145305, -17.92015940598198753 ) ) ;
#8549 = CARTESIAN_POINT ( 'NONE',  ( 35.54859390953723164, -23.18451583373416014, -14.99999999999999822 ) ) ;
#8550 = CIRCLE ( 'NONE', #8076, 4.000000000000000000 ) ;
#8551 = ORIENTED_EDGE ( 'NONE', *, *, #27038, .F. ) ;
#8552 = CARTESIAN_POINT ( 'NONE',  ( 12.71834232392635045, 8.667191563245470576, -14.95615232649864090 ) ) ;
#8553 = AXIS2_PLACEMENT_3D ( 'NONE', #13262, #22580, #4258 ) ;
#8554 = CARTESIAN_POINT ( 'NONE',  ( 10.66915452275446619, 9.042499785519874322, -16.41100549784887619 ) ) ;
#8555 = PLANE ( 'NONE',  #53 ) ;
#8556 = CARTESIAN_POINT ( 'NONE',  ( 143.6922820468854525, -1.999999999999978018, -17.92658477444275889 ) ) ;
#8557 = VERTEX_POINT ( 'NONE', #11137 ) ;
#8558 = CARTESIAN_POINT ( 'NONE',  ( 147.0152310637605524, -4.999999999999977796, -6.958068083716895558 ) ) ;
#8559 = VERTEX_POINT ( 'NONE', #6720 ) ;
#8560 = CARTESIAN_POINT ( 'NONE',  ( 12.86729516143382845, 9.515644835462770956, -16.11619563230584973 ) ) ;
#8561 = ORIENTED_EDGE ( 'NONE', *, *, #25875, .T. ) ;
#8563 = CARTESIAN_POINT ( 'NONE',  ( 36.54859390953724585, -21.18451583373416014, -17.22552805718784441 ) ) ;
#8562 = VECTOR ( 'NONE', #21446, 1000.000000000000000 ) ;
#8564 = CARTESIAN_POINT ( 'NONE',  ( 17.55424633453837302, 0.6138019359854992585, -14.89346452969079060 ) ) ;
#8565 = EDGE_LOOP ( 'NONE', ( #9605, #29472, #19777, #4770 ) ) ;
#8566 = CARTESIAN_POINT ( 'NONE',  ( 148.6922820468854525, -4.999999999999977796, -26.58683881228715862 ) ) ;
#8567 = ORIENTED_EDGE ( 'NONE', *, *, #1969, .T. ) ;
#8568 = CARTESIAN_POINT ( 'NONE',  ( 149.7287565553229740, -1.999999999999976241, -7.839745962155603820 ) ) ;
#8569 =( NAMED_UNIT ( * ) PLANE_ANGLE_UNIT ( ) SI_UNIT ( $, .RADIAN. ) );
#8570 = CARTESIAN_POINT ( 'NONE',  ( 27.71186802668094273, -7.007055141436442369, -19.33373627201896383 ) ) ;
#8571 = CARTESIAN_POINT ( 'NONE',  ( 20.32939975687981615, -5.674178230592766603, -17.16996371750385109 ) ) ;
#8572 = ORIENTED_EDGE ( 'NONE', *, *, #1168, .T. ) ;
#8573 = ORIENTED_EDGE ( 'NONE', *, *, #7202, .T. ) ;
#8574 = CARTESIAN_POINT ( 'NONE',  ( 162.0152310637604103, -9.999999999999998224, -0.06116980274991495881 ) ) ;
#8575 = DIRECTION ( 'NONE',  ( 0.000000000000000000, 0.000000000000000000, 1.000000000000000000 ) ) ;
#8576 = AXIS2_PLACEMENT_3D ( 'NONE', #27121, #1619, #17617 ) ;
#8577 = DIRECTION ( 'NONE',  ( -0.8090169943749474513, -2.183098979609982436E-16, -0.5877852522924731371 ) ) ;
#8578 = EDGE_CURVE ( 'NONE', #3931, #30101, #22748, .T. ) ;
#8579 = CARTESIAN_POINT ( 'NONE',  ( 13.00000000000000178, -2.870178842070716726E-15, -23.00000000000000000 ) ) ;
#8580 = DIRECTION ( 'NONE',  ( 0.3090169943749472292, 8.338696094057992503E-17, -0.9510565162951536422 ) ) ;
#8581 = VECTOR ( 'NONE', #23251, 1000.000000000000000 ) ;
#8582 = EDGE_CURVE ( 'NONE', #24297, #18704, #20287, .T. ) ;
#8583 = CARTESIAN_POINT ( 'NONE',  ( 15.00000000000000000, 0.000000000000000000, 0.000000000000000000 ) ) ;
#8584 = VECTOR ( 'NONE', #6015, 1000.000000000000000 ) ;
#8585 = CARTESIAN_POINT ( 'NONE',  ( 11.22390034614927856, 9.091215689738174177, -17.24160205726399653 ) ) ;
#8586 = CARTESIAN_POINT ( 'NONE',  ( 12.56861602585598980, 8.601024833420110483, -15.07548682890769243 ) ) ;
#8587 = CARTESIAN_POINT ( 'NONE',  ( 157.0152310637604387, -10.00000000000000000, -0.06116980274991495881 ) ) ;
#8588 = DIRECTION ( 'NONE',  ( 0.000000000000000000, 0.000000000000000000, -1.000000000000000000 ) ) ;
#8589 = LINE ( 'NONE', #8443, #8105 ) ;
#8590 = ORIENTED_EDGE ( 'NONE', *, *, #10381, .T. ) ;
#8591 = CARTESIAN_POINT ( 'NONE',  ( 9.641354186875979337, 17.66887565656821124, -17.90893343548146177 ) ) ;
#8592 = DIRECTION ( 'NONE',  ( 1.000000000000000000, 2.698458740408365879E-16, -1.110223024625156540E-16 ) ) ;
#8593 = DIRECTION ( 'NONE',  ( 1.000000000000000000, 0.000000000000000000, 0.000000000000000000 ) ) ;
#8594 = DIRECTION ( 'NONE',  ( 0.5877852522924731371, 1.586114251531760728E-16, -0.8090169943749474513 ) ) ;
#8596 = ORIENTED_EDGE ( 'NONE', *, *, #8497, .T. ) ;
#8595 = CARTESIAN_POINT ( 'NONE',  ( 22.90372073960079646, -4.505259139820817715, -13.75793632099288111 ) ) ;
#8597 = ORIENTED_EDGE ( 'NONE', *, *, #27871, .T. ) ;
#8598 = CARTESIAN_POINT ( 'NONE',  ( 5.749818843786239420, -5.000000000000015987, 17.69612279726095139 ) ) ;
#8599 = CARTESIAN_POINT ( 'NONE',  ( 12.24726067228269422, 9.517041913610183812, -15.33161271801373182 ) ) ;
#8600 = DIRECTION ( 'NONE',  ( 0.000000000000000000, 0.000000000000000000, -1.000000000000000000 ) ) ;
#8601 = FACE_BOUND ( 'NONE', #26626, .T. ) ;
#8602 = VECTOR ( 'NONE', #28339, 1000.000000000000000 ) ;
#8603 = CARTESIAN_POINT ( 'NONE',  ( 23.60870351872479844, -7.222488552757559077, -14.83554404960226947 ) ) ;
#8604 = DIRECTION ( 'NONE',  ( 1.000000000000000000, 2.698458740408365879E-16, -1.110223024625156540E-16 ) ) ;
#8605 = CARTESIAN_POINT ( 'NONE',  ( 23.81787570424677014, -0.6874775570582684070, -15.56398403670522157 ) ) ;
#8606 = ORIENTED_EDGE ( 'NONE', *, *, #26706, .T. ) ;
#8607 = CARTESIAN_POINT ( 'NONE',  ( 35.54859390953723874, -22.18451583373416014, -15.00000000000000000 ) ) ;
#8608 = SHAPE_REPRESENTATION_RELATIONSHIP ( 'NONE' , 'NONE' ,  #16744, #13457 ) ;
#8609 = CARTESIAN_POINT ( 'NONE',  ( 13.78676817088038931, 5.425489125369224119, -17.89072192914586168 ) ) ;
#8610 = VECTOR ( 'NONE', #2171, 1000.000000000000000 ) ;
#8611 = CARTESIAN_POINT ( 'NONE',  ( 27.20859382114707614, -12.49599901988731077, -15.99530080614381511 ) ) ;
#8612 = VECTOR ( 'NONE', #23095, 1000.000000000000114 ) ;
#8613 = ORIENTED_EDGE ( 'NONE', *, *, #17786, .T. ) ;
#8614 = CARTESIAN_POINT ( 'NONE',  ( 29.46565128511723586, -7.689737916804423534, -14.82739468409561567 ) ) ;
#8615 = AXIS2_PLACEMENT_3D ( 'NONE', #19727, #29096, #17150 ) ;
#8616 = DIRECTION ( 'NONE',  ( -2.698458740408365879E-16, 1.000000000000000000, 0.000000000000000000 ) ) ;
#8617 = EDGE_CURVE ( 'NONE', #21141, #5593, #16010, .T. ) ;
#8618 = LINE ( 'NONE', #27583, #28799 ) ;
#8619 = CARTESIAN_POINT ( 'NONE',  ( 102.5724172122712474, -4.999999999999989342, -74.52322330502413195 ) ) ;
#8620 = ADVANCED_FACE ( 'NONE', ( #27214 ), #30121, .F. ) ;
#8621 = DIRECTION ( 'NONE',  ( 0.9510565162951535312, 2.566386769018988816E-16, -0.3090169943749475623 ) ) ;
#8622 =( GEOMETRIC_REPRESENTATION_CONTEXT ( 3 ) GLOBAL_UNCERTAINTY_ASSIGNED_CONTEXT ( ( #2795 ) ) GLOBAL_UNIT_ASSIGNED_CONTEXT ( ( #28013, #1118, #21698 ) ) REPRESENTATION_CONTEXT ( 'NONE', 'WORKASPACE' ) );
#8623 = EDGE_CURVE ( 'NONE', #14471, #12367, #16163, .T. ) ;
#8624 = CARTESIAN_POINT ( 'NONE',  ( 4.681481898397010788, -6.534749472788171865, -1.177036983504575751E-14 ) ) ;
#8625 = CARTESIAN_POINT ( 'NONE',  ( 23.69966960967911973, -9.104540460734687812, -16.16703237251472558 ) ) ;
#8626 = CARTESIAN_POINT ( 'NONE',  ( 21.26575470983302196, 3.903880982571942493, -18.68858533207590966 ) ) ;
#8627 = CARTESIAN_POINT ( 'NONE',  ( 35.85321554361588170, -20.06054918781481788, -21.42207597224664894 ) ) ;
#8628 = CARTESIAN_POINT ( 'NONE',  ( 1.660531772554317831, -3.660093687634888848, -1.932505669160685592E-14 ) ) ;
#8629 = VECTOR ( 'NONE', #17614, 1000.000000000000000 ) ;
#8630 = CARTESIAN_POINT ( 'NONE',  ( 11.47511325496290624, 9.259230714725578792, -15.85997136665693041 ) ) ;
#8631 = DIRECTION ( 'NONE',  ( -1.000000000000000000, 0.000000000000000000, -0.000000000000000000 ) ) ;
#8632 = DIRECTION ( 'NONE',  ( 0.000000000000000000, 0.000000000000000000, 1.000000000000000000 ) ) ;
#8633 = CARTESIAN_POINT ( 'NONE',  ( 13.12808413666193275, 8.572828783776230921, -15.90834477884588516 ) ) ;
#8634 = DIRECTION ( 'NONE',  ( 0.5877852522924731371, 1.586114251531760728E-16, -0.8090169943749474513 ) ) ;
#8635 = CARTESIAN_POINT ( 'NONE',  ( 147.0152310637605808, -10.00000000000000178, -34.70218595412750773 ) ) ;
#8636 = CARTESIAN_POINT ( 'NONE',  ( 12.39803340617553928, 8.535179507765855433, -15.21071672276548625 ) ) ;
#8637 = VERTEX_POINT ( 'NONE', #17841 ) ;
#8638 = CARTESIAN_POINT ( 'NONE',  ( 139.7287565553230024, -1.999999999999979128, 0.8205080756887930260 ) ) ;
#8639 = DIRECTION ( 'NONE',  ( 0.000000000000000000, 0.000000000000000000, -1.000000000000000000 ) ) ;
#8640 = LINE ( 'NONE', #10929, #9774 ) ;
#8641 = ORIENTED_EDGE ( 'NONE', *, *, #27, .T. ) ;
#8642 = CARTESIAN_POINT ( 'NONE',  ( 8.944584683310379702, 16.95159276115599667, -17.95086732675816776 ) ) ;
#8643 = CARTESIAN_POINT ( 'NONE',  ( 31.91112766891453845, -10.28950255622343946, -18.29678896503644481 ) ) ;
#8644 = CARTESIAN_POINT ( 'NONE',  ( 22.45977841265724351, 4.097634946112983734, -18.47195213137534964 ) ) ;
#8645 = CARTESIAN_POINT ( 'NONE',  ( 30.58006126958193249, -8.114715823802763239, -15.12008790671442426 ) ) ;
#8646 = AXIS2_PLACEMENT_3D ( 'NONE', #8675, #20272, #15392 ) ;
#8647 = DIRECTION ( 'NONE',  ( 0.9510565162951536422, 2.566386769018988816E-16, 0.3090169943749472292 ) ) ;
#8648 = DIRECTION ( 'NONE',  ( -2.698458740408365879E-16, 1.000000000000000000, 0.000000000000000000 ) ) ;
#8649 = CARTESIAN_POINT ( 'NONE',  ( 26.83635784119175938, -3.902057423304301942, -19.75319010936098962 ) ) ;
#8650 = VECTOR ( 'NONE', #5660, 1000.000000000000000 ) ;
#8651 = VERTEX_POINT ( 'NONE', #20731 ) ;
#8652 = LINE ( 'NONE', #17960, #7469 ) ;
#8654 = ORIENTED_EDGE ( 'NONE', *, *, #11376, .F. ) ;
#8653 = DIRECTION ( 'NONE',  ( -2.698458740408365879E-16, 1.000000000000000000, 0.000000000000000000 ) ) ;
#8655 = ADVANCED_FACE ( 'NONE', ( #24896 ), #10832, .T. ) ;
#8656 = LINE ( 'NONE', #2381, #28837 ) ;
#8657 = CARTESIAN_POINT ( 'NONE',  ( 142.2287565553230309, -10.00000000000000533, -12.16987298107780369 ) ) ;
#8658 = ADVANCED_FACE ( 'NONE', ( #22449 ), #8981, .T. ) ;
#8659 = ADVANCED_FACE ( 'NONE', ( #1696 ), #29835, .T. ) ;
#8660 = EDGE_CURVE ( 'NONE', #20055, #10866, #8687, .T. ) ;
#8661 = LINE ( 'NONE', #29802, #12664 ) ;
#8662 = CARTESIAN_POINT ( 'NONE',  ( 35.46586886002400263, -20.81287600694606610, -19.09165458252410374 ) ) ;
#8663 = VERTEX_POINT ( 'NONE', #6424 ) ;
#8664 = CARTESIAN_POINT ( 'NONE',  ( 12.75280283744833376, 7.624395256242640251, -14.92868632776139037 ) ) ;
#8665 = ORIENTED_EDGE ( 'NONE', *, *, #15201, .T. ) ;
#8666 = VECTOR ( 'NONE', #22830, 1000.000000000000000 ) ;
#8667 = CARTESIAN_POINT ( 'NONE',  ( 26.57062215293289498, -11.41726559881178638, -18.09730928560479057 ) ) ;
#8668 = CARTESIAN_POINT ( 'NONE',  ( 142.0152310637605808, -10.00000000000000355, -6.958068083716895558 ) ) ;
#8669 = CARTESIAN_POINT ( 'NONE',  ( 14.75361449413180637, 10.34920949090176201, -14.61276839131081218 ) ) ;
#8670 = PLANE ( 'NONE',  #8756 ) ;
#8671 = ORIENTED_EDGE ( 'NONE', *, *, #1719, .F. ) ;
#8672 = VECTOR ( 'NONE', #9422, 1000.000000000000000 ) ;
#8673 = CARTESIAN_POINT ( 'NONE',  ( 2.698458740408370316E-15, -10.00000000000001776, 0.000000000000000000 ) ) ;
#8674 = CARTESIAN_POINT ( 'NONE',  ( 15.61762486822808604, 9.948436389806387226, -12.64537296286936829 ) ) ;
#8675 = CARTESIAN_POINT ( 'NONE',  ( 0.000000000000000000, 0.000000000000000000, 0.000000000000000000 ) ) ;
#8676 = DIRECTION ( 'NONE',  ( 1.000000000000000000, 2.891205793294675861E-16, 0.000000000000000000 ) ) ;
#8677 = EDGE_LOOP ( 'NONE', ( #22271, #227, #796, #13634 ) ) ;
#8678 = CARTESIAN_POINT ( 'NONE',  ( 9.661884236495001943, 16.25482124545614937, -17.91517755594902894 ) ) ;
#8679 = AXIS2_PLACEMENT_3D ( 'NONE', #7655, #16961, #26287 ) ;
#8680 = CARTESIAN_POINT ( 'NONE',  ( 22.01749846045582970, -4.595750957016929483, -16.30794181244783303 ) ) ;
#8681 = CARTESIAN_POINT ( 'NONE',  ( 20.44279466453895822, 5.363259340322034774, -13.44374883282906552 ) ) ;
#8682 = LINE ( 'NONE', #17989, #8689 ) ;
#8683 = CARTESIAN_POINT ( 'NONE',  ( 132.2287565553230024, -4.999999999999982236, -3.509618943233400401 ) ) ;
#8684 = CARTESIAN_POINT ( 'NONE',  ( 20.50636976340433293, -0.9757509181830721356, -19.91080244439677571 ) ) ;
#8685 = VECTOR ( 'NONE', #26112, 1000.000000000000000 ) ;
#8686 = LINE ( 'NONE', #5965, #14914 ) ;
#8687 = LINE ( 'NONE', #27370, #26449 ) ;
#8688 = B_SPLINE_CURVE_WITH_KNOTS ( 'NONE', 3,
 ( #7511, #11467, #202, #23238, #14360, #51 ),
 .UNSPECIFIED., .F., .F.,
 ( 4, 2, 4 ),
 ( 2.380731629581706008E-07, 0.002336973833157567244, 0.004673709593152178265 ),
 .UNSPECIFIED. ) ;
#8689 = VECTOR ( 'NONE', #30113, 1000.000000000000000 ) ;
#8690 = EDGE_CURVE ( 'NONE', #20489, #7228, #15711, .T. ) ;
#8691 = EDGE_LOOP ( 'NONE', ( #6325, #27663, #8464, #20415 ) ) ;
#8692 = EDGE_CURVE ( 'NONE', #26883, #13495, #4129, .T. ) ;
#8693 = EDGE_CURVE ( 'NONE', #21590, #30106, #7015, .T. ) ;
#8694 = LINE ( 'NONE', #3833, #26842 ) ;
#8695 = CARTESIAN_POINT ( 'NONE',  ( 35.02155038278115740, -19.81678845073966500, -20.19863594638463411 ) ) ;
#8696 = DIRECTION ( 'NONE',  ( 0.000000000000000000, 0.000000000000000000, -1.000000000000000000 ) ) ;
#8697 = EDGE_LOOP ( 'NONE', ( #4899, #29824, #12951, #177, #1206 ) ) ;
#8698 = DIRECTION ( 'NONE',  ( -2.698458740408365879E-16, 1.000000000000000000, 0.000000000000000000 ) ) ;
#8699 = CARTESIAN_POINT ( 'NONE',  ( 16.79143122783437292, 7.330551994622505063, -14.54187356113185103 ) ) ;
#8700 = CARTESIAN_POINT ( 'NONE',  ( 14.13034256312282189, 10.34920949090176201, -13.83076321228938887 ) ) ;
#8701 = CARTESIAN_POINT ( 'NONE',  ( 159.5152310637604671, -9.999999999999998224, -13.05155085951651195 ) ) ;
#8702 = VERTEX_POINT ( 'NONE', #11727 ) ;
#8703 = LINE ( 'NONE', #10702, #29380 ) ;
#8704 = CARTESIAN_POINT ( 'NONE',  ( 12.79001206111077948, 7.640833942120977440, -14.89903028090515136 ) ) ;
#8705 = CARTESIAN_POINT ( 'NONE',  ( 2.500000000000000444, 1.178949249685215417, 2.041999999999998483 ) ) ;
#8706 = CARTESIAN_POINT ( 'NONE',  ( 154.5152310637605240, -4.999999999999976019, -21.71180489736091346 ) ) ;
#8707 = ORIENTED_EDGE ( 'NONE', *, *, #24180, .T. ) ;
#8708 = LINE ( 'NONE', #8410, #8131 ) ;
#8709 = ORIENTED_EDGE ( 'NONE', *, *, #234, .T. ) ;
#8710 = CARTESIAN_POINT ( 'NONE',  ( 10.35864918915110877, 16.97212501191939538, -17.94384837343789485 ) ) ;
#8711 = VECTOR ( 'NONE', #15520, 1000.000000000000000 ) ;
#8712 = CARTESIAN_POINT ( 'NONE',  ( 36.54859390954302967, -21.18451583373416014, -15.55638201429745848 ) ) ;
#8713 = CARTESIAN_POINT ( 'NONE',  ( 18.04049687913209610, 0.8262538513465327306, -14.27019888128743297 ) ) ;
#8714 = VERTEX_POINT ( 'NONE', #5171 ) ;
#8715 = VERTEX_POINT ( 'NONE', #2901 ) ;
#8716 = LINE ( 'NONE', #17866, #890 ) ;
#8717 = FACE_OUTER_BOUND ( 'NONE', #13862, .T. ) ;
#8718 = CLOSED_SHELL ( 'NONE', ( #9615, #30063, #5549, #2387, #15377, #3785, #3477, #23204, #20365, #3040, #22166, #4662, #12438, #1304, #7235, #8238, #15208, #26364, #24022, #2305, #12214, #14305, #27399, #5752, #15087, #21129, #2897, #4184 ) ) ;
#8719 = CARTESIAN_POINT ( 'NONE',  ( 25.01196530022370368, -10.21768535905550124, -13.66937216179565517 ) ) ;
#8720 = CARTESIAN_POINT ( 'NONE',  ( 25.25756851182965335, -6.311239348595019116, -19.54001279501058264 ) ) ;
#8721 = ORIENTED_EDGE ( 'NONE', *, *, #1806, .T. ) ;
#8722 = ORIENTED_EDGE ( 'NONE', *, *, #24223, .T. ) ;
#8723 = DIRECTION ( 'NONE',  ( 1.000000000000000000, 2.698458740408365879E-16, -1.110223024625156540E-16 ) ) ;
#8724 = ADVANCED_FACE ( 'NONE', ( #9283 ), #18754, .T. ) ;
#8725 = FACE_OUTER_BOUND ( 'NONE', #5615, .T. ) ;
#8726 = AXIS2_PLACEMENT_3D ( 'NONE', #25673, #19099, #12370 ) ;
#8727 = CARTESIAN_POINT ( 'NONE',  ( 133.7287565553229172, -4.999999999999982236, -36.50000000000000711 ) ) ;
#8728 = DIRECTION ( 'NONE',  ( 1.000000000000000000, -0.000000000000000000, -0.000000000000000000 ) ) ;
#8729 = CARTESIAN_POINT ( 'NONE',  ( 11.22589550380084411, 9.082134330754477958, -17.24077175062176082 ) ) ;
#8730 = CARTESIAN_POINT ( 'NONE',  ( 12.49977518293622758, 8.570603418560722275, -15.13035415120363325 ) ) ;
#8731 = CARTESIAN_POINT ( 'NONE',  ( 27.39958189869922123, -12.72506959635235368, -13.65552181841346524 ) ) ;
#8732 = ORIENTED_EDGE ( 'NONE', *, *, #14874, .T. ) ;
#8733 = CARTESIAN_POINT ( 'NONE',  ( 147.0152310637605524, -10.00000000000000178, -17.38167787843871182 ) ) ;
#8734 = ORIENTED_EDGE ( 'NONE', *, *, #26052, .F. ) ;
#8735 = LINE ( 'NONE', #15462, #22934 ) ;
#8736 = EDGE_LOOP ( 'NONE', ( #4589, #27826, #11695, #7069 ) ) ;
#8737 = DIRECTION ( 'NONE',  ( 0.9510565162951536422, 2.566386769018988816E-16, 0.3090169943749472292 ) ) ;
#8738 = CARTESIAN_POINT ( 'NONE',  ( 18.26505246421942275, 9.297698622231314047, -17.43849025199569169 ) ) ;
#8739 = DIRECTION ( 'NONE',  ( -1.000000000000000000, 0.000000000000000000, 1.779203565104417375E-16 ) ) ;
#8740 = LINE ( 'NONE', #18511, #6305 ) ;
#8742 = EDGE_LOOP ( 'NONE', ( #12322, #1350, #5746, #28860 ) ) ;
#8741 = CARTESIAN_POINT ( 'NONE',  ( 21.54098841764929873, -5.100688324319140321, -15.19385678519978633 ) ) ;
#8743 = ORIENTED_EDGE ( 'NONE', *, *, #23877, .T. ) ;
#8744 = CARTESIAN_POINT ( 'NONE',  ( 172.7287565553229456, -3.999999999999989786, 0.5000000000000029976 ) ) ;
#8745 = CARTESIAN_POINT ( 'NONE',  ( 12.24523703128252983, 9.516147632761573050, -15.33322559543412034 ) ) ;
#8746 = CARTESIAN_POINT ( 'NONE',  ( 33.43446274600908907, -12.68684440242773448, -19.71889742777951327 ) ) ;
#8747 = DIRECTION ( 'NONE',  ( 0.3090169943749472292, 8.338696094057992503E-17, -0.9510565162951536422 ) ) ;
#8748 = CARTESIAN_POINT ( 'NONE',  ( 28.09718568327657806, -5.958257988085632562, -17.17874431236187149 ) ) ;
#8749 = LINE ( 'NONE', #18365, #19367 ) ;
#8750 = CARTESIAN_POINT ( 'NONE',  ( 22.68669718693540105, -3.283095500849226411, -14.44170700164887933 ) ) ;
#8751 = ORIENTED_EDGE ( 'NONE', *, *, #10348, .T. ) ;
#8752 = PRODUCT_DEFINITION_FORMATION_WITH_SPECIFIED_SOURCE ( 'ANY', '', #15688, .NOT_KNOWN. ) ;
#8753 = LINE ( 'NONE', #20510, #13949 ) ;
#8754 = EDGE_CURVE ( 'NONE', #7452, #19213, #18608, .T. ) ;
#8755 = EDGE_LOOP ( 'NONE', ( #16212, #2049, #13370, #22909, #14929 ) ) ;
#8756 = AXIS2_PLACEMENT_3D ( 'NONE', #4256, #22879, #27787 ) ;
#8757 = CARTESIAN_POINT ( 'NONE',  ( 15.02162844583664736, 5.759011576665847620, -14.59661587647459591 ) ) ;
#8758 = CARTESIAN_POINT ( 'NONE',  ( 29.92318863513849436, -9.020257460645494163, -14.67793329163371574 ) ) ;
#8759 = VECTOR ( 'NONE', #23307, 1000.000000000000000 ) ;
#8760 = ORIENTED_EDGE ( 'NONE', *, *, #15591, .F. ) ;
#8761 = ORIENTED_EDGE ( 'NONE', *, *, #19856, .F. ) ;
#8762 = LINE ( 'NONE', #15783, #20480 ) ;
#8763 = CARTESIAN_POINT ( 'NONE',  ( 159.7287565553229172, -1.999999999999973577, -7.839745962155603820 ) ) ;
#8764 = ORIENTED_EDGE ( 'NONE', *, *, #23303, .F. ) ;
#8765 = CARTESIAN_POINT ( 'NONE',  ( 144.7287565553230309, -1.999999999999977129, -25.16025403784439973 ) ) ;
#8766 = VECTOR ( 'NONE', #6170, 1000.000000000000000 ) ;
#8767 = DIRECTION ( 'NONE',  ( -1.000000000000000000, 0.000000000000000000, -0.000000000000000000 ) ) ;
#8768 = CARTESIAN_POINT ( 'NONE',  ( 169.7287565553229740, -1.999999999999969580, -33.82050807568879947 ) ) ;
#8769 = FACE_OUTER_BOUND ( 'NONE', #25881, .T. ) ;
#8770 = DIRECTION ( 'NONE',  ( -2.698458740408365879E-16, 1.000000000000000000, 0.000000000000000000 ) ) ;
#8771 = CARTESIAN_POINT ( 'NONE',  ( 24.97936687747968776, -7.804033356035183999, -18.74018705570338028 ) ) ;
#8772 = CARTESIAN_POINT ( 'NONE',  ( 19.85388831290292799, 7.668379621071204078, -15.62993620635094061 ) ) ;
#8774 = ORIENTED_EDGE ( 'NONE', *, *, #4535, .F. ) ;
#8773 = CARTESIAN_POINT ( 'NONE',  ( 36.01637063434644404, -20.79351858480864124, -21.36424221831693870 ) ) ;
#8775 = PLANE ( 'NONE',  #19759 ) ;
#8776 = CARTESIAN_POINT ( 'NONE',  ( 11.47029057985033340, 9.281140223223081520, -15.86198156829250117 ) ) ;
#8777 = CARTESIAN_POINT ( 'NONE',  ( 0.000000000000000000, 0.000000000000000000, -2.450000000000000622 ) ) ;
#8778 = DIRECTION ( 'NONE',  ( 0.000000000000000000, -1.000000000000000000, 1.287488025362403787E-15 ) ) ;
#8779 = CARTESIAN_POINT ( 'NONE',  ( 9.667875940510226584, 16.22734252707768832, -17.88507284477129033 ) ) ;
#8780 = CARTESIAN_POINT ( 'NONE',  ( 25.00000000000000000, 60.00000000000000711, -24.99999999999999289 ) ) ;
#8781 = ORIENTED_EDGE ( 'NONE', *, *, #27860, .F. ) ;
#8782 = CARTESIAN_POINT ( 'NONE',  ( 172.7287565553229456, -1.999999999999970468, 6.499999999999980460 ) ) ;
#8783 = CARTESIAN_POINT ( 'NONE',  ( 12.50140887008201851, 8.571324787501421127, -15.12905211845398412 ) ) ;
#8784 = VERTEX_POINT ( 'NONE', #14163 ) ;
#8785 = DIRECTION ( 'NONE',  ( 0.3090169943749472292, 8.338696094057992503E-17, -0.9510565162951536422 ) ) ;
#8786 = DIRECTION ( 'NONE',  ( -0.9510565162951536422, -2.566386769018988323E-16, 0.3090169943749475623 ) ) ;
#8787 = DIRECTION ( 'NONE',  ( -2.698458740408365879E-16, 1.000000000000000000, 0.000000000000000000 ) ) ;
#8788 = ORIENTED_EDGE ( 'NONE', *, *, #6474, .F. ) ;
#8789 = CARTESIAN_POINT ( 'NONE',  ( 13.41328399211976397, 7.640833942120977440, -15.68103545992656578 ) ) ;
#8791 = VECTOR ( 'NONE', #29778, 1000.000000000000000 ) ;
#8790 = CARTESIAN_POINT ( 'NONE',  ( 35.85321554361588170, -20.06054918781481788, -21.42207597224664894 ) ) ;
#8792 = EDGE_CURVE ( 'NONE', #16514, #23037, #25937, .T. ) ;
#8793 = ADVANCED_FACE ( 'NONE', ( #28555 ), #16459, .F. ) ;
#8794 = CARTESIAN_POINT ( 'NONE',  ( 15.57379856253263206, 2.175854586521385858, -15.33309735461106094 ) ) ;
#8795 = VECTOR ( 'NONE', #6282, 1000.000000000000000 ) ;
#8796 = ADVANCED_FACE ( 'NONE', ( #14463 ), #9587, .T. ) ;
#8797 = CARTESIAN_POINT ( 'NONE',  ( 28.35369828010231785, -12.30166555976806464, -13.00196782638265169 ) ) ;
#8798 = LINE ( 'NONE', #27164, #8209 ) ;
#8799 = EDGE_CURVE ( 'NONE', #20749, #11253, #18908, .T. ) ;
#8800 = DIRECTION ( 'NONE',  ( -0.5877852522924731371, -1.586114251531760235E-16, 0.8090169943749474513 ) ) ;
#8801 = CARTESIAN_POINT ( 'NONE',  ( 18.47998620531167902, -1.197692507188573785, -16.87724725366775402 ) ) ;
#8802 = VECTOR ( 'NONE', #14090, 1000.000000000000000 ) ;
#8803 = ORIENTED_EDGE ( 'NONE', *, *, #9409, .F. ) ;
#8804 = DIRECTION ( 'NONE',  ( -0.9510565162951536422, -2.566386769018988323E-16, 0.3090169943749475623 ) ) ;
#8805 = VERTEX_POINT ( 'NONE', #7464 ) ;
#8807 = ORIENTED_EDGE ( 'NONE', *, *, #17517, .F. ) ;
#8806 = SURFACE_STYLE_FILL_AREA ( #13087 ) ;
#8808 = LINE ( 'NONE', #18117, #9426 ) ;
#8809 = VECTOR ( 'NONE', #18239, 1000.000000000000000 ) ;
#8810 = DIRECTION ( 'NONE',  ( 0.000000000000000000, 0.000000000000000000, -1.000000000000000000 ) ) ;
#8811 = CARTESIAN_POINT ( 'NONE',  ( 35.54859390953724585, -21.18451583373416014, -17.78191007148576119 ) ) ;
#8812 = ORIENTED_EDGE ( 'NONE', *, *, #4983, .F. ) ;
#8813 = VECTOR ( 'NONE', #9195, 1000.000000000000000 ) ;
#8814 = CARTESIAN_POINT ( 'NONE',  ( 10.66857885413002727, 9.045135741668604012, -16.41124387233542592 ) ) ;
#8815 = ORIENTED_EDGE ( 'NONE', *, *, #15376, .T. ) ;
#8816 = CARTESIAN_POINT ( 'NONE',  ( 25.71553203045151292, -8.406338935355361031, -18.42709291467145150 ) ) ;
#8817 = DIRECTION ( 'NONE',  ( 0.8660254037844378194, 0.5000000000000014433, 0.000000000000000000 ) ) ;
#8818 = CARTESIAN_POINT ( 'NONE',  ( 10.35864918915110877, 16.97212501191939538, -17.91928203681695564 ) ) ;
#8819 = CARTESIAN_POINT ( 'NONE',  ( 162.0152310637604387, -4.999999999999974243, -1.798730398669517324E-14 ) ) ;
#8820 = MECHANICAL_DESIGN_GEOMETRIC_PRESENTATION_REPRESENTATION (  '', ( #3963 ), #3912 ) ;
#8821 = ORIENTED_EDGE ( 'NONE', *, *, #21387, .T. ) ;
#8822 = DIRECTION ( 'NONE',  ( -2.908569913943825554E-16, 1.000000000000000000, -6.826925868028084042E-18 ) ) ;
#8823 = DIRECTION ( 'NONE',  ( 0.000000000000000000, 1.000000000000000000, -1.287488025362403787E-15 ) ) ;
#8824 = CARTESIAN_POINT ( 'NONE',  ( 154.5152310637604955, -1.999999999999974909, -13.05155085951651195 ) ) ;
#8825 = ORIENTED_EDGE ( 'NONE', *, *, #15753, .T. ) ;
#8826 = FACE_OUTER_BOUND ( 'NONE', #23213, .T. ) ;
#8827 = ORIENTED_EDGE ( 'NONE', *, *, #10448, .F. ) ;
#8828 = CARTESIAN_POINT ( 'NONE',  ( 13.13233772467555660, 8.574708520419219937, -15.90495459411799395 ) ) ;
#8829 = EDGE_CURVE ( 'NONE', #15396, #23103, #25624, .T. ) ;
#8830 = CARTESIAN_POINT ( 'NONE',  ( 18.58771872311928774, 0.01515834859250781048, -13.77226461354315035 ) ) ;
#8831 = CARTESIAN_POINT ( 'NONE',  ( 22.36047763332208405, -4.488847068091893711, -15.41575731358746104 ) ) ;
#8832 = ORIENTED_EDGE ( 'NONE', *, *, #15588, .T. ) ;
#8833 = EDGE_CURVE ( 'NONE', #17684, #22172, #300, .T. ) ;
#8834 = CARTESIAN_POINT ( 'NONE',  ( 21.37428249720081297, 2.009508332918806151, -14.44682725892062614 ) ) ;
#8835 = CARTESIAN_POINT ( 'NONE',  ( 174.5152310637604103, -4.999999999999970690, -13.05155085951651195 ) ) ;
#8836 = EDGE_CURVE ( 'NONE', #24130, #11673, #14309, .T. ) ;
#8837 = DIRECTION ( 'NONE',  ( 2.908569913943825554E-16, -1.000000000000000000, 0.000000000000000000 ) ) ;
#8838 = VECTOR ( 'NONE', #24907, 1000.000000000000000 ) ;
#8839 = CARTESIAN_POINT ( 'NONE',  ( 20.99533150354982070, 4.487273811465053441, -19.54336078777620500 ) ) ;
#8840 = DIRECTION ( 'NONE',  ( -1.000000000000000000, 0.000000000000000000, 0.000000000000000000 ) ) ;
#8841 = CARTESIAN_POINT ( 'NONE',  ( 420.0000000000002274, 34.64101615137744972, 10.00000000000000178 ) ) ;
#8842 = ORIENTED_EDGE ( 'NONE', *, *, #12830, .F. ) ;
#8843 = CARTESIAN_POINT ( 'NONE',  ( 10.35864918915110877, 16.97212501191939538, -21.33333333332589277 ) ) ;
#8844 = CARTESIAN_POINT ( 'NONE',  ( 35.53434814243864537, -22.12051714835155281, -18.84852710552948096 ) ) ;
#8845 = CARTESIAN_POINT ( 'NONE',  ( -8.000000000000001776, -4.336808689942017736E-15, 0.000000000000000000 ) ) ;
#8846 = EDGE_LOOP ( 'NONE', ( #11736, #610, #16645, #7825 ) ) ;
#8847 = LINE ( 'NONE', #4286, #10962 ) ;
#8848 = CARTESIAN_POINT ( 'NONE',  ( 18.69974902744413470, 8.051839821468062652, -15.50866580261103955 ) ) ;
#8849 = CARTESIAN_POINT ( 'NONE',  ( 12.38124869470495781, 9.576253617860157163, -15.22482189909362660 ) ) ;
#8850 = CARTESIAN_POINT ( 'NONE',  ( 35.45944968151609800, -21.78403803824750185, -19.54251958818673174 ) ) ;
#8851 = VERTEX_POINT ( 'NONE', #602 ) ;
#8852 = EDGE_LOOP ( 'NONE', ( #15720, #1652, #533, #8875 ) ) ;
#8853 = DIRECTION ( 'NONE',  ( 0.3090169943749472292, 8.338696094057992503E-17, -0.9510565162951536422 ) ) ;
#8854 = CARTESIAN_POINT ( 'NONE',  ( 12.74961974476379289, 7.623002797808662301, -14.93122222525392928 ) ) ;
#8855 = PLANE ( 'NONE',  #22951 ) ;
#8856 = PLANE ( 'NONE',  #1353 ) ;
#8857 = ORIENTED_EDGE ( 'NONE', *, *, #14909, .T. ) ;
#8858 = CARTESIAN_POINT ( 'NONE',  ( 149.5152310637604955, -4.999999999999976907, -4.391296821672111328 ) ) ;
#8859 = ORIENTED_EDGE ( 'NONE', *, *, #9202, .F. ) ;
#8860 = CARTESIAN_POINT ( 'NONE',  ( 10.35864918915110877, 16.97212501191939538, -17.91928203681695564 ) ) ;
#8861 = CARTESIAN_POINT ( 'NONE',  ( 36.53496835490201988, -21.12330343441383818, -18.71787618725911884 ) ) ;
#8862 = CARTESIAN_POINT ( 'NONE',  ( 20.39549844898813191, -2.061726703908969505, -13.85117726305786512 ) ) ;
#8863 = VERTEX_POINT ( 'NONE', #7608 ) ;
#8864 = PRODUCT ( 'Pedal Return Coil Spring', 'Pedal Return Coil Spring', '', ( #2934 ) ) ;
#8865 = EDGE_CURVE ( 'NONE', #11598, #14522, #632, .T. ) ;
#8866 = ORIENTED_EDGE ( 'NONE', *, *, #14949, .T. ) ;
#8867 = ADVANCED_FACE ( 'NONE', ( #451 ), #23800, .T. ) ;
#8868 = DIRECTION ( 'NONE',  ( -1.000000000000000000, -2.908569913943825554E-16, 0.000000000000000000 ) ) ;
#8869 = EDGE_CURVE ( 'NONE', #14718, #29543, #24509, .T. ) ;
#8870 = ADVANCED_FACE ( 'NONE', ( #21345 ), #26244, .T. ) ;
#8871 = LINE ( 'NONE', #6594, #24490 ) ;
#8872 = CARTESIAN_POINT ( 'NONE',  ( 28.12627659338356878, -5.062120396530918498, -14.05642262879015369 ) ) ;
#8873 = CARTESIAN_POINT ( 'NONE',  ( 25.74978097135661770, 0.6894738977563982241, -15.43585696046938160 ) ) ;
#8874 = AXIS2_PLACEMENT_3D ( 'NONE', #15740, #9009, #4306 ) ;
#8875 = ORIENTED_EDGE ( 'NONE', *, *, #3678, .F. ) ;
#8876 = EDGE_LOOP ( 'NONE', ( #22397, #23555, #24311, #15870 ) ) ;
#8877 = DIRECTION ( 'NONE',  ( 0.000000000000000000, 1.000000000000000000, 0.000000000000000000 ) ) ;
#8878 = CARTESIAN_POINT ( 'NONE',  ( 161.1922820468853104, -10.00000000000000000, -2.083034168790677043 ) ) ;
#8879 = LINE ( 'NONE', #23089, #14086 ) ;
#8880 = AXIS2_PLACEMENT_3D ( 'NONE', #27056, #12672, #5818 ) ;
#8881 = DIRECTION ( 'NONE',  ( 2.908569913943825554E-16, -1.000000000000000000, 0.000000000000000000 ) ) ;
#8882 = CARTESIAN_POINT ( 'NONE',  ( 12.93612603019711571, 8.763434079353435990, -14.78257486846209545 ) ) ;
#8883 = CARTESIAN_POINT ( 'NONE',  ( 15.00000000000000000, 6.779440132085338567E-16, -4.513000000000000789 ) ) ;
#8884 = CARTESIAN_POINT ( 'NONE',  ( 158.6922820468853388, -10.00000000000000000, -6.413161187712876909 ) ) ;
#8885 = ORIENTED_EDGE ( 'NONE', *, *, #25484, .F. ) ;
#8886 = CARTESIAN_POINT ( 'NONE',  ( 163.6922820468852819, -1.999999999999972689, 2.247092850131518826 ) ) ;
#8887 = VECTOR ( 'NONE', #13684, 1000.000000000000000 ) ;
#8888 = CARTESIAN_POINT ( 'NONE',  ( 14.65865118920550714, 8.193166376910747672, -14.78953851775792216 ) ) ;
#8889 = CARTESIAN_POINT ( 'NONE',  ( 16.48213915071852398, -5.000000000000013323, -50.72680832159814912 ) ) ;
#8890 = CARTESIAN_POINT ( 'NONE',  ( 164.5152310637604671, -4.999999999999973355, -21.71180489736091346 ) ) ;
#8891 = ORIENTED_EDGE ( 'NONE', *, *, #7364, .T. ) ;
#8893 = EDGE_LOOP ( 'NONE', ( #25261, #8181, #2512, #24168 ) ) ;
#8892 = CARTESIAN_POINT ( 'NONE',  ( 25.31619048431776875, -0.2099727537683927225, -15.56338435260822628 ) ) ;
#8894 = ORIENTED_EDGE ( 'NONE', *, *, #16999, .F. ) ;
#8895 = DIRECTION ( 'NONE',  ( -0.5877852522924731371, 0.000000000000000000, 0.8090169943749474513 ) ) ;
#8896 = CARTESIAN_POINT ( 'NONE',  ( 11.05541533128794107, 17.68942332327241829, -17.91551483529627120 ) ) ;
#8897 = CARTESIAN_POINT ( 'NONE',  ( 32.91905456285188336, -11.74221475484424104, -17.14214516703887980 ) ) ;
#8898 = CARTESIAN_POINT ( 'NONE',  ( 138.6922820468853956, -1.999999999999979572, 2.247092850131519715 ) ) ;
#8899 = CARTESIAN_POINT ( 'NONE',  ( 26.72358035960067824, -3.685970424986596772, -17.59444040205794835 ) ) ;
#8900 = DIRECTION ( 'NONE',  ( 0.000000000000000000, 2.775557561562890735E-17, -1.000000000000000000 ) ) ;
#8901 = CARTESIAN_POINT ( 'NONE',  ( 20.68883037063079300, -1.960602941680898548, -15.52464631352181001 ) ) ;
#8902 = ORIENTED_EDGE ( 'NONE', *, *, #28323, .F. ) ;
#8903 = EDGE_CURVE ( 'NONE', #2266, #570, #13864, .T. ) ;
#8904 = CARTESIAN_POINT ( 'NONE',  ( 129.5152310637605808, -10.00000000000000888, -19.94844914048349338 ) ) ;
#8905 = FILL_AREA_STYLE_COLOUR ( '', #26882 ) ;
#8906 = CARTESIAN_POINT ( 'NONE',  ( 32.82164812444874968, -10.95096414870911161, -14.63344683186480211 ) ) ;
#8907 = VECTOR ( 'NONE', #10340, 1000.000000000000000 ) ;
#8908 = CARTESIAN_POINT ( 'NONE',  ( 30.22932097093386261, -9.048247045011217793, -15.48080783641366942 ) ) ;
#8909 = ORIENTED_EDGE ( 'NONE', *, *, #3440, .F. ) ;
#8910 = CARTESIAN_POINT ( 'NONE',  ( 139.5152310637606092, -1.999999999999978684, -19.94844914048349338 ) ) ;
#8911 = AXIS2_PLACEMENT_3D ( 'NONE', #24217, #19170, #19466 ) ;
#8912 = FACE_OUTER_BOUND ( 'NONE', #16935, .T. ) ;
#8913 = DIRECTION ( 'NONE',  ( 0.3090169943749475623, 8.338696094058001131E-17, 0.9510565162951536422 ) ) ;
#8914 = DIRECTION ( 'NONE',  ( 1.000000000000000000, 0.000000000000000000, 0.000000000000000000 ) ) ;
#8915 = DIRECTION ( 'NONE',  ( 1.000000000000000000, 0.000000000000000000, -0.000000000000000000 ) ) ;
#8916 = DIRECTION ( 'NONE',  ( 0.9510565162951536422, 0.000000000000000000, -0.3090169943749475623 ) ) ;
#8917 = CARTESIAN_POINT ( 'NONE',  ( 25.81628275165185116, -0.2054900511636704452, -18.66752024111776009 ) ) ;
#8918 = CARTESIAN_POINT ( 'NONE',  ( 17.94193213664724951, 0.5400182743772068417, -16.55803501089447849 ) ) ;
#8919 = EDGE_CURVE ( 'NONE', #18472, #13174, #7169, .T. ) ;
#8920 = VECTOR ( 'NONE', #27491, 1000.000000000000114 ) ;
#8921 = CARTESIAN_POINT ( 'NONE',  ( 35.94849409650817762, -20.48858525550898335, -21.40790205994406747 ) ) ;
#8922 = DIRECTION ( 'NONE',  ( -0.5877852522924731371, -1.586114251531760728E-16, -0.8090169943749474513 ) ) ;
#8923 = CARTESIAN_POINT ( 'NONE',  ( 11.47250673971808688, 9.270976631574885829, -15.86106510822916249 ) ) ;
#8924 = CARTESIAN_POINT ( 'NONE',  ( 173.6922820468853388, -1.999999999999969358, -23.73366926340167637 ) ) ;
#8925 = CARTESIAN_POINT ( 'NONE',  ( 138.6922820468854525, -4.999999999999980460, -17.92658477444275533 ) ) ;
#8926 = CARTESIAN_POINT ( 'NONE',  ( 9.667369220937283458, 16.22966640763102220, -17.88537093449073012 ) ) ;
#8927 = DIRECTION ( 'NONE',  ( -0.9510565162951536422, -2.566386769018988816E-16, -0.3090169943749472292 ) ) ;
#8928 = DIRECTION ( 'NONE',  ( 0.5877852522924731371, 0.000000000000000000, 0.8090169943749474513 ) ) ;
#8929 = CARTESIAN_POINT ( 'NONE',  ( 12.49957999542663600, 8.570517509188613658, -15.13050969259218981 ) ) ;
#8930 = ORIENTED_EDGE ( 'NONE', *, *, #19998, .F. ) ;
#8931 = LINE ( 'NONE', #18249, #16867 ) ;
#8932 = CARTESIAN_POINT ( 'NONE',  ( 173.6922820468853672, -1.999999999999968914, -32.39392330124607611 ) ) ;
#8933 = CARTESIAN_POINT ( 'NONE',  ( 132.2287565553230024, -10.00000000000000888, -20.83012701892220164 ) ) ;
#8934 = AXIS2_PLACEMENT_3D ( 'NONE', #6195, #1474, #15487 ) ;
#8935 = ORIENTED_EDGE ( 'NONE', *, *, #29954, .F. ) ;
#8936 = EDGE_CURVE ( 'NONE', #117, #21069, #21802, .T. ) ;
#8937 = VERTEX_POINT ( 'NONE', #14908 ) ;
#8938 = CARTESIAN_POINT ( 'NONE',  ( 8.965340528640792783, 16.85640380871598509, -17.50303937619785444 ) ) ;
#8939 = CARTESIAN_POINT ( 'NONE',  ( 33.15841575409167064, -12.44672528413413026, -20.67776857359057274 ) ) ;
#8940 = CARTESIAN_POINT ( 'NONE',  ( 20.63001478507949926, 2.108136148055946180, -20.13827832349858937 ) ) ;
#8941 = CARTESIAN_POINT ( 'NONE',  ( 14.69068284915647560, 4.968298739062387170, -17.53091140782979807 ) ) ;
#8942 = CARTESIAN_POINT ( 'NONE',  ( 0.000000000000000000, 0.000000000000000000, 19.04999999999997229 ) ) ;
#8943 = CARTESIAN_POINT ( 'NONE',  ( 27.64697528205969590, -2.889103667904926898, -18.32829528246118755 ) ) ;
#8944 = ORIENTED_EDGE ( 'NONE', *, *, #645, .F. ) ;
#8945 = FACE_BOUND ( 'NONE', #4840, .T. ) ;
#8947 = EDGE_LOOP ( 'NONE', ( #15622, #1574, #18575, #29313 ) ) ;
#8946 = LINE ( 'NONE', #18573, #6314 ) ;
#8948 = PLANE ( 'NONE',  #25525 ) ;
#8949 = VECTOR ( 'NONE', #28415, 1000.000000000000000 ) ;
#8950 = CARTESIAN_POINT ( 'NONE',  ( 174.5152310637604387, -9.999999999999994671, -21.71180489736091346 ) ) ;
#8951 = EDGE_CURVE ( 'NONE', #29592, #22249, #3349, .T. ) ;
#8952 = EDGE_CURVE ( 'NONE', #23002, #17166, #28710, .T. ) ;
#8953 = ADVANCED_FACE ( 'NONE', ( #12477 ), #14759, .T. ) ;
#8954 = CARTESIAN_POINT ( 'NONE',  ( 35.54859390953724585, -21.18451583373416014, -17.64281456791166391 ) ) ;
#8955 = CARTESIAN_POINT ( 'NONE',  ( 10.66806909375856627, 9.047473561677174203, -16.41145467664113156 ) ) ;
#8956 = EDGE_CURVE ( 'NONE', #12555, #4706, #3200, .T. ) ;
#8957 = CARTESIAN_POINT ( 'NONE',  ( 29.22485947447185595, -8.910266539455653501, -18.36689805200119707 ) ) ;
#8958 = CARTESIAN_POINT ( 'NONE',  ( 166.1922820468853104, -9.999999999999998224, -4.936203717676158398 ) ) ;
#8959 = CARTESIAN_POINT ( 'NONE',  ( 10.37265302513970688, 16.90790163500151166, -17.63730412279738147 ) ) ;
#8960 = CARTESIAN_POINT ( 'NONE',  ( 172.0152310637604671, -9.999999999999994671, -26.04193191628311155 ) ) ;
#8961 = LINE ( 'NONE', #29378, #17389 ) ;
#8962 = ORIENTED_EDGE ( 'NONE', *, *, #11617, .F. ) ;
#8963 = ORIENTED_EDGE ( 'NONE', *, *, #24952, .T. ) ;
#8964 = CYLINDRICAL_SURFACE ( 'NONE', #10010, 4.250000000000003553 ) ;
#8965 = CARTESIAN_POINT ( 'NONE',  ( 12.63667343406881294, 8.631100619704961119, -15.02124387326777111 ) ) ;
#8966 = EDGE_LOOP ( 'NONE', ( #1841, #22925, #13547, #21030 ) ) ;
#8967 = ORIENTED_EDGE ( 'NONE', *, *, #4950, .F. ) ;
#8968 = CARTESIAN_POINT ( 'NONE',  ( 139.7287565553230309, -1.999999999999978684, -25.16025403784439973 ) ) ;
#8969 = VERTEX_POINT ( 'NONE', #5628 ) ;
#8970 = CARTESIAN_POINT ( 'NONE',  ( 9.661883061612440926, 16.25482663361732705, -17.95086732675816776 ) ) ;
#8971 = ORIENTED_EDGE ( 'NONE', *, *, #18557, .F. ) ;
#8972 = CARTESIAN_POINT ( 'NONE',  ( 23.89160689111651337, -1.335809292830872241, -14.36923488517323477 ) ) ;
#8973 = CARTESIAN_POINT ( 'NONE',  ( 20.42254326673722531, -2.835881520377886655, -15.10989100197473789 ) ) ;
#8974 = CARTESIAN_POINT ( 'NONE',  ( 22.83681518364245022, 2.349634567491368564, -16.30468554850739338 ) ) ;
#8975 = DIRECTION ( 'NONE',  ( 0.000000000000000000, -1.000000000000000000, -0.000000000000000000 ) ) ;
#8976 = VECTOR ( 'NONE', #4354, 1000.000000000000000 ) ;
#8977 = FACE_OUTER_BOUND ( 'NONE', #1497, .T. ) ;
#8978 = CARTESIAN_POINT ( 'NONE',  ( 23.61827771231835982, -0.6465389018800060672, -13.57143891608981612 ) ) ;
#8979 = FILL_AREA_STYLE ('',( #23643 ) ) ;
#8980 = EDGE_CURVE ( 'NONE', #21422, #29780, #26547, .T. ) ;
#8981 = PLANE ( 'NONE',  #21076 ) ;
#8982 = CARTESIAN_POINT ( 'NONE',  ( 10.40163623209820365, 16.77498095339038287, -17.46874319472340176 ) ) ;
#8983 = EDGE_CURVE ( 'NONE', #10906, #26227, #14613, .T. ) ;
#8984 = CARTESIAN_POINT ( 'NONE',  ( 35.52583876341286384, -22.08228901593173177, -18.97221062538168113 ) ) ;
#8985 = PLANE ( 'NONE',  #26322 ) ;
#8986 = VERTEX_POINT ( 'NONE', #1063 ) ;
#8987 = EDGE_CURVE ( 'NONE', #11708, #2172, #29015, .T. ) ;
#8988 = EDGE_CURVE ( 'NONE', #18123, #27662, #26397, .T. ) ;
#8989 = CARTESIAN_POINT ( 'NONE',  ( 129.5152310637605808, -10.00000000000000888, -2.627941064794695691 ) ) ;
#8990 = AXIS2_PLACEMENT_3D ( 'NONE', #5103, #14697, #24038 ) ;
#8991 = EDGE_CURVE ( 'NONE', #16958, #2560, #10035, .T. ) ;
#8992 = CARTESIAN_POINT ( 'NONE',  ( 16.57956996521092918, 4.788269978297743812, -19.71382457362092566 ) ) ;
#8993 = CARTESIAN_POINT ( 'NONE',  ( 11.28117986039200815, 16.65403841451731637, -16.78246231193739035 ) ) ;
#8994 = LINE ( 'NONE', #18312, #23384 ) ;
#8995 = ORIENTED_EDGE ( 'NONE', *, *, #28841, .T. ) ;
#8996 = EDGE_LOOP ( 'NONE', ( #14630, #9613, #29087 ) ) ;
#8997 = CARTESIAN_POINT ( 'NONE',  ( 9.915538251416846194, 16.41143258624473233, -16.50493629029764264 ) ) ;
#8998 = CARTESIAN_POINT ( 'NONE',  ( 9.641364314812712166, 17.66882920855936590, -17.90209449470656722 ) ) ;
#8999 = CARTESIAN_POINT ( 'NONE',  ( 134.7287565553230024, -10.00000000000000711, -7.839745962155602044 ) ) ;
#9000 = FACE_OUTER_BOUND ( 'NONE', #5788, .T. ) ;
#9001 = CARTESIAN_POINT ( 'NONE',  ( 137.2287565553230309, -10.00000000000000533, -12.16987298107780013 ) ) ;
#9002 = VERTEX_POINT ( 'NONE', #10689 ) ;
#9003 = CARTESIAN_POINT ( 'NONE',  ( 12.92285173585636215, 9.540162674316999158, -16.07191862488577527 ) ) ;
#9004 = VECTOR ( 'NONE', #14140, 1000.000000000000000 ) ;
#9005 = CARTESIAN_POINT ( 'NONE',  ( 36.54859390953723874, -21.18451583373416014, -14.99999999999999822 ) ) ;
#9006 = CARTESIAN_POINT ( 'NONE',  ( 26.87257363757477435, -3.324124212371978082, -16.68573618535388547 ) ) ;
#9007 = CARTESIAN_POINT ( 'NONE',  ( 3.149999999999999023, 1.398881011027695624E-15, 1.700000000000000178 ) ) ;
#9008 = VERTEX_POINT ( 'NONE', #15412 ) ;
#9009 = DIRECTION ( 'NONE',  ( 0.000000000000000000, 0.000000000000000000, 1.000000000000000000 ) ) ;
#9010 = CARTESIAN_POINT ( 'NONE',  ( 27.20456514074317056, -5.347416052021189081, -13.22196079581408235 ) ) ;
#9011 = CARTESIAN_POINT ( 'NONE',  ( 25.92522129715230506, 0.6472387150544522960, -15.98534533675435299 ) ) ;
#9012 = VECTOR ( 'NONE', #21357, 1000.000000000000000 ) ;
#9013 = EDGE_LOOP ( 'NONE', ( #11764, #23071, #25959, #4467 ) ) ;
#9014 = DIRECTION ( 'NONE',  ( 0.9510565162951536422, 2.566386769018988816E-16, 0.3090169943749472292 ) ) ;
#9015 = VECTOR ( 'NONE', #23904, 1000.000000000000000 ) ;
#9016 = CARTESIAN_POINT ( 'NONE',  ( 119.7807826737523271, -4.999999999999985789, -87.02583265024875914 ) ) ;
#9017 = DIRECTION ( 'NONE',  ( 0.000000000000000000, 0.000000000000000000, 1.000000000000000000 ) ) ;
#9018 = ADVANCED_FACE ( 'NONE', ( #26749 ), #1399, .T. ) ;
#9019 = PLANE ( 'NONE',  #18260 ) ;
#9020 = VECTOR ( 'NONE', #28541, 1000.000000000000000 ) ;
#9021 = EDGE_CURVE ( 'NONE', #16825, #17911, #22138, .T. ) ;
#9022 = ADVANCED_FACE ( 'NONE', ( #8091 ), #22452, .T. ) ;
#9023 = CARTESIAN_POINT ( 'NONE',  ( 12.49899259368311988, 8.570259324921714494, -15.13097775544467005 ) ) ;
#9024 = EDGE_CURVE ( 'NONE', #16967, #24164, #13125, .T. ) ;
#9025 = CARTESIAN_POINT ( 'NONE',  ( 30.62762753239542590, -8.735908549479720620, -17.37160549233551876 ) ) ;
#9026 = DIRECTION ( 'NONE',  ( -0.8090169943749474513, -2.183098979609982436E-16, -0.5877852522924731371 ) ) ;
#9027 = ORIENTED_EDGE ( 'NONE', *, *, #19612, .F. ) ;
#9028 = AXIS2_PLACEMENT_3D ( 'NONE', #29952, #27939, #11706 ) ;
#9029 = CARTESIAN_POINT ( 'NONE',  ( 9.641350810849047548, 17.66889113945805789, -17.98596209335946128 ) ) ;
#9030 = MECHANICAL_DESIGN_GEOMETRIC_PRESENTATION_REPRESENTATION (  '', ( #17819 ), #16345 ) ;
#9031 = CARTESIAN_POINT ( 'NONE',  ( 15.15242361522499692, 5.855521407460130057, -16.92275779674541170 ) ) ;
#9032 = CARTESIAN_POINT ( 'NONE',  ( 137.0152310637605808, -4.999999999999980460, -1.521174642513229767E-14 ) ) ;
#9033 = DIRECTION ( 'NONE',  ( 0.5877852522924731371, 1.586114251531760728E-16, 0.8090169943749474513 ) ) ;
#9035 = ORIENTED_EDGE ( 'NONE', *, *, #18168, .F. ) ;
#9034 = CARTESIAN_POINT ( 'NONE',  ( 27.31974442496251143, -5.660127319198639206, -14.41990313654811651 ) ) ;
#9036 = VERTEX_POINT ( 'NONE', #26907 ) ;
#9037 = CARTESIAN_POINT ( 'NONE',  ( 4.000000000000000000, -1.549102112939128917, -2.292104661404055665 ) ) ;
#9038 = CARTESIAN_POINT ( 'NONE',  ( 12.24912255266251293, 9.517392596235749735, -15.33016477413064393 ) ) ;
#9039 = CIRCLE ( 'NONE', #3711, 8.000000000000007105 ) ;
#9040 = CARTESIAN_POINT ( 'NONE',  ( 35.54859390953724585, -22.18451583373416014, -18.06010107863414405 ) ) ;
#9041 = CARTESIAN_POINT ( 'NONE',  ( 14.79111372287554715, 6.954724682967856175, -19.27298399620107361 ) ) ;
#9042 = ORIENTED_EDGE ( 'NONE', *, *, #11288, .F. ) ;
#9043 = CARTESIAN_POINT ( 'NONE',  ( 159.5152310637605240, -1.999999999999973133, -19.94844914048349693 ) ) ;
#9044 = CARTESIAN_POINT ( 'NONE',  ( 23.12480016457037379, 1.528454477237789488, -15.53356264363713102 ) ) ;
#9045 = ORIENTED_EDGE ( 'NONE', *, *, #28003, .F. ) ;
#9046 = DIRECTION ( 'NONE',  ( -0.9510565162951536422, 0.000000000000000000, -0.3090169943749472292 ) ) ;
#9047 = CARTESIAN_POINT ( 'NONE',  ( 28.15263004948277725, -12.62334012340276779, -12.05588540746726345 ) ) ;
#9048 = CARTESIAN_POINT ( 'NONE',  ( 27.67597367917761630, -6.185689562215541670, -12.94745500973225383 ) ) ;
#9049 = CIRCLE ( 'NONE', #2268, 5.000000000000000888 ) ;
#9050 = ORIENTED_EDGE ( 'NONE', *, *, #10517, .T. ) ;
#9051 = EDGE_CURVE ( 'NONE', #29151, #25751, #1104, .T. ) ;
#9052 = LINE ( 'NONE', #11496, #3920 ) ;
#9053 = VECTOR ( 'NONE', #6174, 1000.000000000000000 ) ;
#9054 = AXIS2_PLACEMENT_3D ( 'NONE', #17450, #10739, #13026 ) ;
#9055 = CARTESIAN_POINT ( 'NONE',  ( 172.7287565553229456, -9.999999999999971578, -33.50000000000000000 ) ) ;
#9056 = CARTESIAN_POINT ( 'NONE',  ( 158.6922820468853388, -1.999999999999974465, -6.413161187712876909 ) ) ;
#9057 = CARTESIAN_POINT ( 'NONE',  ( 147.0152310637605808, -1.999999999999976241, -34.70218595412750773 ) ) ;
#9058 = EDGE_CURVE ( 'NONE', #13389, #15955, #4541, .T. ) ;
#9059 = CARTESIAN_POINT ( 'NONE',  ( 20.00000000000017053, 27.64101615137744972, 12.00000000000000178 ) ) ;
#9060 = ADVANCED_FACE ( 'NONE', ( #29371 ), #7933, .T. ) ;
#9061 = CARTESIAN_POINT ( 'NONE',  ( 142.0152310637605808, -10.00000000000000355, -26.04193191628310800 ) ) ;
#9062 = EDGE_CURVE ( 'NONE', #18724, #24484, #6115, .T. ) ;
#9063 = CARTESIAN_POINT ( 'NONE',  ( 26.30156876094583396, -3.312801620251602852, -13.23872229457767169 ) ) ;
#9064 = CARTESIAN_POINT ( 'NONE',  ( 19.42071131597032974, 7.574497315622086724, -15.00200944635056644 ) ) ;
#9065 = CARTESIAN_POINT ( 'NONE',  ( 33.88611015167484197, -15.71585695178754882, -20.89774115172086510 ) ) ;
#9066 = SURFACE_SIDE_STYLE ('',( #4511 ) ) ;
#9067 = CARTESIAN_POINT ( 'NONE',  ( 11.47269659055779378, 9.270105954394804115, -15.86098659800193644 ) ) ;
#9068 = AXIS2_PLACEMENT_3D ( 'NONE', #11942, #373, #26012 ) ;
#9069 = CARTESIAN_POINT ( 'NONE',  ( 152.2287565553229740, -1.999999999999975353, -12.16987298107780369 ) ) ;
#9070 = DIRECTION ( 'NONE',  ( 0.000000000000000000, 0.000000000000000000, -1.000000000000000000 ) ) ;
#9071 = CARTESIAN_POINT ( 'NONE',  ( 9.671924655352764688, 16.20877460471870535, -17.88339855620073848 ) ) ;
#9072 = LINE ( 'NONE', #27310, #13641 ) ;
#9073 = EDGE_LOOP ( 'NONE', ( #21391, #11479, #27776, #18935 ) ) ;
#9074 = CARTESIAN_POINT ( 'NONE',  ( 138.6922820468854241, -10.00000000000000533, -0.6060766987539614181 ) ) ;
#9075 = CARTESIAN_POINT ( 'NONE',  ( 12.48484057295006977, 8.564241722236854315, -15.14223913367768759 ) ) ;
#9076 = ORIENTED_EDGE ( 'NONE', *, *, #21639, .T. ) ;
#9077 = VECTOR ( 'NONE', #17897, 999.9999999999998863 ) ;
#9078 = CARTESIAN_POINT ( 'NONE',  ( 175.7287565553229456, -4.999999999999970690, 0.5000000000000029976 ) ) ;
#9079 = CARTESIAN_POINT ( 'NONE',  ( 132.0152310637605524, -4.999999999999982236, -8.721423840594310306 ) ) ;
#9080 = VERTEX_POINT ( 'NONE', #29524 ) ;
#9081 = AXIS2_PLACEMENT_3D ( 'NONE', #505, #18505, #25528 ) ;
#9082 = CARTESIAN_POINT ( 'NONE',  ( 16.53342136567307108, 10.04554801986687629, -15.32032680638607047 ) ) ;
#9083 = VERTEX_POINT ( 'NONE', #6272 ) ;
#9084 = ORIENTED_EDGE ( 'NONE', *, *, #13448, .F. ) ;
#9085 = CARTESIAN_POINT ( 'NONE',  ( 9.112530393872706469, 16.18137232441842954, -17.05472470070859714 ) ) ;
#9086 = CARTESIAN_POINT ( 'NONE',  ( 32.41494245136814811, -10.61148775487728813, -19.57799680467864789 ) ) ;
#9087 = AXIS2_PLACEMENT_3D ( 'NONE', #17878, #26948, #3871 ) ;
#9088 = CARTESIAN_POINT ( 'NONE',  ( 15.90442531705523876, 3.007083446286336947, -19.83189509879157697 ) ) ;
#9089 = CARTESIAN_POINT ( 'NONE',  ( 17.75014749421169213, 9.747325538739326944, -14.55496937630740639 ) ) ;
#9090 = CARTESIAN_POINT ( 'NONE',  ( -1.310872448937994594, 8.480771745766412906, -4.682649155111336725 ) ) ;
#9091 = CARTESIAN_POINT ( 'NONE',  ( 24.13298513268436452, -7.720266465098472253, -12.91035621449759496 ) ) ;
#9092 = EDGE_CURVE ( 'NONE', #19566, #26769, #6426, .T. ) ;
#9093 = VECTOR ( 'NONE', #21570, 1000.000000000000000 ) ;
#9094 = ORIENTED_EDGE ( 'NONE', *, *, #16523, .F. ) ;
#9095 = DIRECTION ( 'NONE',  ( -2.698458740408365879E-16, 1.000000000000000000, 0.000000000000000000 ) ) ;
#9097 = EDGE_LOOP ( 'NONE', ( #19962, #19464 ) ) ;
#9096 = DIRECTION ( 'NONE',  ( -0.000000000000000000, -0.000000000000000000, -1.000000000000000000 ) ) ;
#9098 = CONICAL_SURFACE ( 'NONE', #3277, 8.000000000000007105, 1.047197551196596077 ) ;
#9099 = CARTESIAN_POINT ( 'NONE',  ( 164.5152310637604955, -1.999999999999971800, -19.94844914048349693 ) ) ;
#9100 = DIRECTION ( 'NONE',  ( 1.000000000000000000, 0.000000000000000000, 0.000000000000000000 ) ) ;
#9101 = CARTESIAN_POINT ( 'NONE',  ( 34.19542162461613799, -15.10542955289956346, -18.90659549333309286 ) ) ;
#9102 = CARTESIAN_POINT ( 'NONE',  ( 10.66819573146529621, 9.046892785011555915, -16.41140230749465800 ) ) ;
#9103 = ORIENTED_EDGE ( 'NONE', *, *, #20132, .T. ) ;
#9104 = CARTESIAN_POINT ( 'NONE',  ( 26.47511176763426377, -7.718147522161595830, -18.64721581247919602 ) ) ;
#9105 = LINE ( 'NONE', #8958, #28968 ) ;
#9106 = CARTESIAN_POINT ( 'NONE',  ( 10.45306510330410177, 16.53912159438435125, -17.34933906371858114 ) ) ;
#9107 = FACE_BOUND ( 'NONE', #24867, .T. ) ;
#9108 = CARTESIAN_POINT ( 'NONE',  ( 167.0152310637604671, -1.999999999999971800, -6.958068083716895558 ) ) ;
#9109 = ORIENTED_EDGE ( 'NONE', *, *, #11151, .T. ) ;
#9110 = CARTESIAN_POINT ( 'NONE',  ( 420.0000000000002274, 34.64101615137744972, 14.00000000000000178 ) ) ;
#9111 = CIRCLE ( 'NONE', #385, 3.000000000000002665 ) ;
#9112 = LINE ( 'NONE', #27793, #14617 ) ;
#9113 = LINE ( 'NONE', #30254, #1820 ) ;
#9114 = ORIENTED_EDGE ( 'NONE', *, *, #17624, .T. ) ;
#9115 = CARTESIAN_POINT ( 'NONE',  ( 9.661901852922078149, 16.25474045427587200, -17.91339448853296901 ) ) ;
#9116 = ORIENTED_EDGE ( 'NONE', *, *, #6087, .F. ) ;
#9117 = AXIS2_PLACEMENT_3D ( 'NONE', #8009, #20207, #3592 ) ;
#9118 = CARTESIAN_POINT ( 'NONE',  ( 22.28228072301589080, -4.238876526682920698, -17.70252831752424427 ) ) ;
#9119 = CARTESIAN_POINT ( 'NONE',  ( 22.53049847760648561, -4.001888697258268124, -18.07502562731026075 ) ) ;
#9120 = CARTESIAN_POINT ( 'NONE',  ( 22.90957683611224738, 2.308586283387667581, -16.61139769879808625 ) ) ;
#9121 = DIRECTION ( 'NONE',  ( 1.000000000000000000, 4.440892098500622217E-16, 0.000000000000000000 ) ) ;
#9122 = CARTESIAN_POINT ( 'NONE',  ( 420.0000000000002274, 34.64101615137744972, 12.00000000000000178 ) ) ;
#9123 = ORIENTED_EDGE ( 'NONE', *, *, #20963, .F. ) ;
#9124 = DIRECTION ( 'NONE',  ( 1.000000000000000000, 2.698458740408365879E-16, -1.110223024625156540E-16 ) ) ;
#9125 = ADVANCED_FACE ( 'NONE', ( #12675 ), #29203, .T. ) ;
#9126 = EDGE_CURVE ( 'NONE', #26448, #12138, #8694, .T. ) ;
#9127 = CARTESIAN_POINT ( 'NONE',  ( 26.87257363757477435, -3.324124212371978082, -16.68573618535388547 ) ) ;
#9128 = FACE_OUTER_BOUND ( 'NONE', #17182, .T. ) ;
#9129 = DIRECTION ( 'NONE',  ( -0.8090169943749474513, -2.183098979609982436E-16, -0.5877852522924731371 ) ) ;
#9130 = CARTESIAN_POINT ( 'NONE',  ( 20.00000000000000711, 55.00000000000000711, 29.99999999999998579 ) ) ;
#9131 = VECTOR ( 'NONE', #17480, 1000.000000000000000 ) ;
#9132 = CARTESIAN_POINT ( 'NONE',  ( -16.00000000000017053, 34.64101615137744972, -10.00000000000000000 ) ) ;
#9133 = CARTESIAN_POINT ( 'NONE',  ( 10.35953768210033665, 16.96805026999784616, -17.84385765891457254 ) ) ;
#9134 = CARTESIAN_POINT ( 'NONE',  ( 46.75000000000000000, 0.000000000000000000, 0.000000000000000000 ) ) ;
#9135 = DIRECTION ( 'NONE',  ( -0.8090169943749474513, -2.183098979609982436E-16, 0.5877852522924731371 ) ) ;
#9136 = AXIS2_PLACEMENT_3D ( 'NONE', #28143, #7199, #16495 ) ;
#9137 = ORIENTED_EDGE ( 'NONE', *, *, #1415, .F. ) ;
#9138 = VERTEX_POINT ( 'NONE', #3981 ) ;
#9139 = CARTESIAN_POINT ( 'NONE',  ( 159.7287565553228887, -1.999999999999974021, 0.8205080756887930260 ) ) ;
#9140 = CARTESIAN_POINT ( 'NONE',  ( 16.21960234321935701, 7.070186740785398882, -14.59618053200276044 ) ) ;
#9141 = CARTESIAN_POINT ( 'NONE',  ( 11.27495124880614163, 16.68260362121340279, -16.78505081266910182 ) ) ;
#9142 = PLANE ( 'NONE',  #12659 ) ;
#9143 = ORIENTED_EDGE ( 'NONE', *, *, #20208, .F. ) ;
#9144 = ORIENTED_EDGE ( 'NONE', *, *, #18559, .T. ) ;
#9145 = CARTESIAN_POINT ( 'NONE',  ( 9.643509238790151983, 17.65899231378470446, -17.74106871770035099 ) ) ;
#9146 = CARTESIAN_POINT ( 'NONE',  ( 12.76023694501680517, 7.627675785621035764, -14.92276157399860281 ) ) ;
#9147 = FACE_OUTER_BOUND ( 'NONE', #18368, .T. ) ;
#9148 = FACE_OUTER_BOUND ( 'NONE', #3264, .T. ) ;
#9149 = ORIENTED_EDGE ( 'NONE', *, *, #3108, .T. ) ;
#9150 = EDGE_LOOP ( 'NONE', ( #29405, #24559, #9159, #28581, #27031 ) ) ;
#9151 = CARTESIAN_POINT ( 'NONE',  ( 7.347286611336969031, 4.995646404165290377, -0.4969600502617546600 ) ) ;
#9152 = ORIENTED_EDGE ( 'NONE', *, *, #6496, .F. ) ;
#9153 = CARTESIAN_POINT ( 'NONE',  ( 10.37265302513970688, 16.90790163500151166, -17.63730412279738147 ) ) ;
#9154 = CARTESIAN_POINT ( 'NONE',  ( 36.54859286093297754, -21.18451112290966165, -18.39168789611893118 ) ) ;
#9155 = CARTESIAN_POINT ( 'NONE',  ( 25.71553203045151292, -8.406338935355361031, -18.42709291467145150 ) ) ;
#9156 = VECTOR ( 'NONE', #29456, 1000.000000000000000 ) ;
#9157 = CARTESIAN_POINT ( 'NONE',  ( 130.7287565553229172, -4.999999999999982236, -19.55415080639417269 ) ) ;
#9158 = DIRECTION ( 'NONE',  ( -0.9510565162951536422, 0.000000000000000000, -0.3090169943749472292 ) ) ;
#9159 = ORIENTED_EDGE ( 'NONE', *, *, #27896, .T. ) ;
#9160 = CARTESIAN_POINT ( 'NONE',  ( 0.000000000000000000, 0.000000000000000000, 0.000000000000000000 ) ) ;
#9161 = ADVANCED_FACE ( 'NONE', ( #20003 ), #3532, .T. ) ;
#9162 = EDGE_CURVE ( 'NONE', #20741, #20699, #5969, .T. ) ;
#9163 = CARTESIAN_POINT ( 'NONE',  ( 17.81745789538532776, 7.988559130291253751, -20.18242036267038841 ) ) ;
#9164 = AXIS2_PLACEMENT_3D ( 'NONE', #29513, #8975, #13115 ) ;
#9165 = EDGE_CURVE ( 'NONE', #14471, #19412, #10982, .T. ) ;
#9166 = CARTESIAN_POINT ( 'NONE',  ( 25.25929662509423324, 0.6462067467026075818, -14.45468018858982795 ) ) ;
#9167 = ADVANCED_FACE ( 'NONE', ( #29677 ), #28797, .T. ) ;
#9168 = B_SPLINE_CURVE_WITH_KNOTS ( 'NONE', 3,
 ( #26531, #14744, #28692, #26383 ),
 .UNSPECIFIED., .F., .F.,
 ( 4, 4 ),
 ( 2.380737581781596564E-07, 0.002336974151641542981 ),
 .UNSPECIFIED. ) ;
#9169 = AXIS2_PLACEMENT_3D ( 'NONE', #16764, #24244, #29009 ) ;
#9170 = ORIENTED_EDGE ( 'NONE', *, *, #24836, .F. ) ;
#9171 = DIRECTION ( 'NONE',  ( 0.000000000000000000, 0.000000000000000000, 1.000000000000000000 ) ) ;
#9172 = CARTESIAN_POINT ( 'NONE',  ( 9.884967449281269580, -8.443187699361526910, -18.00000000000000000 ) ) ;
#9173 = DIRECTION ( 'NONE',  ( 0.000000000000000000, 0.000000000000000000, 1.000000000000000000 ) ) ;
#9174 = LINE ( 'NONE', #18499, #245 ) ;
#9175 = UNCERTAINTY_MEASURE_WITH_UNIT (LENGTH_MEASURE( 1.000000000000000082E-05 ), #23222, 'distance_accuracy_value', 'NONE');
#9176 = CARTESIAN_POINT ( 'NONE',  ( 10.38540050948072846, 18.16934103347302454, -16.97553146008864289 ) ) ;
#9177 = DIRECTION ( 'NONE',  ( -2.698458740408365879E-16, 1.000000000000000000, 0.000000000000000000 ) ) ;
#9178 = ORIENTED_EDGE ( 'NONE', *, *, #30125, .F. ) ;
#9179 = FACE_OUTER_BOUND ( 'NONE', #20250, .T. ) ;
#9180 = EDGE_LOOP ( 'NONE', ( #14048, #2657, #23018, #13556 ) ) ;
#9181 = CARTESIAN_POINT ( 'NONE',  ( 11.47155695691762212, 9.275332456566969697, -15.86145787682774078 ) ) ;
#9182 = ORIENTED_EDGE ( 'NONE', *, *, #12071, .T. ) ;
#9183 = CARTESIAN_POINT ( 'NONE',  ( 16.42791133306356599, 6.383902638027607601, -15.35376453018263199 ) ) ;
#9184 = CARTESIAN_POINT ( 'NONE',  ( -7.806255641895631925E-14, -4.618802153517044928, -2.092734410091829034 ) ) ;
#9185 = LINE ( 'NONE', #13182, #22046 ) ;
#9187 = ORIENTED_EDGE ( 'NONE', *, *, #10347, .F. ) ;
#9186 = CARTESIAN_POINT ( 'NONE',  ( 26.07968421886551980, -9.001936657367064498, -13.61655714643126913 ) ) ;
#9188 = AXIS2_PLACEMENT_3D ( 'NONE', #2301, #17590, #3869 ) ;
#9189 = ORIENTED_EDGE ( 'NONE', *, *, #13179, .F. ) ;
#9190 = DIRECTION ( 'NONE',  ( 1.110223024625156540E-16, 2.995891024602366092E-32, 1.000000000000000000 ) ) ;
#9191 = CARTESIAN_POINT ( 'NONE',  ( 11.05541533671906684, 17.68942329836457361, -17.91521986731755334 ) ) ;
#9192 = ORIENTED_EDGE ( 'NONE', *, *, #19272, .T. ) ;
#9193 = AXIS2_PLACEMENT_3D ( 'NONE', #13583, #22907, #20736 ) ;
#9194 = CARTESIAN_POINT ( 'NONE',  ( 33.33926371295168423, -12.28475995124076903, -19.67523791759492013 ) ) ;
#9195 = DIRECTION ( 'NONE',  ( -2.698458740408365879E-16, 1.000000000000000000, 0.000000000000000000 ) ) ;
#9196 = PLANE ( 'NONE',  #26703 ) ;
#9197 = CARTESIAN_POINT ( 'NONE',  ( 23.02024704684396283, -2.230829994151436679, -18.49515006079944612 ) ) ;
#9198 = ORIENTED_EDGE ( 'NONE', *, *, #26015, .F. ) ;
#9199 = CARTESIAN_POINT ( 'NONE',  ( 20.00000000000000355, 60.00000000000000711, -24.99999999999999645 ) ) ;
#9200 = CARTESIAN_POINT ( 'NONE',  ( 19.54218497767158169, 4.227554098413554229, -14.22708607227295730 ) ) ;
#9201 = CARTESIAN_POINT ( 'NONE',  ( 27.56197131007709444, -12.41890123633259435, -14.84244373703855935 ) ) ;
#9202 = EDGE_CURVE ( 'NONE', #26513, #10566, #24587, .T. ) ;
#9203 = EDGE_CURVE ( 'NONE', #15583, #22598, #4579, .T. ) ;
#9204 = EDGE_CURVE ( 'NONE', #4351, #2732, #502, .T. ) ;
#9205 = ORIENTED_EDGE ( 'NONE', *, *, #27177, .T. ) ;
#9206 = CARTESIAN_POINT ( 'NONE',  ( 0.000000000000000000, 0.000000000000000000, 0.000000000000000000 ) ) ;
#9207 = AXIS2_PLACEMENT_3D ( 'NONE', #24141, #10837, #15414 ) ;
#9208 = DIRECTION ( 'NONE',  ( -2.698458740408365879E-16, 1.000000000000000000, 0.000000000000000000 ) ) ;
#9209 = AXIS2_PLACEMENT_3D ( 'NONE', #12150, #9859, #7578 ) ;
#9210 = LINE ( 'NONE', #25413, #30081 ) ;
#9211 = CARTESIAN_POINT ( 'NONE',  ( 143.6922820468854241, -4.999999999999979572, -9.266330736598359152 ) ) ;
#9212 = CARTESIAN_POINT ( 'NONE',  ( 9.920751600319857033, 16.38752350362809551, -16.50277044458016107 ) ) ;
#9213 = CARTESIAN_POINT ( 'NONE',  ( 27.68278592340041655, -3.068913841971319112, -15.41105173719521915 ) ) ;
#9214 = CARTESIAN_POINT ( 'NONE',  ( 16.02150382621726976, 6.204807860950024789, -14.00014022580063155 ) ) ;
#9215 = CARTESIAN_POINT ( 'NONE',  ( 36.51148101492068321, -23.01778725746827803, -19.37219236604238759 ) ) ;
#9216 = SURFACE_SIDE_STYLE ('',( #13947 ) ) ;
#9217 = LINE ( 'NONE', #6960, #7401 ) ;
#9218 = DIRECTION ( 'NONE',  ( -2.698458740408365879E-16, 1.000000000000000000, 0.000000000000000000 ) ) ;
#9219 = LINE ( 'NONE', #11370, #4661 ) ;
#9220 = CARTESIAN_POINT ( 'NONE',  ( 17.32695330507268494, 5.471673316493076200, -20.08600194542987794 ) ) ;
#9221 = EDGE_LOOP ( 'NONE', ( #25685, #14817, #2163, #24551 ) ) ;
#9222 = LINE ( 'NONE', #6661, #11004 ) ;
#9223 = CARTESIAN_POINT ( 'NONE',  ( 10.33811693838771717, 18.38618951776012267, -17.97192418671890835 ) ) ;
#9224 = ORIENTED_EDGE ( 'NONE', *, *, #21340, .T. ) ;
#9225 = AXIS2_PLACEMENT_3D ( 'NONE', #14627, #9445, #23975 ) ;
#9226 = DIRECTION ( 'NONE',  ( -2.698458740408365879E-16, 1.000000000000000000, 0.000000000000000000 ) ) ;
#9227 = LINE ( 'NONE', #12134, #13699 ) ;
#9228 = CARTESIAN_POINT ( 'NONE',  ( 14.57776618122778700, 6.338444840345393239, -15.85465340776532095 ) ) ;
#9229 = VECTOR ( 'NONE', #27515, 1000.000000000000000 ) ;
#9230 = AXIS2_PLACEMENT_3D ( 'NONE', #25114, #6350, #20662 ) ;
#9231 = ORIENTED_EDGE ( 'NONE', *, *, #3571, .T. ) ;
#9232 = CARTESIAN_POINT ( 'NONE',  ( 35.54859390953724585, -23.18451583373416014, -18.19919658220850422 ) ) ;
#9233 = CARTESIAN_POINT ( 'NONE',  ( 15.68163020692053422, 2.793964495486057409, -19.44966893625607085 ) ) ;
#9234 = CARTESIAN_POINT ( 'NONE',  ( 18.31728471214517029, 9.901174664208697962, -15.18855771585127634 ) ) ;
#9235 = EDGE_CURVE ( 'NONE', #27415, #4938, #22750, .T. ) ;
#9236 = EDGE_CURVE ( 'NONE', #12198, #4960, #18157, .T. ) ;
#9237 = DIRECTION ( 'NONE',  ( -2.908569913943825554E-16, 1.000000000000000000, -6.826925868028084042E-18 ) ) ;
#9238 = EDGE_CURVE ( 'NONE', #14962, #24264, #13487, .T. ) ;
#9239 = CARTESIAN_POINT ( 'NONE',  ( 20.46682838619579670, -4.770343855991169058, -14.23415315410508342 ) ) ;
#9240 = VERTEX_POINT ( 'NONE', #20701 ) ;
#9241 = ORIENTED_EDGE ( 'NONE', *, *, #776, .F. ) ;
#9242 = DIRECTION ( 'NONE',  ( 0.3090169943749475623, 8.338696094058001131E-17, 0.9510565162951536422 ) ) ;
#9243 = AXIS2_PLACEMENT_3D ( 'NONE', #23081, #18490, #16341 ) ;
#9244 = AXIS2_PLACEMENT_3D ( 'NONE', #21852, #17271, #1119 ) ;
#9246 = ORIENTED_EDGE ( 'NONE', *, *, #19448, .F. ) ;
#9245 = LINE ( 'NONE', #28529, #14571 ) ;
#9247 = ORIENTED_EDGE ( 'NONE', *, *, #19611, .T. ) ;
#9248 = LINE ( 'NONE', #7131, #15797 ) ;
#9249 = CARTESIAN_POINT ( 'NONE',  ( 0.000000000000000000, 0.000000000000000000, -18.00000000000000000 ) ) ;
#9250 = ORIENTED_EDGE ( 'NONE', *, *, #14575, .F. ) ;
#9251 = CARTESIAN_POINT ( 'NONE',  ( 35.92974604556026463, -18.40436019371391652, -19.36057938427370217 ) ) ;
#9252 = CARTESIAN_POINT ( 'NONE',  ( 10.66667607898454939, 9.053862104998891880, -16.41203073725236905 ) ) ;
#9253 = ORIENTED_EDGE ( 'NONE', *, *, #28189, .T. ) ;
#9254 = DIRECTION ( 'NONE',  ( 0.5877852522924731371, 1.586114251531760728E-16, -0.8090169943749474513 ) ) ;
#9255 = DIRECTION ( 'NONE',  ( -0.8090169943749474513, -2.183098979609982436E-16, 0.5877852522924731371 ) ) ;
#9256 = CARTESIAN_POINT ( 'NONE',  ( 10.43477690885096720, 16.62299358534909288, -17.37687480348504820 ) ) ;
#9257 = FACE_OUTER_BOUND ( 'NONE', #25174, .T. ) ;
#9258 = PLANE ( 'NONE',  #352 ) ;
#9259 = AXIS2_PLACEMENT_3D ( 'NONE', #17604, #28652, #5421 ) ;
#9260 = ORIENTED_EDGE ( 'NONE', *, *, #17743, .F. ) ;
#9261 = CIRCLE ( 'NONE', #5874, 4.000000000000000000 ) ;
#9262 = DIRECTION ( 'NONE',  ( 0.3090169943749472292, 8.338696094057992503E-17, -0.9510565162951536422 ) ) ;
#9263 = CARTESIAN_POINT ( 'NONE',  ( 141.1922820468854241, -4.999999999999980460, -2.083034168790677043 ) ) ;
#9264 = ORIENTED_EDGE ( 'NONE', *, *, #3202, .T. ) ;
#9265 = ORIENTED_EDGE ( 'NONE', *, *, #11070, .F. ) ;
#9266 = CARTESIAN_POINT ( 'NONE',  ( 148.6922820468853956, -4.999999999999977796, -6.413161187712876909 ) ) ;
#9267 = EDGE_LOOP ( 'NONE', ( #8707, #11261, #7396, #21217 ) ) ;
#9268 = CARTESIAN_POINT ( 'NONE',  ( 9.667846996725693032, 16.22747526696303666, -17.88508502774671882 ) ) ;
#9269 = AXIS2_PLACEMENT_3D ( 'NONE', #9361, #20405, #13249 ) ;
#9270 = CARTESIAN_POINT ( 'NONE',  ( 23.59026362060683724, -1.443753810951279082, -14.18444229111703514 ) ) ;
#9271 = CARTESIAN_POINT ( 'NONE',  ( 24.16235420939608858, 2.058193855977920261, -15.89352170542055198 ) ) ;
#9272 = CARTESIAN_POINT ( 'NONE',  ( 16.29141254853644227, 2.771581735061156682, -15.76764191790683611 ) ) ;
#9273 = PLANE ( 'NONE',  #14045 ) ;
#9274 = CARTESIAN_POINT ( 'NONE',  ( 6.505213034913026604E-15, 9.237604307034033013, -5.000000000000000888 ) ) ;
#9275 = EDGE_CURVE ( 'NONE', #17847, #6680, #6843, .T. ) ;
#9276 = LINE ( 'NONE', #599, #19592 ) ;
#9277 = EDGE_CURVE ( 'NONE', #10473, #17748, #8661, .T. ) ;
#9278 = CARTESIAN_POINT ( 'NONE',  ( 23.63863231746517712, -2.790269051896475450, -19.68844555248840678 ) ) ;
#9279 = APPLICATION_CONTEXT ( 'automotive_design' ) ;
#9280 = ORIENTED_EDGE ( 'NONE', *, *, #15028, .F. ) ;
#9281 =( LENGTH_UNIT ( ) NAMED_UNIT ( * ) SI_UNIT ( .MILLI., .METRE. ) );
#9282 = AXIS2_PLACEMENT_3D ( 'NONE', #28247, #7299, #18741 ) ;
#9283 = FACE_OUTER_BOUND ( 'NONE', #17971, .T. ) ;
#9284 = SURFACE_STYLE_USAGE ( .BOTH. , #9431 ) ;
#9285 = VECTOR ( 'NONE', #6216, 1000.000000000000000 ) ;
#9286 = CARTESIAN_POINT ( 'NONE',  ( 7.340088617936617155, -5.000000000000015987, 22.59046990083097484 ) ) ;
#9287 = CARTESIAN_POINT ( 'NONE',  ( 173.6922820468852535, -9.999999999999996447, 2.247092850131519715 ) ) ;
#9288 = CARTESIAN_POINT ( 'NONE',  ( 10.35864918915110877, 16.97212501191939538, -17.94384837343789485 ) ) ;
#9289 = CARTESIAN_POINT ( 'NONE',  ( 35.54787733059053778, -22.18129662410796854, -18.46719521006932396 ) ) ;
#9290 = COLOUR_RGB ( '', 0.40784314, 0.44705882, 0.49803922) ;
#9291 = CARTESIAN_POINT ( 'NONE',  ( 32.63711423693117553, -11.05166607373017484, -18.34576405707344549 ) ) ;
#9292 = ORIENTED_EDGE ( 'NONE', *, *, #26050, .T. ) ;
#9293 = CARTESIAN_POINT ( 'NONE',  ( 12.82830918206423121, 7.509569466653498004, -16.13756579491948173 ) ) ;
#9294 = VERTEX_POINT ( 'NONE', #13697 ) ;
#9295 = CARTESIAN_POINT ( 'NONE',  ( 134.5152310637605524, -10.00000000000000533, -30.37205893520530964 ) ) ;
#9296 = EDGE_CURVE ( 'NONE', #14128, #18267, #11205, .T. ) ;
#9297 = CARTESIAN_POINT ( 'NONE',  ( 20.23291344124205793, 5.521974472852556381, -14.51730806008046137 ) ) ;
#9298 = CARTESIAN_POINT ( 'NONE',  ( 11.28624536866114347, 16.63080734789289750, -16.78036754607827064 ) ) ;
#9299 = CARTESIAN_POINT ( 'NONE',  ( 35.54502023521215648, -22.16846120802060938, -18.59538644662325524 ) ) ;
#9300 = ORIENTED_EDGE ( 'NONE', *, *, #5852, .F. ) ;
#9301 = EDGE_CURVE ( 'NONE', #17531, #27161, #27926, .T. ) ;
#9302 = ORIENTED_EDGE ( 'NONE', *, *, #1417, .F. ) ;
#9303 = CARTESIAN_POINT ( 'NONE',  ( 9.641350810849047548, 17.66889113945805789, -17.91752729848689185 ) ) ;
#9304 = CARTESIAN_POINT ( 'NONE',  ( 129.5152310637605808, -10.00000000000000888, -28.60870317832789311 ) ) ;
#9305 = PRODUCT_DEFINITION ( 'UNKNOWN', '', #2946, #17406 ) ;
#9306 = CARTESIAN_POINT ( 'NONE',  ( 9.641351654859628084, 17.66888726871794191, -17.91235298298990841 ) ) ;
#9307 = LINE ( 'NONE', #8345, #27864 ) ;
#9308 = DIRECTION ( 'NONE',  ( -2.698458740408365879E-16, 1.000000000000000000, 0.000000000000000000 ) ) ;
#9309 = VERTEX_POINT ( 'NONE', #6690 ) ;
#9310 = CARTESIAN_POINT ( 'NONE',  ( 5.690023276062400548, 5.952467836904161480, -4.869346954796185400 ) ) ;
#9311 = VERTEX_POINT ( 'NONE', #6988 ) ;
#9312 = CARTESIAN_POINT ( 'NONE',  ( 10.36219267574928260, 16.95587413069128857, -17.77286471925143019 ) ) ;
#9313 = VECTOR ( 'NONE', #28048, 1000.000000000000000 ) ;
#9314 = VECTOR ( 'NONE', #21742, 1000.000000000000000 ) ;
#9316 = VECTOR ( 'NONE', #20799, 1000.000000000000000 ) ;
#9315 = CARTESIAN_POINT ( 'NONE',  ( 36.54859195715578579, -22.18450706271777406, -18.40832622446962930 ) ) ;
#9317 = CARTESIAN_POINT ( 'NONE',  ( 26.80628776457338347, -3.176708023846821494, -16.02594779711905559 ) ) ;
#9318 = CARTESIAN_POINT ( 'NONE',  ( 152.0152310637604955, -1.999999999999976241, -15.61832212156129351 ) ) ;
#9319 = DIRECTION ( 'NONE',  ( 6.938893903907227392E-16, -0.000000000000000000, 1.000000000000000000 ) ) ;
#9320 = ORIENTED_EDGE ( 'NONE', *, *, #2413, .F. ) ;
#9321 = DIRECTION ( 'NONE',  ( 0.9237280213470682178, 0.3830490080632377725, 0.000000000000000000 ) ) ;
#9322 = CARTESIAN_POINT ( 'NONE',  ( 18.55323344277375242, 5.040171350539718098, -19.22783755317104237 ) ) ;
#9323 = CARTESIAN_POINT ( 'NONE',  ( 27.33932411720343936, -8.205422078888220838, -18.29166945089792407 ) ) ;
#9324 = ORIENTED_EDGE ( 'NONE', *, *, #23597, .F. ) ;
#9325 = FACE_BOUND ( 'NONE', #24721, .T. ) ;
#9326 = LINE ( 'NONE', #22942, #23775 ) ;
#9327 = DIRECTION ( 'NONE',  ( -0.8090169943749474513, -2.183098979609982436E-16, -0.5877852522924731371 ) ) ;
#9328 = LINE ( 'NONE', #29873, #19719 ) ;
#9329 = CARTESIAN_POINT ( 'NONE',  ( 10.72588575366639674, 16.60783230186494563, -15.95209284586258214 ) ) ;
#9330 = CARTESIAN_POINT ( 'NONE',  ( 159.7287565553230024, -9.999999999999998224, -33.82050807568879947 ) ) ;
#9331 = ADVANCED_FACE ( 'NONE', ( #18269 ), #27778, .F. ) ;
#9332 = ADVANCED_FACE ( 'NONE', ( #18427 ), #17965, .T. ) ;
#9333 = CYLINDRICAL_SURFACE ( 'NONE', #4172, 1.500000000000001332 ) ;
#9334 = ORIENTED_EDGE ( 'NONE', *, *, #24659, .T. ) ;
#9335 = CARTESIAN_POINT ( 'NONE',  ( 11.47250673971808688, 9.270976631574885829, -15.86106510822916249 ) ) ;
#9336 = EDGE_CURVE ( 'NONE', #722, #756, #29644, .T. ) ;
#9337 = VERTEX_POINT ( 'NONE', #4543 ) ;
#9338 = CARTESIAN_POINT ( 'NONE',  ( 17.81918496738754953, 9.416330548141603529, -16.00206777915198586 ) ) ;
#9339 = DIRECTION ( 'NONE',  ( 0.000000000000000000, 0.000000000000000000, 1.000000000000000000 ) ) ;
#9340 = DIRECTION ( 'NONE',  ( -0.9510565162951536422, -2.566386769018988323E-16, 0.3090169943749475623 ) ) ;
#9341 = EDGE_CURVE ( 'NONE', #11366, #6539, #16131, .T. ) ;
#9342 = CARTESIAN_POINT ( 'NONE',  ( 29.72799312938100513, -7.689056491358781997, -15.42978383025728384 ) ) ;
#9343 = EDGE_LOOP ( 'NONE', ( #24837, #2687, #9549, #9114, #26888 ) ) ;
#9344 = FACE_OUTER_BOUND ( 'NONE', #591, .T. ) ;
#9345 = CARTESIAN_POINT ( 'NONE',  ( 11.05610776857519184, 17.68624771760786274, -17.82814161748832760 ) ) ;
#9346 = ORIENTED_EDGE ( 'NONE', *, *, #17248, .T. ) ;
#9347 = CARTESIAN_POINT ( 'NONE',  ( 35.54859390953724585, -22.18451583373416014, -17.64281456791166036 ) ) ;
#9348 = CARTESIAN_POINT ( 'NONE',  ( 14.93287775521291394, 9.378568215907955974, -14.88591063491414168 ) ) ;
#9349 = PLANE ( 'NONE',  #17402 ) ;
#9350 = VECTOR ( 'NONE', #1544, 999.9999999999998863 ) ;
#9351 = CARTESIAN_POINT ( 'NONE',  ( 25.66261690555348807, -4.931278859741150100, -13.05994810794548933 ) ) ;
#9352 = ORIENTED_EDGE ( 'NONE', *, *, #6530, .T. ) ;
#9353 = CARTESIAN_POINT ( 'NONE',  ( -8.000000000000000000, 4.618802153517028941, -4.285468820183664818 ) ) ;
#9354 = CARTESIAN_POINT ( 'NONE',  ( 17.97606266963480692, 4.724414365053664966, -20.23074386977120298 ) ) ;
#9355 = CARTESIAN_POINT ( 'NONE',  ( 16.67011857490315307, 4.279483903030143921, -15.63504347475558198 ) ) ;
#9356 = ORIENTED_EDGE ( 'NONE', *, *, #17873, .T. ) ;
#9357 = CARTESIAN_POINT ( 'NONE',  ( -3.344563996438223885, -2.687817229851500844, -2.291324518471496319 ) ) ;
#9358 = VECTOR ( 'NONE', #15562, 1000.000000000000000 ) ;
#9359 = DIRECTION ( 'NONE',  ( -0.5877852522924731371, -1.586114251531760235E-16, 0.8090169943749474513 ) ) ;
#9360 = FACE_OUTER_BOUND ( 'NONE', #2862, .T. ) ;
#9361 = CARTESIAN_POINT ( 'NONE',  ( 162.0152310637604103, -9.999999999999998224, -0.06116980274991495881 ) ) ;
#9362 = DIRECTION ( 'NONE',  ( 0.3090169943749472292, 8.338696094057992503E-17, -0.9510565162951536422 ) ) ;
#9363 = VECTOR ( 'NONE', #23640, 999.9999999999998863 ) ;
#9364 = CARTESIAN_POINT ( 'NONE',  ( 9.898178882064430084, 16.49104486689975246, -16.51464960819000893 ) ) ;
#9365 = CARTESIAN_POINT ( 'NONE',  ( 24.68698569862014480, -7.792836496385216805, -13.74806253080685359 ) ) ;
#9366 = CARTESIAN_POINT ( 'NONE',  ( 22.28231863826031756, 1.183864898644814811, -18.90614694914491167 ) ) ;
#9367 = EDGE_CURVE ( 'NONE', #10926, #13095, #20557, .T. ) ;
#9369 = VERTEX_POINT ( 'NONE', #13543 ) ;
#9368 = CARTESIAN_POINT ( 'NONE',  ( 31.50466570323033011, -10.22776944099620877, -17.14799365788790553 ) ) ;
#9370 = CARTESIAN_POINT ( 'NONE',  ( 13.00000000000000178, -2.870178842070716726E-15, 23.00000000000000000 ) ) ;
#9371 = ADVANCED_FACE ( 'NONE', ( #2421 ), #11104, .T. ) ;
#9372 = EDGE_CURVE ( 'NONE', #24060, #18723, #27481, .T. ) ;
#9373 = LINE ( 'NONE', #25885, #3949 ) ;
#9374 = DIRECTION ( 'NONE',  ( 0.5877852522924731371, 1.586114251531760728E-16, 0.8090169943749474513 ) ) ;
#9375 = EDGE_CURVE ( 'NONE', #209, #13070, #30238, .T. ) ;
#9377 = ORIENTED_EDGE ( 'NONE', *, *, #2071, .T. ) ;
#9376 = CARTESIAN_POINT ( 'NONE',  ( 15.46244301724551740, 3.702889819443702990, -17.82701508041758842 ) ) ;
#9378 = ORIENTED_EDGE ( 'NONE', *, *, #19996, .F. ) ;
#9379 = LINE ( 'NONE', #7106, #25158 ) ;
#9380 = CARTESIAN_POINT ( 'NONE',  ( 10.33812163068573575, 18.38616799828327686, -17.90626694547636433 ) ) ;
#9381 = ORIENTED_EDGE ( 'NONE', *, *, #27325, .T. ) ;
#9382 = DIRECTION ( 'NONE',  ( -0.5877852522924731371, -1.586114251531760728E-16, -0.8090169943749474513 ) ) ;
#9383 = DIRECTION ( 'NONE',  ( 0.000000000000000000, 0.000000000000000000, -1.000000000000000000 ) ) ;
#9384 = AXIS2_PLACEMENT_3D ( 'NONE', #10531, #3383, #19839 ) ;
#9385 = CARTESIAN_POINT ( 'NONE',  ( 16.34386185847872142, 4.569898679961749366, -19.52586945278800812 ) ) ;
#9386 = ORIENTED_EDGE ( 'NONE', *, *, #25069, .F. ) ;
#9387 = CARTESIAN_POINT ( 'NONE',  ( 27.68941694697105760, -11.75984073208553582, -11.85267853464266352 ) ) ;
#9388 = VERTEX_POINT ( 'NONE', #25013 ) ;
#9389 = CARTESIAN_POINT ( 'NONE',  ( 34.96958981470057637, -20.58335714263341387, -21.20026138435576613 ) ) ;
#9390 = CARTESIAN_POINT ( 'NONE',  ( 25.36902537161520499, -2.228419832982303728, -15.31576610616191481 ) ) ;
#9391 = CARTESIAN_POINT ( 'NONE',  ( 14.24687995347741420, 8.287322832548987606, -13.87414582376881000 ) ) ;
#9392 = AXIS2_PLACEMENT_3D ( 'NONE', #11988, #26059, #5592 ) ;
#9393 = CARTESIAN_POINT ( 'NONE',  ( 29.48152472672500579, -5.877396966218813468, -15.70213184580788379 ) ) ;
#9394 = ORIENTED_EDGE ( 'NONE', *, *, #16549, .F. ) ;
#9395 = LINE ( 'NONE', #28834, #22575 ) ;
#9397 = EDGE_LOOP ( 'NONE', ( #9944, #6416, #13489, #16046 ) ) ;
#9396 = DIRECTION ( 'NONE',  ( -1.110223024625156540E-16, 0.000000000000000000, -1.000000000000000000 ) ) ;
#9398 = ORIENTED_EDGE ( 'NONE', *, *, #18759, .T. ) ;
#9399 = DIRECTION ( 'NONE',  ( -0.5877852522924731371, -1.586114251531760235E-16, 0.8090169943749474513 ) ) ;
#9400 = CARTESIAN_POINT ( 'NONE',  ( 133.6922820468854241, -1.999999999999981348, -17.92658477444275533 ) ) ;
#9401 = CARTESIAN_POINT ( 'NONE',  ( 36.54859390953724585, -21.18451583373416014, -18.19919658220850422 ) ) ;
#9402 = CARTESIAN_POINT ( 'NONE',  ( 12.75517096047518173, 7.625437268557950787, -14.92679923539383680 ) ) ;
#9403 = EDGE_LOOP ( 'NONE', ( #18925, #14830, #12314, #18836 ) ) ;
#9404 = EDGE_CURVE ( 'NONE', #28119, #8559, #27339, .T. ) ;
#9405 = VECTOR ( 'NONE', #3134, 1000.000000000000000 ) ;
#9406 = CARTESIAN_POINT ( 'NONE',  ( 146.1922820468854241, -10.00000000000000355, -10.74328820663507678 ) ) ;
#9407 = DIRECTION ( 'NONE',  ( 0.000000000000000000, 0.000000000000000000, -1.000000000000000000 ) ) ;
#9408 = EDGE_CURVE ( 'NONE', #5618, #15809, #22720, .T. ) ;
#9409 = EDGE_CURVE ( 'NONE', #12138, #29920, #22867, .T. ) ;
#9410 = CARTESIAN_POINT ( 'NONE',  ( 10.47103768343372288, 16.45669705093847313, -17.33522727542475295 ) ) ;
#9411 = CARTESIAN_POINT ( 'NONE',  ( 102.8198706071908219, -4.999999999999989342, 74.70300872013253013 ) ) ;
#9412 = EDGE_CURVE ( 'NONE', #4141, #28792, #1976, .T. ) ;
#9413 = LINE ( 'NONE', #18738, #8059 ) ;
#9414 = ORIENTED_EDGE ( 'NONE', *, *, #13525, .T. ) ;
#9415 = DIRECTION ( 'NONE',  ( -0.9510565162951536422, 0.000000000000000000, -0.3090169943749472292 ) ) ;
#9416 = CARTESIAN_POINT ( 'NONE',  ( 5.828767459767482784, -5.000000000000015987, 17.93910165294919423 ) ) ;
#9417 = CARTESIAN_POINT ( 'NONE',  ( 169.7287565553228603, -9.999999999999998224, 0.8205080756887930260 ) ) ;
#9418 = ORIENTED_EDGE ( 'NONE', *, *, #6299, .F. ) ;
#9419 = CARTESIAN_POINT ( 'NONE',  ( 11.14294825671155209, 9.462472856991839265, -17.27507855072861176 ) ) ;
#9420 = CARTESIAN_POINT ( 'NONE',  ( 27.25745087693901425, -5.581270904725432302, -18.17424208600867175 ) ) ;
#9421 = CARTESIAN_POINT ( 'NONE',  ( 17.97606266963480692, 4.724414365053664966, -20.23074386977120298 ) ) ;
#9422 = DIRECTION ( 'NONE',  ( 0.5877852522924731371, 1.586114251531760728E-16, 0.8090169943749474513 ) ) ;
#9423 = DIRECTION ( 'NONE',  ( -2.698458740408365879E-16, 1.000000000000000000, 0.000000000000000000 ) ) ;
#9424 = CARTESIAN_POINT ( 'NONE',  ( 164.5152310637604671, -1.999999999999971800, -21.71180489736091346 ) ) ;
#9425 = CARTESIAN_POINT ( 'NONE',  ( 23.77086030874127687, -7.150112426529108944, -14.59934731766091431 ) ) ;
#9426 = VECTOR ( 'NONE', #27777, 1000.000000000000000 ) ;
#9427 = ORIENTED_EDGE ( 'NONE', *, *, #22591, .F. ) ;
#9428 = LINE ( 'NONE', #20885, #27179 ) ;
#9429 = EDGE_CURVE ( 'NONE', #13842, #23922, #26535, .T. ) ;
#9430 = CARTESIAN_POINT ( 'NONE',  ( 132.0152310637605808, -10.00000000000000711, -6.958068083716893781 ) ) ;
#9431 = SURFACE_SIDE_STYLE ('',( #15451 ) ) ;
#9432 = DIRECTION ( 'NONE',  ( -0.8090169943749474513, -2.183098979609982436E-16, -0.5877852522924731371 ) ) ;
#9433 = LINE ( 'NONE', #12033, #24581 ) ;
#9434 = CARTESIAN_POINT ( 'NONE',  ( 10.35887147716723611, 16.97110557074245563, -17.87975733919941845 ) ) ;
#9435 = CARTESIAN_POINT ( 'NONE',  ( 35.32886446602115171, -21.19738783794349857, -20.03221113960638178 ) ) ;
#9436 = CARTESIAN_POINT ( 'NONE',  ( 33.44337896868773186, -12.72690026786775341, -19.72159258799634074 ) ) ;
#9437 = ORIENTED_EDGE ( 'NONE', *, *, #29953, .F. ) ;
#9438 = CARTESIAN_POINT ( 'NONE',  ( 8.944585198251687075, 16.95159039956950764, -17.91368623377419667 ) ) ;
#9439 = ORIENTED_EDGE ( 'NONE', *, *, #13100, .T. ) ;
#9440 = ADVANCED_FACE ( 'NONE', ( #7580 ), #21312, .T. ) ;
#9441 = LINE ( 'NONE', #12337, #13422 ) ;
#9442 = CARTESIAN_POINT ( 'NONE',  ( 20.22088415693689356, -1.238650738454883493, -19.72259765018230482 ) ) ;
#9443 = EDGE_CURVE ( 'NONE', #18076, #14, #421, .T. ) ;
#9444 = CARTESIAN_POINT ( 'NONE',  ( 11.27239417409149880, 16.69433069180593776, -16.78622300611779750 ) ) ;
#9445 = DIRECTION ( 'NONE',  ( -1.000000000000000000, 0.000000000000000000, 0.000000000000000000 ) ) ;
#9446 = EDGE_CURVE ( 'NONE', #506, #29222, #28385, .T. ) ;
#9447 = ORIENTED_EDGE ( 'NONE', *, *, #6440, .T. ) ;
#9448 = VERTEX_POINT ( 'NONE', #19321 ) ;
#9449 = CARTESIAN_POINT ( 'NONE',  ( 9.641351021852148762, 17.66889017177091503, -17.91406276888456617 ) ) ;
#9450 = DIRECTION ( 'NONE',  ( -2.698458740408365879E-16, 1.000000000000000000, 0.000000000000000000 ) ) ;
#9451 = VECTOR ( 'NONE', #3910, 1000.000000000000000 ) ;
#9452 = CARTESIAN_POINT ( 'NONE',  ( 9.915248083523094280, 16.41276333319327918, -16.50506225043874409 ) ) ;
#9453 = CARTESIAN_POINT ( 'NONE',  ( 158.6922820468854241, -1.999999999999973133, -35.24709285013155835 ) ) ;
#9454 = DIRECTION ( 'NONE',  ( 0.3090169943749472292, 8.338696094057992503E-17, -0.9510565162951536422 ) ) ;
#9455 = VERTEX_POINT ( 'NONE', #28532 ) ;
#9456 = CARTESIAN_POINT ( 'NONE',  ( 4.680456609903983711, 6.535341423375600201, -0.01688885742777455554 ) ) ;
#9457 = ORIENTED_EDGE ( 'NONE', *, *, #13723, .F. ) ;
#9458 = CARTESIAN_POINT ( 'NONE',  ( 10.47401950373780899, 16.44302204293020964, -17.33397781699859053 ) ) ;
#9459 = EDGE_LOOP ( 'NONE', ( #10365, #28747, #3260, #28190 ) ) ;
#9460 = CARTESIAN_POINT ( 'NONE',  ( 36.54859390953724585, -22.18451583373416014, -17.99055332684694974 ) ) ;
#9461 = CARTESIAN_POINT ( 'NONE',  ( 31.81434894052502571, -10.04473835610349575, -15.03854332269495764 ) ) ;
#9462 = CARTESIAN_POINT ( 'NONE',  ( 26.36224721256908410, -8.875037662531589433, -13.49479840426202948 ) ) ;
#9463 = EDGE_LOOP ( 'NONE', ( #7479, #12848, #7043, #191 ) ) ;
#9464 = DIRECTION ( 'NONE',  ( -0.9510565162951536422, -2.566386769018988323E-16, 0.3090169943749475623 ) ) ;
#9465 = EDGE_LOOP ( 'NONE', ( #27291, #10968, #2837, #19161 ) ) ;
#9466 = VECTOR ( 'NONE', #5824, 1000.000000000000000 ) ;
#9467 = CARTESIAN_POINT ( 'NONE',  ( 33.16581763841239194, -10.35476010881584052, -17.60936685258081624 ) ) ;
#9468 = CARTESIAN_POINT ( 'NONE',  ( 0.000000000000000000, 0.000000000000000000, -28.00000000000000000 ) ) ;
#9469 = CARTESIAN_POINT ( 'NONE',  ( 18.16542447708646790, 4.701683080007062365, -19.22226433900947029 ) ) ;
#9470 = CARTESIAN_POINT ( 'NONE',  ( 27.04128250769109698, -11.23896722199365961, -17.17396923023889244 ) ) ;
#9471 = ORIENTED_EDGE ( 'NONE', *, *, #22631, .F. ) ;
#9472 = EDGE_CURVE ( 'NONE', #12367, #14559, #16588, .T. ) ;
#9473 = FACE_BOUND ( 'NONE', #26107, .T. ) ;
#9474 = AXIS2_PLACEMENT_3D ( 'NONE', #13461, #6460, #25230 ) ;
#9475 = ORIENTED_EDGE ( 'NONE', *, *, #29614, .T. ) ;
#9476 = PLANE ( 'NONE',  #7688 ) ;
#9477 = DIRECTION ( 'NONE',  ( -0.5877852522924731371, -1.586114251531760728E-16, -0.8090169943749474513 ) ) ;
#9478 = FACE_OUTER_BOUND ( 'NONE', #17350, .T. ) ;
#9479 = CARTESIAN_POINT ( 'NONE',  ( 10.73702987185851931, 16.55672395529124330, -15.94748436097269817 ) ) ;
#9480 = CARTESIAN_POINT ( 'NONE',  ( 141.1922820468854525, -1.999999999999978684, -13.59645775552055902 ) ) ;
#9481 = ORIENTED_EDGE ( 'NONE', *, *, #12330, .F. ) ;
#9482 = LINE ( 'NONE', #4767, #16888 ) ;
#9483 = ORIENTED_EDGE ( 'NONE', *, *, #21561, .T. ) ;
#9484 = CARTESIAN_POINT ( 'NONE',  ( 11.34314632229486364, 9.864239995495806212, -15.91456019135469013 ) ) ;
#9485 = ORIENTED_EDGE ( 'NONE', *, *, #12140, .F. ) ;
#9486 = CARTESIAN_POINT ( 'NONE',  ( 19.07048665705943336, 2.338351316274200453, -13.70053041002553407 ) ) ;
#9487 = LINE ( 'NONE', #4480, #29319 ) ;
#9488 = CARTESIAN_POINT ( 'NONE',  ( 168.6922820468852819, -9.999999999999998224, -0.6060766987539614181 ) ) ;
#9489 = CARTESIAN_POINT ( 'NONE',  ( 26.47511176763426377, -7.718147522161595830, -18.64721581247919602 ) ) ;
#9490 = CARTESIAN_POINT ( 'NONE',  ( 133.7287565553229456, -1.999999999999980904, 6.499999999999978684 ) ) ;
#9491 = CARTESIAN_POINT ( 'NONE',  ( 11.08268301555968094, 17.56437024738003316, -17.37355016474266733 ) ) ;
#9492 = ORIENTED_EDGE ( 'NONE', *, *, #19270, .T. ) ;
#9493 = CARTESIAN_POINT ( 'NONE',  ( 35.37054299657279444, -20.38462739797860479, -19.24905200684423789 ) ) ;
#9494 = CARTESIAN_POINT ( 'NONE',  ( 17.32873655921053313, 10.26331207550778579, -16.20725374984683143 ) ) ;
#9495 = ORIENTED_EDGE ( 'NONE', *, *, #28451, .F. ) ;
#9496 = VECTOR ( 'NONE', #19101, 1000.000000000000000 ) ;
#9497 = FACE_OUTER_BOUND ( 'NONE', #4644, .T. ) ;
#9498 = CARTESIAN_POINT ( 'NONE',  ( 27.61464345320196045, -4.235915813641956795, -14.29244051139929894 ) ) ;
#9499 = ORIENTED_EDGE ( 'NONE', *, *, #10958, .T. ) ;
#9500 = DIRECTION ( 'NONE',  ( -0.5877852522924731371, -1.586114251531760235E-16, 0.8090169943749474513 ) ) ;
#9501 = CARTESIAN_POINT ( 'NONE',  ( 21.26575470983302196, 3.903880982571942493, -18.68858533207590966 ) ) ;
#9502 = CARTESIAN_POINT ( 'NONE',  ( 15.09270446591840731, 5.883488971450414162, -17.42782692652931331 ) ) ;
#9503 = VERTEX_POINT ( 'NONE', #3024 ) ;
#9504 = ORIENTED_EDGE ( 'NONE', *, *, #23247, .F. ) ;
#9505 = EDGE_CURVE ( 'NONE', #5460, #7125, #14135, .T. ) ;
#9506 = CARTESIAN_POINT ( 'NONE',  ( 162.0152310637604955, -1.999999999999972689, -15.61832212156129707 ) ) ;
#9507 = ADVANCED_FACE ( 'NONE', ( #25912, #18874 ), #28232, .T. ) ;
#9508 = LINE ( 'NONE', #14387, #3598 ) ;
#9509 = PLANE ( 'NONE',  #28116 ) ;
#9510 = CARTESIAN_POINT ( 'NONE',  ( 157.2287565553229740, -1.999999999999973577, -20.83012701892220520 ) ) ;
#9511 = CIRCLE ( 'NONE', #26131, 0.2500000000000002220 ) ;
#9512 = LINE ( 'NONE', #16395, #12373 ) ;
#9513 = ORIENTED_EDGE ( 'NONE', *, *, #446, .T. ) ;
#9514 = AXIS2_PLACEMENT_3D ( 'NONE', #8334, #19931, #6050 ) ;
#9515 = CARTESIAN_POINT ( 'NONE',  ( 9.655099948573186097, 17.60583584124798051, -17.48406748397995614 ) ) ;
#9516 = CARTESIAN_POINT ( 'NONE',  ( 22.71651454236177514, -3.376241010138071541, -20.62701743264632270 ) ) ;
#9517 = CARTESIAN_POINT ( 'NONE',  ( 21.59786356094703308, -0.7637721020719707710, -13.97513905925265298 ) ) ;
#9519 = ORIENTED_EDGE ( 'NONE', *, *, #28738, .F. ) ;
#9518 = CARTESIAN_POINT ( 'NONE',  ( 33.18306031693006730, -12.55741664378837896, -20.68523176094931415 ) ) ;
#9520 = CARTESIAN_POINT ( 'NONE',  ( 137.0152310637605808, -10.00000000000000533, -34.70218595412750773 ) ) ;
#9521 = DIRECTION ( 'NONE',  ( 1.000000000000000000, 4.440892098500622217E-16, 0.000000000000000000 ) ) ;
#9522 = LINE ( 'NONE', #22989, #29869 ) ;
#9523 = LINE ( 'NONE', #16404, #24652 ) ;
#9524 = CARTESIAN_POINT ( 'NONE',  ( 19.51440197245297270, 8.071880087464508691, -17.28625796899888201 ) ) ;
#9525 = ORIENTED_EDGE ( 'NONE', *, *, #8038, .F. ) ;
#9526 = CARTESIAN_POINT ( 'NONE',  ( 172.7287565553229456, -3.999999999999989786, 8.500000000000007105 ) ) ;
#9527 = CARTESIAN_POINT ( 'NONE',  ( 10.71981169803933120, 16.63568869523268390, -15.95461020916288675 ) ) ;
#9528 = VECTOR ( 'NONE', #4514, 1000.000000000000000 ) ;
#9529 = ORIENTED_EDGE ( 'NONE', *, *, #439, .F. ) ;
#9530 = CARTESIAN_POINT ( 'NONE',  ( 13.06098793629887744, -5.000000000000014211, -40.19758755079165979 ) ) ;
#9531 = LINE ( 'NONE', #9845, #27408 ) ;
#9532 = VECTOR ( 'NONE', #8822, 1000.000000000000000 ) ;
#9533 = CARTESIAN_POINT ( 'NONE',  ( 17.29421355564066332, 9.360779442694735053, -19.18964209290773937 ) ) ;
#9534 = CARTESIAN_POINT ( 'NONE',  ( 29.81560109580191664, -6.784977964013398477, -14.56477501241906403 ) ) ;
#9535 = EDGE_LOOP ( 'NONE', ( #28748, #16427, #174, #20514 ) ) ;
#9536 = CARTESIAN_POINT ( 'NONE',  ( 35.54859390954303677, -23.18451583373416014, -15.55638201429745848 ) ) ;
#9537 = CARTESIAN_POINT ( 'NONE',  ( 22.98313442454129429, 1.505266882216666158, -15.27805348665062546 ) ) ;
#9538 = AXIS2_PLACEMENT_3D ( 'NONE', #7890, #22390, #10783 ) ;
#9539 = CARTESIAN_POINT ( 'NONE',  ( 20.14628369065288993, 2.528829491441240584, -14.55248280469624866 ) ) ;
#9540 = AXIS2_PLACEMENT_3D ( 'NONE', #1858, #6111, #24584 ) ;
#9541 = ORIENTED_EDGE ( 'NONE', *, *, #178, .F. ) ;
#9542 = CARTESIAN_POINT ( 'NONE',  ( 30.15014520769674533, -9.019674524353797906, -15.19912247041013842 ) ) ;
#9543 = ADVANCED_FACE ( 'NONE', ( #5139 ), #5449, .T. ) ;
#9544 = EDGE_CURVE ( 'NONE', #25774, #26592, #2573, .T. ) ;
#9545 = ORIENTED_EDGE ( 'NONE', *, *, #4318, .T. ) ;
#9546 = ADVANCED_FACE ( 'NONE', ( #119 ), #4836, .T. ) ;
#9547 = CARTESIAN_POINT ( 'NONE',  ( 152.0152310637604671, -1.999999999999976241, -0.06116980274991495881 ) ) ;
#9549 = ORIENTED_EDGE ( 'NONE', *, *, #23991, .T. ) ;
#9548 = DIRECTION ( 'NONE',  ( 0.000000000000000000, 0.000000000000000000, 1.000000000000000000 ) ) ;
#9550 = ORIENTED_EDGE ( 'NONE', *, *, #10230, .T. ) ;
#9551 = DIRECTION ( 'NONE',  ( -0.9510565162951536422, -2.566386769018988816E-16, -0.3090169943749472292 ) ) ;
#9552 = AXIS2_PLACEMENT_3D ( 'NONE', #28215, #26499, #5117 ) ;
#9553 = CARTESIAN_POINT ( 'NONE',  ( -4.000000000000003553, -6.938893903907228378E-15, -2.450000000000000178 ) ) ;
#9554 = CARTESIAN_POINT ( 'NONE',  ( 34.55638066306561029, -12.23714146529668234, -18.94394112255963236 ) ) ;
#9555 = AXIS2_PLACEMENT_3D ( 'NONE', #8112, #5387, #5837 ) ;
#9556 = CARTESIAN_POINT ( 'NONE',  ( 9.641350810849047548, 17.66889113945805789, -19.66666666666842644 ) ) ;
#9557 = EDGE_LOOP ( 'NONE', ( #15232, #29224, #11408 ) ) ;
#9558 = AXIS2_PLACEMENT_3D ( 'NONE', #10831, #17695, #2003 ) ;
#9559 = DIRECTION ( 'NONE',  ( -2.698458740408365879E-16, 1.000000000000000000, 0.000000000000000000 ) ) ;
#9560 = DIRECTION ( 'NONE',  ( -0.5877852522924731371, -1.586114251531760728E-16, -0.8090169943749474513 ) ) ;
#9561 = CARTESIAN_POINT ( 'NONE',  ( 10.73134732381016576, 15.26288385841099249, -17.22756371135774245 ) ) ;
#9562 = FACE_OUTER_BOUND ( 'NONE', #19306, .T. ) ;
#9563 = CARTESIAN_POINT ( 'NONE',  ( 142.0152310637605524, -10.00000000000000533, 1.702185954127501066 ) ) ;
#9564 = ORIENTED_EDGE ( 'NONE', *, *, #12629, .F. ) ;
#9565 = CARTESIAN_POINT ( 'NONE',  ( -2.500000000000002665, -1.110223024625156738E-15, -2.424599999999998978 ) ) ;
#9566 = DIRECTION ( 'NONE',  ( -0.000000000000000000, -0.000000000000000000, 1.000000000000000000 ) ) ;
#9567 = ORIENTED_EDGE ( 'NONE', *, *, #23379, .T. ) ;
#9568 = ORIENTED_EDGE ( 'NONE', *, *, #30190, .F. ) ;
#9569 = CARTESIAN_POINT ( 'NONE',  ( 178.7287565553229172, -1.999999999999968914, 0.5000000000000029976 ) ) ;
#9570 = ORIENTED_EDGE ( 'NONE', *, *, #21341, .F. ) ;
#9571 = CARTESIAN_POINT ( 'NONE',  ( 9.662182123323882266, 16.25345509848694547, -17.90638241064055336 ) ) ;
#9572 = EDGE_CURVE ( 'NONE', #3020, #6774, #9862, .T. ) ;
#9573 = CARTESIAN_POINT ( 'NONE',  ( 24.53726495287250486, -4.893489461768670168, -18.28393818840952534 ) ) ;
#9574 = CARTESIAN_POINT ( 'NONE',  ( 26.39122182234759961, -2.132411660323914049, -15.07701415690354274 ) ) ;
#9575 = VECTOR ( 'NONE', #8012, 1000.000000000000000 ) ;
#9576 = LINE ( 'NONE', #28255, #13079 ) ;
#9577 = DIRECTION ( 'NONE',  ( -0.5877852522924731371, -1.586114251531760728E-16, -0.8090169943749474513 ) ) ;
#9578 = DIRECTION ( 'NONE',  ( -1.000000000000000000, 0.000000000000000000, 0.000000000000000000 ) ) ;
#9579 = AXIS2_PLACEMENT_3D ( 'NONE', #12349, #8224, #17092 ) ;
#9580 = CARTESIAN_POINT ( 'NONE',  ( 26.04489551603160180, -6.130266781319400948, -13.71289979607875154 ) ) ;
#9581 = EDGE_CURVE ( 'NONE', #23543, #24609, #11698, .T. ) ;
#9582 = VECTOR ( 'NONE', #24082, 1000.000000000000000 ) ;
#9583 = EDGE_CURVE ( 'NONE', #11816, #930, #26213, .T. ) ;
#9584 = ADVANCED_FACE ( 'NONE', ( #14582 ), #23932, .T. ) ;
#9585 =( NAMED_UNIT ( * ) PLANE_ANGLE_UNIT ( ) SI_UNIT ( $, .RADIAN. ) );
#9586 = EDGE_CURVE ( 'NONE', #27772, #7950, #23613, .T. ) ;
#9587 = PLANE ( 'NONE',  #29928 ) ;
#9588 = VECTOR ( 'NONE', #6605, 1000.000000000000000 ) ;
#9589 = LINE ( 'NONE', #18909, #18460 ) ;
#9590 = DIRECTION ( 'NONE',  ( -0.9510565162951536422, 0.000000000000000000, -0.3090169943749472292 ) ) ;
#9591 = CARTESIAN_POINT ( 'NONE',  ( 129.5152310637605524, -10.00000000000000888, -21.71180489736090991 ) ) ;
#9592 = CARTESIAN_POINT ( 'NONE',  ( 10.47169460192958645, 16.45368433897878191, -17.33494088278173351 ) ) ;
#9593 = CARTESIAN_POINT ( 'NONE',  ( 136.1922820468854241, -10.00000000000000533, -30.91696583120935671 ) ) ;
#9594 = CARTESIAN_POINT ( 'NONE',  ( 34.11209566957792561, -15.73109017586260272, -19.92372960426217787 ) ) ;
#9595 = VERTEX_POINT ( 'NONE', #21157 ) ;
#9596 = CARTESIAN_POINT ( 'NONE',  ( 15.26446397285951839, 8.458903494591371697, -14.20561233965910297 ) ) ;
#9597 = ORIENTED_EDGE ( 'NONE', *, *, #13188, .T. ) ;
#9598 = CARTESIAN_POINT ( 'NONE',  ( 0.000000000000000000, 0.000000000000000000, 0.000000000000000000 ) ) ;
#9599 = COLOUR_RGB ( '', 0.72549020, 0.75294118, 0.79215686) ;
#9600 = CARTESIAN_POINT ( 'NONE',  ( 18.80472905218952917, 2.352968372735388503, -20.19605574946481497 ) ) ;
#9601 = CARTESIAN_POINT ( 'NONE',  ( 11.05552354607739929, 17.68892703645376585, -17.88069451076903249 ) ) ;
#9602 = LINE ( 'NONE', #165, #5353 ) ;
#9603 = EDGE_LOOP ( 'NONE', ( #12610, #22341, #3262, #16109 ) ) ;
#9604 = ORIENTED_EDGE ( 'NONE', *, *, #10025, .T. ) ;
#9605 = ORIENTED_EDGE ( 'NONE', *, *, #6342, .T. ) ;
#9606 = AXIS2_PLACEMENT_3D ( 'NONE', #27283, #11486, #25400 ) ;
#9607 = CARTESIAN_POINT ( 'NONE',  ( 9.644802874473198173, 17.65305953564175567, -17.69767226479352118 ) ) ;
#9608 = DIRECTION ( 'NONE',  ( 1.110223024625156540E-16, 2.995891024602366092E-32, 1.000000000000000000 ) ) ;
#9609 = CARTESIAN_POINT ( 'NONE',  ( 9.879812780108833792, 16.57527415160161510, -16.52987074417163527 ) ) ;
#9610 = LINE ( 'NONE', #25958, #1369 ) ;
#9611 = ORIENTED_EDGE ( 'NONE', *, *, #20200, .T. ) ;
#9612 = DIRECTION ( 'NONE',  ( 1.000000000000000000, 2.698458740408365879E-16, -1.110223024625156540E-16 ) ) ;
#9613 = ORIENTED_EDGE ( 'NONE', *, *, #22916, .F. ) ;
#9614 = CARTESIAN_POINT ( 'NONE',  ( 10.47169460192958645, 16.45368433897878191, -17.33494088278173351 ) ) ;
#9615 = ADVANCED_FACE ( 'NONE', ( #24674 ), #22380, .F. ) ;
#9616 = ORIENTED_EDGE ( 'NONE', *, *, #12212, .T. ) ;
#9617 = CIRCLE ( 'NONE', #13519, 8.000000000000003553 ) ;
#9618 = CARTESIAN_POINT ( 'NONE',  ( 32.82219004228267778, -9.671386367997632405, -18.62901690529166743 ) ) ;
#9619 = CARTESIAN_POINT ( 'NONE',  ( 17.30683543869610119, 10.98570342618945617, -17.92154440881979482 ) ) ;
#9620 = CARTESIAN_POINT ( 'NONE',  ( 27.51942754507220812, -5.605608590038333006, -14.64806962472005658 ) ) ;
#9621 = FACE_OUTER_BOUND ( 'NONE', #19024, .T. ) ;
#9622 = ORIENTED_EDGE ( 'NONE', *, *, #21169, .T. ) ;
#9623 = CARTESIAN_POINT ( 'NONE',  ( 34.52681913409613657, -13.10175273156466069, -19.97882978310374469 ) ) ;
#9624 = CARTESIAN_POINT ( 'NONE',  ( 16.66981565813235733, 9.362922448895053762, -13.87743608138566920 ) ) ;
#9625 = CARTESIAN_POINT ( 'NONE',  ( 27.79246359028025992, -7.761574269410560944, -18.12988733074048753 ) ) ;
#9626 = EDGE_CURVE ( 'NONE', #5247, #29002, #9734, .T. ) ;
#9627 = AXIS2_PLACEMENT_3D ( 'NONE', #6097, #27040, #27353 ) ;
#9628 = EDGE_CURVE ( 'NONE', #27716, #16265, #24520, .T. ) ;
#9630 = ORIENTED_EDGE ( 'NONE', *, *, #5882, .F. ) ;
#9629 = EDGE_CURVE ( 'NONE', #18781, #21937, #8024, .T. ) ;
#9631 = FACE_BOUND ( 'NONE', #21607, .T. ) ;
#9632 = AXIS2_PLACEMENT_3D ( 'NONE', #19867, #14977, #3268 ) ;
#9633 = ORIENTED_EDGE ( 'NONE', *, *, #28618, .F. ) ;
#9634 = FACE_OUTER_BOUND ( 'NONE', #2275, .T. ) ;
#9635 = CARTESIAN_POINT ( 'NONE',  ( 144.7287565553230309, -4.999999999999978684, -16.50000000000000000 ) ) ;
#9636 = LINE ( 'NONE', #18954, #28768 ) ;
#9637 = LINE ( 'NONE', #12078, #13900 ) ;
#9638 = CARTESIAN_POINT ( 'NONE',  ( 10.71678736308702362, 16.64955868083699997, -15.95594379117117434 ) ) ;
#9639 = DIRECTION ( 'NONE',  ( -2.698458740408365879E-16, 1.000000000000000000, 0.000000000000000000 ) ) ;
#9640 = DIRECTION ( 'NONE',  ( -0.000000000000000000, -0.000000000000000000, 1.000000000000000000 ) ) ;
#9641 = VERTEX_POINT ( 'NONE', #5598 ) ;
#9642 = CARTESIAN_POINT ( 'NONE',  ( 9.915538251416846194, 16.41143258624473233, -16.50493629029764264 ) ) ;
#9643 = ORIENTED_EDGE ( 'NONE', *, *, #6407, .T. ) ;
#9644 = CARTESIAN_POINT ( 'NONE',  ( 9.667620158929956631, 16.22851557400931455, -17.88520075955172572 ) ) ;
#9645 = CARTESIAN_POINT ( 'NONE',  ( 23.16986854814090080, 3.028408164773654931, -18.83379972368585342 ) ) ;
#9646 = LINE ( 'NONE', #9032, #10742 ) ;
#9647 = DIRECTION ( 'NONE',  ( -0.000000000000000000, -0.000000000000000000, -1.000000000000000000 ) ) ;
#9648 = CARTESIAN_POINT ( 'NONE',  ( 27.51942754507220812, -5.605608590038333006, -14.64806962472005658 ) ) ;
#9649 = ORIENTED_EDGE ( 'NONE', *, *, #22874, .F. ) ;
#9650 = LINE ( 'NONE', #23707, #2295 ) ;
#9651 = CARTESIAN_POINT ( 'NONE',  ( 11.05541573950045375, 17.68942145115775944, -17.91357985325011626 ) ) ;
#9652 = ORIENTED_EDGE ( 'NONE', *, *, #16870, .T. ) ;
#9653 = AXIS2_PLACEMENT_3D ( 'NONE', #2892, #26085, #9121 ) ;
#9654 = CARTESIAN_POINT ( 'NONE',  ( 33.60099431436507444, -12.44312249125652414, -18.72218098825057098 ) ) ;
#9655 = CARTESIAN_POINT ( 'NONE',  ( 16.75072914628186282, 8.771658487634226731, -19.67538163746542779 ) ) ;
#9656 = PLANE ( 'NONE',  #3792 ) ;
#9657 = CARTESIAN_POINT ( 'NONE',  ( 9.114604345319493817, 16.17186091871610287, -17.05386699646955861 ) ) ;
#9658 = CARTESIAN_POINT ( 'NONE',  ( 31.00997733146710900, -7.209757123251725019, -15.04105334301871011 ) ) ;
#9659 = ORIENTED_EDGE ( 'NONE', *, *, #10939, .F. ) ;
#9660 = DIRECTION ( 'NONE',  ( 0.000000000000000000, -1.000000000000000000, 0.000000000000000000 ) ) ;
#9661 = FILL_AREA_STYLE ('',( #25705 ) ) ;
#9662 = CARTESIAN_POINT ( 'NONE',  ( 20.01918758985507196, 7.682949113293006782, -15.97060347488303123 ) ) ;
#9663 = CARTESIAN_POINT ( 'NONE',  ( 16.64656040655037827, 6.484405094197702724, -15.29036880746224014 ) ) ;
#9664 = VERTEX_POINT ( 'NONE', #12905 ) ;
#9666 = ORIENTED_EDGE ( 'NONE', *, *, #26787, .T. ) ;
#9665 = EDGE_CURVE ( 'NONE', #3010, #28897, #19929, .T. ) ;
#9667 = DIRECTION ( 'NONE',  ( -0.8090169943749474513, -2.183098979609982436E-16, 0.5877852522924731371 ) ) ;
#9668 = CARTESIAN_POINT ( 'NONE',  ( 159.7287565553229456, -10.00000000000000000, -16.50000000000000355 ) ) ;
#9669 = CARTESIAN_POINT ( 'NONE',  ( 3.441479889454326813, -5.000000000000016875, 10.59178599929328435 ) ) ;
#9670 = VECTOR ( 'NONE', #19431, 1000.000000000000000 ) ;
#9671 = DIRECTION ( 'NONE',  ( 1.110223024625156540E-16, 2.995891024602366092E-32, 1.000000000000000000 ) ) ;
#9672 = DIRECTION ( 'NONE',  ( 0.000000000000000000, 0.000000000000000000, -1.000000000000000000 ) ) ;
#9673 = CARTESIAN_POINT ( 'NONE',  ( 9.641359250860388030, 17.66885243249017634, -17.90483003768722625 ) ) ;
#9674 = CARTESIAN_POINT ( 'NONE',  ( 28.95742876386502118, -9.428754790923060014, -17.52548735455339823 ) ) ;
#9675 = CARTESIAN_POINT ( 'NONE',  ( 24.52508672555368463, -0.3756359333432500169, -18.08805785897195051 ) ) ;
#9676 = CARTESIAN_POINT ( 'NONE',  ( 32.52689891806821265, -10.77327725507678302, -19.81022979934233064 ) ) ;
#9677 = VECTOR ( 'NONE', #25418, 1000.000000000000000 ) ;
#9678 = CARTESIAN_POINT ( 'NONE',  ( 12.50268541164654756, 8.571888915454989544, -15.12803469218787811 ) ) ;
#9679 = LINE ( 'NONE', #5112, #12741 ) ;
#9680 = CARTESIAN_POINT ( 'NONE',  ( 2.000000000000026201, 3.464101615137736623, -2.450000000000000622 ) ) ;
#9681 = CARTESIAN_POINT ( 'NONE',  ( 15.14574614762244487, 6.587483969391940697, -15.14885142785537830 ) ) ;
#9682 = FACE_OUTER_BOUND ( 'NONE', #26728, .T. ) ;
#9683 = CARTESIAN_POINT ( 'NONE',  ( 10.72001338896670397, 16.63476371493014128, -15.95452473000899118 ) ) ;
#9684 = EDGE_CURVE ( 'NONE', #8715, #15699, #12753, .T. ) ;
#9685 = DIRECTION ( 'NONE',  ( 1.110223024625156540E-16, 2.995891024602366092E-32, 1.000000000000000000 ) ) ;
#9686 = DIRECTION ( 'NONE',  ( 0.000000000000000000, 0.000000000000000000, 1.000000000000000000 ) ) ;
#9687 = PRODUCT_RELATED_PRODUCT_CATEGORY ( 'part', '', ( #8864 ) ) ;
#9688 = CARTESIAN_POINT ( 'NONE',  ( 17.12833724908345800, 9.171387755021909172, -19.38714867094073213 ) ) ;
#9689 = ORIENTED_EDGE ( 'NONE', *, *, #11078, .F. ) ;
#9690 = CARTESIAN_POINT ( 'NONE',  ( 15.78898853071975061, 11.08777142890889245, -14.37707943039971781 ) ) ;
#9691 = ORIENTED_EDGE ( 'NONE', *, *, #17850, .T. ) ;
#9692 = CARTESIAN_POINT ( 'NONE',  ( 32.63711423693117553, -11.05166607373017484, -18.34576405707344549 ) ) ;
#9693 = VECTOR ( 'NONE', #28456, 1000.000000000000000 ) ;
#9694 = CARTESIAN_POINT ( 'NONE',  ( 20.77099883799555258, -1.523348603316126981, -18.27480029096593839 ) ) ;
#9695 = CARTESIAN_POINT ( 'NONE',  ( 18.95088517700565944, -0.6660330538943091128, -18.51770762617101340 ) ) ;
#9696 = AXIS2_PLACEMENT_3D ( 'NONE', #16460, #7609, #4867 ) ;
#9697 = CARTESIAN_POINT ( 'NONE',  ( 30.28771073495105881, -9.259452824753982014, -16.33981616121770131 ) ) ;
#9698 = ORIENTED_EDGE ( 'NONE', *, *, #16448, .F. ) ;
#9699 = FACE_OUTER_BOUND ( 'NONE', #23943, .T. ) ;
#9700 = ORIENTED_EDGE ( 'NONE', *, *, #3782, .T. ) ;
#9701 = CARTESIAN_POINT ( 'NONE',  ( 0.000000000000000000, 0.000000000000000000, 0.000000000000000000 ) ) ;
#9702 = CARTESIAN_POINT ( 'NONE',  ( 144.7287565553229740, -10.00000000000000533, 0.8205080756887930260 ) ) ;
#9703 = CARTESIAN_POINT ( 'NONE',  ( -4.000000000000005329, 1.935983797701083420, -2.200530693383765168 ) ) ;
#9704 = CARTESIAN_POINT ( 'NONE',  ( 34.71713976128472723, -12.95676249388076329, -18.99403759477717557 ) ) ;
#9705 = VECTOR ( 'NONE', #16781, 1000.000000000000000 ) ;
#9706 = CARTESIAN_POINT ( 'NONE',  ( 9.641404825192898542, 17.66864342279195199, -17.88841768828662282 ) ) ;
#9707 = VERTEX_POINT ( 'NONE', #17486 ) ;
#9708 = CARTESIAN_POINT ( 'NONE',  ( 142.2287565553230024, -1.999999999999978462, -3.509618943233403510 ) ) ;
#9709 = FACE_OUTER_BOUND ( 'NONE', #16105, .T. ) ;
#9710 = CARTESIAN_POINT ( 'NONE',  ( 12.02841764901576838, 9.314357472305010432, -16.69117924060192948 ) ) ;
#9711 = CARTESIAN_POINT ( 'NONE',  ( 171.1922820468853388, -9.999999999999996447, -19.40354224447947828 ) ) ;
#9712 = VECTOR ( 'NONE', #18423, 1000.000000000000000 ) ;
#9713 = CARTESIAN_POINT ( 'NONE',  ( 152.2287565553230024, -4.999999999999976907, -20.83012701892220164 ) ) ;
#9714 = EDGE_CURVE ( 'NONE', #10404, #28006, #29295, .T. ) ;
#9715 = EDGE_CURVE ( 'NONE', #20837, #6555, #7883, .T. ) ;
#9716 = ORIENTED_EDGE ( 'NONE', *, *, #13141, .T. ) ;
#9717 = LINE ( 'NONE', #24084, #11975 ) ;
#9718 = EDGE_CURVE ( 'NONE', #379, #26545, #29231, .T. ) ;
#9719 = DIRECTION ( 'NONE',  ( -0.000000000000000000, -0.000000000000000000, -1.000000000000000000 ) ) ;
#9720 = VERTEX_POINT ( 'NONE', #10160 ) ;
#9721 = EDGE_CURVE ( 'NONE', #9725, #2878, #15188, .T. ) ;
#9722 = DIRECTION ( 'NONE',  ( 1.000000000000000000, 4.440892098500622217E-16, 0.000000000000000000 ) ) ;
#9723 = ORIENTED_EDGE ( 'NONE', *, *, #28623, .T. ) ;
#9724 = CARTESIAN_POINT ( 'NONE',  ( 11.22146363488324283, 9.102391324313689580, -17.24260967991309101 ) ) ;
#9725 = VERTEX_POINT ( 'NONE', #29460 ) ;
#9726 = CARTESIAN_POINT ( 'NONE',  ( 23.91915341143258544, -8.806945430038833678, -17.38103690300000181 ) ) ;
#9727 = CARTESIAN_POINT ( 'NONE',  ( 22.45293885382703536, -0.3771200753331621081, -14.01028023225368635 ) ) ;
#9728 = LINE ( 'NONE', #7459, #415 ) ;
#9729 = CARTESIAN_POINT ( 'NONE',  ( 20.00000000000017053, 34.64101615137744972, 12.00000000000000178 ) ) ;
#9731 = CARTESIAN_POINT ( 'NONE',  ( 172.7287565553229740, -84.33034373659253902, -41.50000000000000711 ) ) ;
#9730 = AXIS2_PLACEMENT_3D ( 'NONE', #35, #21224, #25515 ) ;
#9732 = VECTOR ( 'NONE', #5913, 1000.000000000000000 ) ;
#9733 = CARTESIAN_POINT ( 'NONE',  ( 26.80628776457338347, -3.176708023846821494, -16.02594779711905559 ) ) ;
#9734 = CIRCLE ( 'NONE', #22414, 4.000000000000000000 ) ;
#9735 = VECTOR ( 'NONE', #14726, 1000.000000000000000 ) ;
#9736 = CARTESIAN_POINT ( 'NONE',  ( 138.6922820468854241, -4.999999999999979572, 2.247092850131519715 ) ) ;
#9737 = CARTESIAN_POINT ( 'NONE',  ( -20.00000000000017053, 34.64101615137744972, 9.999999999999998224 ) ) ;
#9738 = CARTESIAN_POINT ( 'NONE',  ( 133.7287565553229456, -4.999999999999981348, 0.5000000000000029976 ) ) ;
#9739 = CARTESIAN_POINT ( 'NONE',  ( 2.928571428571432378, 1.300546971703755312E-15, 2.549999999999998490 ) ) ;
#9740 = FACE_OUTER_BOUND ( 'NONE', #14187, .T. ) ;
#9741 = CONICAL_SURFACE ( 'NONE', #28387, 4.175000000000003375, 0.9599310885968852514 ) ;
#9742 = CARTESIAN_POINT ( 'NONE',  ( 11.94706930840425407, 9.687427868553587729, -16.72481990518296158 ) ) ;
#9743 = LINE ( 'NONE', #9593, #19923 ) ;
#9744 = CARTESIAN_POINT ( 'NONE',  ( 35.02155038278115740, -19.81678845073966500, -20.19863594638463411 ) ) ;
#9745 = ORIENTED_EDGE ( 'NONE', *, *, #8869, .F. ) ;
#9746 = AXIS2_PLACEMENT_3D ( 'NONE', #30022, #23099, #11927 ) ;
#9747 = CARTESIAN_POINT ( 'NONE',  ( 16.49632153860815720, 9.003283391651189405, -13.22380011606493788 ) ) ;
#9748 = ORIENTED_EDGE ( 'NONE', *, *, #20237, .F. ) ;
#9749 = DIRECTION ( 'NONE',  ( -2.698458740408365879E-16, 1.000000000000000000, 0.000000000000000000 ) ) ;
#9750 = CARTESIAN_POINT ( 'NONE',  ( 21.58242789233717573, 5.264303332692052528, -18.32037006577847293 ) ) ;
#9751 = CARTESIAN_POINT ( 'NONE',  ( 12.84980237226573863, 9.516412629723424388, -16.12948954962132575 ) ) ;
#9752 = LINE ( 'NONE', #18923, #25830 ) ;
#9753 = EDGE_LOOP ( 'NONE', ( #9936, #10521, #866, #13465 ) ) ;
#9754 = EDGE_CURVE ( 'NONE', #29043, #4557, #16346, .T. ) ;
#9755 = EDGE_LOOP ( 'NONE', ( #20413, #14237, #6797, #12350 ) ) ;
#9756 = CARTESIAN_POINT ( 'NONE',  ( 11.43229926783177497, 9.455373222906182207, -15.87769231223556332 ) ) ;
#9757 = CARTESIAN_POINT ( 'NONE',  ( 424.0000000000002274, 34.64101615137744972, 14.00000000000000178 ) ) ;
#9758 = EDGE_CURVE ( 'NONE', #18859, #27873, #18046, .T. ) ;
#9759 = CARTESIAN_POINT ( 'NONE',  ( 9.826288910175632552, 16.82074144182198694, -16.60662094963572244 ) ) ;
#9760 = CARTESIAN_POINT ( 'NONE',  ( 154.5152310637605240, -1.999999999999974465, -21.71180489736091346 ) ) ;
#9761 = EDGE_CURVE ( 'NONE', #4670, #7383, #29875, .T. ) ;
#9762 = ORIENTED_EDGE ( 'NONE', *, *, #1346, .T. ) ;
#9763 = ORIENTED_EDGE ( 'NONE', *, *, #29324, .T. ) ;
#9764 = PLANE ( 'NONE',  #18852 ) ;
#9765 = VERTEX_POINT ( 'NONE', #30014 ) ;
#9766 = CARTESIAN_POINT ( 'NONE',  ( 10.47079889355419446, 16.45779217176459852, -17.33533584583738829 ) ) ;
#9767 = ORIENTED_EDGE ( 'NONE', *, *, #23378, .F. ) ;
#9768 = CARTESIAN_POINT ( 'NONE',  ( 36.35800453371076202, -21.32829872614925648, -20.07395605779921155 ) ) ;
#9769 = CARTESIAN_POINT ( 'NONE',  ( 26.57062215293289498, -11.41726559881178638, -18.09730928560479057 ) ) ;
#9770 = CARTESIAN_POINT ( 'NONE',  ( 29.22485947447185595, -8.910266539455653501, -18.36689805200119707 ) ) ;
#9771 = ORIENTED_EDGE ( 'NONE', *, *, #21304, .F. ) ;
#9772 = FACE_OUTER_BOUND ( 'NONE', #26090, .T. ) ;
#9773 = PLANE ( 'NONE',  #22534 ) ;
#9774 = VECTOR ( 'NONE', #17943, 1000.000000000000000 ) ;
#9775 = APPLICATION_PROTOCOL_DEFINITION ( 'draft international standard', 'automotive_design', 1998, #27655 ) ;
#9776 = PRESENTATION_LAYER_ASSIGNMENT (  '', '', ( #3455 ) ) ;
#9777 = CARTESIAN_POINT ( 'NONE',  ( 31.69910715399011636, -11.01187737159756352, -14.44698884073069145 ) ) ;
#9778 = AXIS2_PLACEMENT_3D ( 'NONE', #24910, #4144, #13438 ) ;
#9779 = CARTESIAN_POINT ( 'NONE',  ( 28.09155340820903390, -11.11649160481613130, -13.74484337247343824 ) ) ;
#9780 = VERTEX_POINT ( 'NONE', #27412 ) ;
#9781 = LINE ( 'NONE', #25669, #12304 ) ;
#9782 = FACE_OUTER_BOUND ( 'NONE', #27241, .T. ) ;
#9783 = LINE ( 'NONE', #26136, #10118 ) ;
#9784 = DIRECTION ( 'NONE',  ( -0.8191520442889924647, -3.637765840953617664E-16, -0.5735764363510452712 ) ) ;
#9785 = CARTESIAN_POINT ( 'NONE',  ( 156.1922820468853956, -1.999999999999974021, -19.40354224447947828 ) ) ;
#9786 = CARTESIAN_POINT ( 'NONE',  ( 12.27688791398868950, 9.494734666090453246, -15.31069919958039804 ) ) ;
#9788 = AXIS2_PLACEMENT_3D ( 'NONE', #12451, #21777, #877 ) ;
#9787 = DIRECTION ( 'NONE',  ( 0.5877852522924731371, 0.000000000000000000, 0.8090169943749474513 ) ) ;
#9789 = ORIENTED_EDGE ( 'NONE', *, *, #14273, .F. ) ;
#9790 = CARTESIAN_POINT ( 'NONE',  ( 133.7287565553229172, -4.999999999999981348, -33.50000000000000000 ) ) ;
#9791 = ORIENTED_EDGE ( 'NONE', *, *, #10903, .T. ) ;
#9792 = VECTOR ( 'NONE', #27465, 1000.000000000000000 ) ;
#9793 = CARTESIAN_POINT ( 'NONE',  ( 9.920751600319857033, 16.38752350362809551, -16.50277044458016107 ) ) ;
#9794 = EDGE_LOOP ( 'NONE', ( #27437, #550, #22712, #4411 ) ) ;
#9795 = EDGE_CURVE ( 'NONE', #14810, #4331, #25080, .T. ) ;
#9796 = EDGE_CURVE ( 'NONE', #2176, #26572, #23093, .T. ) ;
#9797 = CARTESIAN_POINT ( 'NONE',  ( 19.77208840006000656, -0.3814412559078061982, -20.24210485642555568 ) ) ;
#9798 = FACE_OUTER_BOUND ( 'NONE', #13152, .T. ) ;
#9799 = LINE ( 'NONE', #28469, #30156 ) ;
#9800 = EDGE_CURVE ( 'NONE', #12966, #3391, #6762, .T. ) ;
#9801 = PLANE ( 'NONE',  #3441 ) ;
#9802 = ORIENTED_EDGE ( 'NONE', *, *, #15030, .F. ) ;
#9803 = DIRECTION ( 'NONE',  ( -0.9510565162951536422, -2.566386769018988816E-16, -0.3090169943749472292 ) ) ;
#9804 = EDGE_CURVE ( 'NONE', #20489, #6766, #15904, .T. ) ;
#9805 = CARTESIAN_POINT ( 'NONE',  ( 11.28016675873817576, 16.65868462784220227, -16.78288126510920719 ) ) ;
#9806 = ORIENTED_EDGE ( 'NONE', *, *, #29253, .T. ) ;
#9807 = CARTESIAN_POINT ( 'NONE',  ( 35.36378496564391583, -20.35426714484339783, -19.25178739305277631 ) ) ;
#9808 = CARTESIAN_POINT ( 'NONE',  ( 17.33713706444265412, 0.9871066061555996418, -18.79342181739402307 ) ) ;
#9809 = LINE ( 'NONE', #19121, #17875 ) ;
#9810 = CARTESIAN_POINT ( 'NONE',  ( 9.112400085652602399, 16.18196993452624355, -17.05477891849903926 ) ) ;
#9811 = CARTESIAN_POINT ( 'NONE',  ( 27.13218800474287207, -6.260320175479137106, -19.66075965151719984 ) ) ;
#9812 = ORIENTED_EDGE ( 'NONE', *, *, #18337, .T. ) ;
#9813 = CARTESIAN_POINT ( 'NONE',  ( 133.6922820468854241, -1.999999999999980904, -23.73366926340167282 ) ) ;
#9814 = SURFACE_STYLE_USAGE ( .BOTH. , #23410 ) ;
#9815 = CARTESIAN_POINT ( 'NONE',  ( 18.72775033408030154, 1.433941090885695768, -19.03071139844121262 ) ) ;
#9816 = CARTESIAN_POINT ( 'NONE',  ( 14.32261721435726542, 8.042684561749755545, -14.95628083625202542 ) ) ;
#9817 = CARTESIAN_POINT ( 'NONE',  ( -19.99999999999999289, 55.00000000000000711, -25.00000000000000000 ) ) ;
#9818 = EDGE_LOOP ( 'NONE', ( #27619, #11108, #26658, #9475, #19560 ) ) ;
#9819 = ORIENTED_EDGE ( 'NONE', *, *, #28806, .F. ) ;
#9820 = LINE ( 'NONE', #228, #16081 ) ;
#9821 = AXIS2_PLACEMENT_3D ( 'NONE', #15907, #10880, #13468 ) ;
#9822 = DIRECTION ( 'NONE',  ( -0.7172983783020616677, 0.6967661275386687336, 0.000000000000000000 ) ) ;
#9823 = CARTESIAN_POINT ( 'NONE',  ( 0.6527133886630125392, -8.860760056385789341, -0.4969600502617795290 ) ) ;
#9824 = DIRECTION ( 'NONE',  ( -2.698458740408366372E-16, 1.000000000000000000, 0.000000000000000000 ) ) ;
#9825 = LINE ( 'NONE', #5412, #11912 ) ;
#9826 = ORIENTED_EDGE ( 'NONE', *, *, #5718, .F. ) ;
#9827 = CARTESIAN_POINT ( 'NONE',  ( 9.919231947839115549, 16.39449282361540483, -16.50339887433786501 ) ) ;
#9828 = CARTESIAN_POINT ( 'NONE',  ( 28.11208967899271371, -8.897075463600188527, -14.13618326516971990 ) ) ;
#9829 = CARTESIAN_POINT ( 'NONE',  ( 19.47744964272635926, 1.166342761889149982, -14.46873920536258495 ) ) ;
#9831 = EDGE_LOOP ( 'NONE', ( #8721, #9109, #863, #25083, #17060, #12203 ) ) ;
#9830 = CARTESIAN_POINT ( 'NONE',  ( 33.33926371295168423, -12.28475995124076903, -19.67523791759492013 ) ) ;
#9832 = DIRECTION ( 'NONE',  ( 0.000000000000000000, 0.000000000000000000, -1.000000000000000000 ) ) ;
#9833 = CARTESIAN_POINT ( 'NONE',  ( 130.7287565553229172, -9.999999999999982236, -36.50000000000000711 ) ) ;
#9834 = EDGE_CURVE ( 'NONE', #20421, #29352, #24860, .T. ) ;
#9835 = AXIS2_PLACEMENT_3D ( 'NONE', #11565, #21184, #14458 ) ;
#9836 = DIRECTION ( 'NONE',  ( 0.000000000000000000, 0.000000000000000000, -1.000000000000000000 ) ) ;
#9837 = CARTESIAN_POINT ( 'NONE',  ( 16.64003638268102137, -5.000000000000013323, -51.21276603297467034 ) ) ;
#9838 = EDGE_CURVE ( 'NONE', #10764, #17796, #15458, .T. ) ;
#9839 = CARTESIAN_POINT ( 'NONE',  ( 19.05868480923028940, 8.129737193291200370, -16.02886444249750042 ) ) ;
#9840 = VERTEX_POINT ( 'NONE', #25232 ) ;
#9841 = PLANE ( 'NONE',  #21243 ) ;
#9842 = EDGE_CURVE ( 'NONE', #26897, #4109, #24942, .T. ) ;
#9843 = CARTESIAN_POINT ( 'NONE',  ( 10.33811697311952216, 18.38618935847563307, -17.91478972043705298 ) ) ;
#9844 = CARTESIAN_POINT ( 'NONE',  ( 167.0152310637604387, -1.999999999999971800, -8.721423840594312082 ) ) ;
#9845 = CARTESIAN_POINT ( 'NONE',  ( 138.6922820468854525, -1.999999999999979128, -23.73366926340167282 ) ) ;
#9846 = CARTESIAN_POINT ( 'NONE',  ( 17.54642605795894994, 9.676486402519270058, -18.74681543856335608 ) ) ;
#9847 = CARTESIAN_POINT ( 'NONE',  ( 30.15790919126650138, -6.784097790808209183, -15.35074926656157324 ) ) ;
#9848 = VERTEX_POINT ( 'NONE', #4168 ) ;
#9849 = CARTESIAN_POINT ( 'NONE',  ( 33.10952763335142635, -11.62914684427059697, -19.38687730282833499 ) ) ;
#9850 = CARTESIAN_POINT ( 'NONE',  ( 20.31058213454123162, -2.053861134507735109, -16.68646832148754200 ) ) ;
#9851 = VECTOR ( 'NONE', #6911, 1000.000000000000000 ) ;
#9852 = CARTESIAN_POINT ( 'NONE',  ( 20.55682936838109498, 0.8107970201405315658, -19.60370085144657182 ) ) ;
#9853 = ORIENTED_EDGE ( 'NONE', *, *, #15130, .T. ) ;
#9854 = CARTESIAN_POINT ( 'NONE',  ( 25.61980203353413543, -10.24193911033393256, -18.22380977611897990 ) ) ;
#9855 = AXIS2_PLACEMENT_3D ( 'NONE', #8942, #3940, #6831 ) ;
#9856 = VERTEX_POINT ( 'NONE', #24787 ) ;
#9857 = FACE_OUTER_BOUND ( 'NONE', #29013, .T. ) ;
#9858 = EDGE_CURVE ( 'NONE', #10985, #28338, #13172, .T. ) ;
#9860 = ORIENTED_EDGE ( 'NONE', *, *, #1803, .F. ) ;
#9859 = DIRECTION ( 'NONE',  ( 0.000000000000000000, 1.000000000000000000, 0.000000000000000000 ) ) ;
#9861 = PLANE ( 'NONE',  #18238 ) ;
#9862 = LINE ( 'NONE', #19174, #27833 ) ;
#9863 = CARTESIAN_POINT ( 'NONE',  ( 33.07549275714919901, -10.34104163876563831, -17.35407900654646340 ) ) ;
#9864 = CARTESIAN_POINT ( 'NONE',  ( 12.75704675400704424, 7.626265983139092874, -14.92530421254393147 ) ) ;
#9865 =( REPRESENTATION_RELATIONSHIP ('NONE','NONE', #5250, #24148 ) REPRESENTATION_RELATIONSHIP_WITH_TRANSFORMATION ( #3092 )SHAPE_REPRESENTATION_RELATIONSHIP( ) );
#9866 = CARTESIAN_POINT ( 'NONE',  ( 11.47554319436263448, -5.000000000000014211, 35.31809036943338498 ) ) ;
#9867 = LINE ( 'NONE', #19180, #26092 ) ;
#9868 = CARTESIAN_POINT ( 'NONE',  ( 12.40302661446015264, 8.678734247659738443, -16.45371344743900366 ) ) ;
#9869 = EDGE_CURVE ( 'NONE', #17672, #12245, #1899, .T. ) ;
#9870 = DIRECTION ( 'NONE',  ( -0.5877852522924731371, -1.586114251531760728E-16, -0.8090169943749474513 ) ) ;
#9871 = DIRECTION ( 'NONE',  ( 1.110223024625156540E-16, 2.995891024602366092E-32, 1.000000000000000000 ) ) ;
#9872 = ORIENTED_EDGE ( 'NONE', *, *, #7907, .F. ) ;
#9873 = CARTESIAN_POINT ( 'NONE',  ( -24.99999999999999289, 55.00000000000000711, -25.00000000000000000 ) ) ;
#9874 = CARTESIAN_POINT ( 'NONE',  ( 174.5152310637604387, -4.999999999999970690, -21.71180489736091346 ) ) ;
#9876 = EDGE_LOOP ( 'NONE', ( #3655, #11946, #6708, #17237 ) ) ;
#9875 = VECTOR ( 'NONE', #8051, 1000.000000000000000 ) ;
#9877 = VERTEX_POINT ( 'NONE', #5220 ) ;
#9878 = CARTESIAN_POINT ( 'NONE',  ( 11.20373435594124878, 9.183700057499073921, -17.24994136041982529 ) ) ;
#9879 = CARTESIAN_POINT ( 'NONE',  ( 23.38178567734072999, -4.037937620979102249, -14.56836966348588369 ) ) ;
#9880 = CARTESIAN_POINT ( 'NONE',  ( 24.59824444495380646, -5.013944910511990649, -19.70109713935865514 ) ) ;
#9881 = PLANE ( 'NONE',  #15991 ) ;
#9882 = CARTESIAN_POINT ( 'NONE',  ( 151.1922820468853672, -4.999999999999976907, -2.083034168790677043 ) ) ;
#9883 = LINE ( 'NONE', #19195, #19140 ) ;
#9884 = VECTOR ( 'NONE', #13284, 1000.000000000000000 ) ;
#9885 = ORIENTED_EDGE ( 'NONE', *, *, #21642, .F. ) ;
#9886 = CARTESIAN_POINT ( 'NONE',  ( 143.6922820468854525, -1.999999999999978462, -23.73366926340167282 ) ) ;
#9887 = EDGE_CURVE ( 'NONE', #25944, #19638, #16357, .T. ) ;
#9888 = CARTESIAN_POINT ( 'NONE',  ( 178.7287565553229172, -1.999999999999968914, 0.5000000000000029976 ) ) ;
#9889 = CARTESIAN_POINT ( 'NONE',  ( 131.1922820468854241, -1.999999999999981792, -2.083034168790673490 ) ) ;
#9890 = EDGE_CURVE ( 'NONE', #18400, #29149, #30169, .T. ) ;
#9891 = CARTESIAN_POINT ( 'NONE',  ( 136.1922820468854241, -1.999999999999980460, -30.91696583120935671 ) ) ;
#9892 = LINE ( 'NONE', #1068, #10417 ) ;
#9893 = VECTOR ( 'NONE', #2864, 1000.000000000000000 ) ;
#9894 = CARTESIAN_POINT ( 'NONE',  ( 12.02799090998256304, 9.316311091778235465, -16.69135597610317134 ) ) ;
#9895 = CARTESIAN_POINT ( 'NONE',  ( 88.14846424109262557, -4.999999999999993783, 64.04360804951359398 ) ) ;
#9896 = CARTESIAN_POINT ( 'NONE',  ( 33.40713826534622655, -12.56408340279653757, -19.71064172033093698 ) ) ;
#9897 = VERTEX_POINT ( 'NONE', #14512 ) ;
#9898 = CARTESIAN_POINT ( 'NONE',  ( 8.944584698556434788, 16.95159269123564272, -17.91535980893264224 ) ) ;
#9899 = CARTESIAN_POINT ( 'NONE',  ( 147.0152310637605808, -10.00000000000000178, -15.61832212156129707 ) ) ;
#9900 = CARTESIAN_POINT ( 'NONE',  ( 22.29983652437130814, 0.6627547066652448304, -20.09853802436992964 ) ) ;
#9901 = CARTESIAN_POINT ( 'NONE',  ( 12.86387084073970222, 9.514634738764476296, -16.11888650007813339 ) ) ;
#9902 = DIRECTION ( 'NONE',  ( 2.908569913943825554E-16, -1.000000000000000000, 0.000000000000000000 ) ) ;
#9903 = AXIS2_PLACEMENT_3D ( 'NONE', #8668, #26444, #12525 ) ;
#9904 = VERTEX_POINT ( 'NONE', #28162 ) ;
#9905 = CARTESIAN_POINT ( 'NONE',  ( 11.47231678315799464, 9.271847796573304379, -15.86114366194887815 ) ) ;
#9906 = CARTESIAN_POINT ( 'NONE',  ( 175.7287565553229456, -4.999999999999970690, 0.5000000000000029976 ) ) ;
#9907 = CARTESIAN_POINT ( 'NONE',  ( 9.916118674515717046, 16.40877069192658055, -16.50468880802031890 ) ) ;
#9908 = DIRECTION ( 'NONE',  ( -0.000000000000000000, -0.000000000000000000, 1.000000000000000000 ) ) ;
#9909 = VERTEX_POINT ( 'NONE', #25679 ) ;
#9910 = DIRECTION ( 'NONE',  ( -2.698458740408365879E-16, 1.000000000000000000, 0.000000000000000000 ) ) ;
#9911 = EDGE_LOOP ( 'NONE', ( #21574, #15273, #7775, #25445 ) ) ;
#9912 = CARTESIAN_POINT ( 'NONE',  ( 13.09018272752966716, 8.557097568986355540, -15.93847522207377310 ) ) ;
#9913 = EDGE_LOOP ( 'NONE', ( #27759, #16274, #9187 ) ) ;
#9914 = CARTESIAN_POINT ( 'NONE',  ( 32.57905638361870615, -9.615828745292011703, -17.95267489271534700 ) ) ;
#9915 = CARTESIAN_POINT ( 'NONE',  ( 17.20878921875063838, 11.12208594754616975, -17.23123872766219833 ) ) ;
#9916 = CARTESIAN_POINT ( 'NONE',  ( 29.88803641097454999, -7.968445601786871002, -16.75847372370488131 ) ) ;
#9917 = PLANE ( 'NONE',  #6725 ) ;
#9918 = ORIENTED_EDGE ( 'NONE', *, *, #16869, .F. ) ;
#9919 = VECTOR ( 'NONE', #12112, 1000.000000000000000 ) ;
#9920 = ORIENTED_EDGE ( 'NONE', *, *, #8497, .F. ) ;
#9921 = CARTESIAN_POINT ( 'NONE',  ( 33.54536560287652946, -10.49856191242287373, -18.63199441812703583 ) ) ;
#9922 = SHAPE_DEFINITION_REPRESENTATION ( #26667, #16744 ) ;
#9923 = CARTESIAN_POINT ( 'NONE',  ( 20.37262416712335167, 4.106476634890254829, -18.27772908839511246 ) ) ;
#9924 = CARTESIAN_POINT ( 'NONE',  ( 27.00739300205740889, -11.59555048707680847, -14.72185353022491050 ) ) ;
#9925 = FACE_BOUND ( 'NONE', #27285, .T. ) ;
#9926 = EDGE_CURVE ( 'NONE', #19638, #5499, #12080, .T. ) ;
#9927 = ADVANCED_FACE ( 'NONE', ( #14356 ), #28005, .T. ) ;
#9928 = ADVANCED_FACE ( 'NONE', ( #25989 ), #23541, .T. ) ;
#9929 = CARTESIAN_POINT ( 'NONE',  ( 47.87499999999999289, 0.000000000000000000, 0.000000000000000000 ) ) ;
#9930 = CARTESIAN_POINT ( 'NONE',  ( 134.7287565553230024, -10.00000000000000711, 0.8205080756887930260 ) ) ;
#9931 = FACE_OUTER_BOUND ( 'NONE', #16349, .T. ) ;
#9932 = CARTESIAN_POINT ( 'NONE',  ( 147.0152310637605808, -1.999999999999976685, -15.61832212156129707 ) ) ;
#9933 = AXIS2_PLACEMENT_3D ( 'NONE', #1211, #19203, #6237 ) ;
#9934 = CARTESIAN_POINT ( 'NONE',  ( 12.27567800861033120, 9.500287468128719937, -15.31119923128196625 ) ) ;
#9935 = CARTESIAN_POINT ( 'NONE',  ( -7.345652830558765167, 4.996589667937382018, -0.4964154566688006032 ) ) ;
#9936 = ORIENTED_EDGE ( 'NONE', *, *, #2530, .F. ) ;
#9937 = CARTESIAN_POINT ( 'NONE',  ( 161.1922820468853388, -9.999999999999998224, -13.59645775552055902 ) ) ;
#9938 = VERTEX_POINT ( 'NONE', #16211 ) ;
#9939 = CARTESIAN_POINT ( 'NONE',  ( 11.48249212886396897, 9.228508165798535501, -15.85668214399537845 ) ) ;
#9940 = CARTESIAN_POINT ( 'NONE',  ( 17.37750100583229340, 1.587821987789380440, -15.03969266580305764 ) ) ;
#9941 = DIRECTION ( 'NONE',  ( 1.000000000000000000, 0.000000000000000000, 0.000000000000000000 ) ) ;
#9942 = CARTESIAN_POINT ( 'NONE',  ( 10.00000000000008527, 17.32050807568872486, -17.99999999999999645 ) ) ;
#9943 = DIRECTION ( 'NONE',  ( -0.9510565162951536422, 0.000000000000000000, -0.3090169943749472292 ) ) ;
#9944 = ORIENTED_EDGE ( 'NONE', *, *, #9446, .T. ) ;
#9945 = LINE ( 'NONE', #7384, #19323 ) ;
#9946 = CARTESIAN_POINT ( 'NONE',  ( 12.84002880955021197, 9.524163120117652426, -16.13635871874149430 ) ) ;
#9947 = ORIENTED_EDGE ( 'NONE', *, *, #2314, .T. ) ;
#9948 = CARTESIAN_POINT ( 'NONE',  ( 33.25502826659400313, -11.79853993747392771, -18.08863679259532731 ) ) ;
#9949 = CARTESIAN_POINT ( 'NONE',  ( 14.73401617531889229, 6.408058468588501810, -15.60580005407095960 ) ) ;
#9950 = DIRECTION ( 'NONE',  ( 1.000000000000000000, 2.698458740408365879E-16, -1.110223024625156540E-16 ) ) ;
#9951 = CARTESIAN_POINT ( 'NONE',  ( 22.14981412484149104, -6.473446789742020258, -15.39974742277494713 ) ) ;
#9952 = ORIENTED_EDGE ( 'NONE', *, *, #11724, .T. ) ;
#9953 = DIRECTION ( 'NONE',  ( -0.000000000000000000, -1.000000000000000000, -0.000000000000000000 ) ) ;
#9954 = VERTEX_POINT ( 'NONE', #354 ) ;
#9955 = CARTESIAN_POINT ( 'NONE',  ( 21.84445237452005628, 0.7298858868756038509, -19.18266460542251295 ) ) ;
#9956 = CARTESIAN_POINT ( 'NONE',  ( 17.88967384018823026, 7.017424582044266224, -15.49508032100559696 ) ) ;
#9957 = VECTOR ( 'NONE', #82, 1000.000000000000000 ) ;
#9958 = ORIENTED_EDGE ( 'NONE', *, *, #4537, .T. ) ;
#9959 = DIRECTION ( 'NONE',  ( -0.9510565162951536422, -2.566386769018988816E-16, -0.3090169943749472292 ) ) ;
#9960 = EDGE_LOOP ( 'NONE', ( #8935, #29397, #9144, #1743 ) ) ;
#9961 = ORIENTED_EDGE ( 'NONE', *, *, #6783, .F. ) ;
#9962 = CARTESIAN_POINT ( 'NONE',  ( 139.5152310637605808, -4.999999999999980460, -1.548930218128858680E-14 ) ) ;
#9963 = EDGE_CURVE ( 'NONE', #25406, #17919, #21239, .T. ) ;
#9964 = EDGE_CURVE ( 'NONE', #10203, #10847, #7064, .T. ) ;
#9965 = EDGE_CURVE ( 'NONE', #2774, #3794, #25840, .T. ) ;
#9966 = LINE ( 'NONE', #21723, #2631 ) ;
#9967 = VERTEX_POINT ( 'NONE', #18957 ) ;
#9968 = EDGE_CURVE ( 'NONE', #22275, #25189, #5066, .T. ) ;
#9969 = DIRECTION ( 'NONE',  ( 1.110223024625156540E-16, 2.995891024602366092E-32, 1.000000000000000000 ) ) ;
#9970 = LINE ( 'NONE', #7842, #27762 ) ;
#9971 = PLANE ( 'NONE',  #25561 ) ;
#9972 = CARTESIAN_POINT ( 'NONE',  ( 11.47231678315799464, 9.271847796573304379, -15.86114366194887815 ) ) ;
#9973 = CARTESIAN_POINT ( 'NONE',  ( 27.38292679376507266, -11.43094998702963849, -14.23096243513112036 ) ) ;
#9974 = CARTESIAN_POINT ( 'NONE',  ( 22.83681518364245022, 2.349634567491368564, -16.30468554850739338 ) ) ;
#9976 = ORIENTED_EDGE ( 'NONE', *, *, #6403, .F. ) ;
#9975 = CARTESIAN_POINT ( 'NONE',  ( 34.90271572771163733, -20.28292729397994876, -21.20502438346732887 ) ) ;
#9977 = DIRECTION ( 'NONE',  ( 0.9510565162951535312, 2.566386769018988816E-16, -0.3090169943749475623 ) ) ;
#9978 = CARTESIAN_POINT ( 'NONE',  ( -0.6554360035617876612, 4.240386000424035906, -2.291324518471510974 ) ) ;
#9979 = CARTESIAN_POINT ( 'NONE',  ( 176.1922820468853388, -9.999999999999994671, -30.91696583120936026 ) ) ;
#9980 = VECTOR ( 'NONE', #1439, 1000.000000000000000 ) ;
#9981 = DIRECTION ( 'NONE',  ( 2.908569913943825554E-16, -1.000000000000000000, 0.000000000000000000 ) ) ;
#9982 = CARTESIAN_POINT ( 'NONE',  ( 46.75000000000000000, 0.000000000000000000, 0.000000000000000000 ) ) ;
#9983 = CARTESIAN_POINT ( 'NONE',  ( 23.76365953361780470, 2.837943588559999508, -16.54419024451982168 ) ) ;
#9984 = PLANE ( 'NONE',  #4202 ) ;
#9985 = CARTESIAN_POINT ( 'NONE',  ( 10.72042364955539284, 16.63288220757436164, -15.95435249082810003 ) ) ;
#9986 = FACE_OUTER_BOUND ( 'NONE', #12987, .T. ) ;
#9987 = DIRECTION ( 'NONE',  ( -5.782411586589357392E-17, 0.000000000000000000, -1.000000000000000000 ) ) ;
#9988 = CARTESIAN_POINT ( 'NONE',  ( 18.80472905218952917, 2.352968372735388503, -20.19605574946481497 ) ) ;
#9989 = CARTESIAN_POINT ( 'NONE',  ( 25.85217995398321378, -12.57279400931185620, -13.36530271656463320 ) ) ;
#9990 = ORIENTED_EDGE ( 'NONE', *, *, #29711, .T. ) ;
#9991 = CARTESIAN_POINT ( 'NONE',  ( 34.96805304670973413, -19.57645325810014114, -20.18246498508359466 ) ) ;
#9992 = ORIENTED_EDGE ( 'NONE', *, *, #27256, .T. ) ;
#9993 = CARTESIAN_POINT ( 'NONE',  ( 26.79503139269368006, -8.611318205148688065, -11.94858980718629304 ) ) ;
#9994 = CARTESIAN_POINT ( 'NONE',  ( 17.84334503882807255, 1.539790780908459000, -16.51430848555953190 ) ) ;
#9995 = ORIENTED_EDGE ( 'NONE', *, *, #6785, .T. ) ;
#9996 = ADVANCED_FACE ( 'NONE', ( #28312 ), #23236, .T. ) ;
#9997 = CIRCLE ( 'NONE', #11456, 2.000000000000000000 ) ;
#9998 = EDGE_CURVE ( 'NONE', #14637, #2694, #28460, .T. ) ;
#9999 = DIRECTION ( 'NONE',  ( 0.9510565162951536422, 2.566386769018988816E-16, 0.3090169943749472292 ) ) ;
#10000 = ORIENTED_EDGE ( 'NONE', *, *, #5297, .F. ) ;
#10002 = EDGE_CURVE ( 'NONE', #10566, #21077, #49, .T. ) ;
#10001 = EDGE_LOOP ( 'NONE', ( #5306, #16696, #11411, #5001 ) ) ;
#10004 = ORIENTED_EDGE ( 'NONE', *, *, #29573, .T. ) ;
#10003 =( NAMED_UNIT ( * ) PLANE_ANGLE_UNIT ( ) SI_UNIT ( $, .RADIAN. ) );
#10005 = DIRECTION ( 'NONE',  ( -1.110223024625156540E-16, 0.000000000000000000, -1.000000000000000000 ) ) ;
#10006 = CARTESIAN_POINT ( 'NONE',  ( 157.2287565553229456, -10.00000000000000000, -12.16987298107780369 ) ) ;
#10007 = AXIS2_PLACEMENT_3D ( 'NONE', #16250, #29768, #9070 ) ;
#10008 = CARTESIAN_POINT ( 'NONE',  ( 35.70376052765831787, -18.38912696963886617, -20.33459093173238941 ) ) ;
#10009 = CARTESIAN_POINT ( 'NONE',  ( 9.641350810849047548, 17.66889113945805789, -17.91928203681695564 ) ) ;
#10010 = AXIS2_PLACEMENT_3D ( 'NONE', #11858, #23319, #21172 ) ;
#10011 = DIRECTION ( 'NONE',  ( -2.698458740408365879E-16, 1.000000000000000000, 0.000000000000000000 ) ) ;
#10012 = CARTESIAN_POINT ( 'NONE',  ( 142.0152310637605240, -10.00000000000000533, -0.06116980274991495881 ) ) ;
#10013 = CARTESIAN_POINT ( 'NONE',  ( 13.12174330432777047, 8.570030634161971861, -15.91339823077023929 ) ) ;
#10014 = DIRECTION ( 'NONE',  ( -1.000000000000000000, 0.000000000000000000, -0.000000000000000000 ) ) ;
#10015 = FACE_OUTER_BOUND ( 'NONE', #6695, .T. ) ;
#10016 = EDGE_LOOP ( 'NONE', ( #16225, #12808, #6389, #17265 ) ) ;
#10017 = VECTOR ( 'NONE', #847, 999.9999999999998863 ) ;
#10018 = DIRECTION ( 'NONE',  ( -0.8090169943749474513, -2.183098979609982436E-16, -0.5877852522924731371 ) ) ;
#10019 = CARTESIAN_POINT ( 'NONE',  ( 134.5152310637605524, -1.999999999999980460, -21.71180489736090991 ) ) ;
#10020 = DIRECTION ( 'NONE',  ( -2.698458740408365879E-16, 1.000000000000000000, 0.000000000000000000 ) ) ;
#10021 = ORIENTED_EDGE ( 'NONE', *, *, #15715, .F. ) ;
#10022 = ORIENTED_EDGE ( 'NONE', *, *, #20783, .F. ) ;
#10023 = ORIENTED_EDGE ( 'NONE', *, *, #18692, .T. ) ;
#10024 = CARTESIAN_POINT ( 'NONE',  ( 11.22348983819090407, 9.093098897663914215, -17.24177177356946800 ) ) ;
#10025 = EDGE_CURVE ( 'NONE', #4487, #22117, #18803, .T. ) ;
#10026 = CARTESIAN_POINT ( 'NONE',  ( 23.72538513773186608, -9.146839435613468794, -15.72061189943629600 ) ) ;
#10027 = CARTESIAN_POINT ( 'NONE',  ( 24.00718893345771932, -1.002666751694005765, -18.91818096615087796 ) ) ;
#10028 = PLANE ( 'NONE',  #4319 ) ;
#10029 = LINE ( 'NONE', #28868, #19899 ) ;
#10030 = DIRECTION ( 'NONE',  ( -0.5877852522924731371, -1.586114251531760728E-16, -0.8090169943749474513 ) ) ;
#10031 = VECTOR ( 'NONE', #27115, 1000.000000000000000 ) ;
#10032 = EDGE_LOOP ( 'NONE', ( #9324, #4987, #10551, #1760 ) ) ;
#10033 = PLANE ( 'NONE',  #19633 ) ;
#10034 = EDGE_CURVE ( 'NONE', #18517, #14794, #16667, .T. ) ;
#10035 = LINE ( 'NONE', #24098, #14733 ) ;
#10036 = FACE_OUTER_BOUND ( 'NONE', #9221, .T. ) ;
#10037 = AXIS2_PLACEMENT_3D ( 'NONE', #21701, #5983, #14673 ) ;
#10038 = DIRECTION ( 'NONE',  ( 0.9510565162951535312, 2.566386769018988816E-16, -0.3090169943749475623 ) ) ;
#10040 = CARTESIAN_POINT ( 'NONE',  ( 0.000000000000000000, 0.000000000000000000, -0.5251556536572770106 ) ) ;
#10039 = AXIS2_PLACEMENT_3D ( 'NONE', #26640, #9832, #7850 ) ;
#10041 = CARTESIAN_POINT ( 'NONE',  ( 11.37973238226026318, 12.28930733048782642, -16.95943368139929319 ) ) ;
#10042 = CARTESIAN_POINT ( 'NONE',  ( 164.7287565553228887, -1.999999999999972244, -7.839745962155603820 ) ) ;
#10043 = CARTESIAN_POINT ( 'NONE',  ( 33.60099431436507444, -12.44312249125652414, -18.72218098825057098 ) ) ;
#10044 = ORIENTED_EDGE ( 'NONE', *, *, #29751, .T. ) ;
#10045 = CARTESIAN_POINT ( 'NONE',  ( 13.48814714115247249, 7.673917307032582791, -15.62136820872497545 ) ) ;
#10046 = DIRECTION ( 'NONE',  ( -0.5877852522924731371, -1.586114251531760235E-16, 0.8090169943749474513 ) ) ;
#10047 = CARTESIAN_POINT ( 'NONE',  ( 24.92864811393110358, -0.2441600445015326137, -14.78813717129899885 ) ) ;
#10048 = CARTESIAN_POINT ( 'NONE',  ( 12.84300253770136990, 9.521034635873322216, -16.13432743836305505 ) ) ;
#10049 = FACE_OUTER_BOUND ( 'NONE', #21053, .T. ) ;
#10050 = ORIENTED_EDGE ( 'NONE', *, *, #22493, .T. ) ;
#10051 = ORIENTED_EDGE ( 'NONE', *, *, #5742, .T. ) ;
#10052 = ORIENTED_EDGE ( 'NONE', *, *, #23166, .F. ) ;
#10053 = CARTESIAN_POINT ( 'NONE',  ( 11.47293561586387867, 9.269010148984008879, -15.86088772249501666 ) ) ;
#10054 = CYLINDRICAL_SURFACE ( 'NONE', #23311, 13.00000000000000178 ) ;
#10055 = AXIS2_PLACEMENT_3D ( 'NONE', #26468, #16836, #16987 ) ;
#10056 = CARTESIAN_POINT ( 'NONE',  ( 9.893572868141015775, 16.51216863388285461, -16.51808063826580408 ) ) ;
#10057 = DIRECTION ( 'NONE',  ( -2.698458740408365879E-16, 1.000000000000000000, 0.000000000000000000 ) ) ;
#10058 = ORIENTED_EDGE ( 'NONE', *, *, #29445, .F. ) ;
#10059 = DIRECTION ( 'NONE',  ( -2.698458740408365879E-16, 1.000000000000000000, 0.000000000000000000 ) ) ;
#10060 = ORIENTED_EDGE ( 'NONE', *, *, #2346, .F. ) ;
#10061 = CARTESIAN_POINT ( 'NONE',  ( 12.04525852301462585, 9.245982119944198274, -16.68353927915122981 ) ) ;
#10062 = EDGE_CURVE ( 'NONE', #8000, #7269, #16283, .T. ) ;
#10063 = ORIENTED_EDGE ( 'NONE', *, *, #19345, .T. ) ;
#10065 = CARTESIAN_POINT ( 'NONE',  ( 35.81175537756147520, -19.87429062379433731, -21.40957262365663993 ) ) ;
#10064 = CONICAL_SURFACE ( 'NONE', #1331, 4.175000000000003375, 0.9599310885968852514 ) ;
#10066 = CARTESIAN_POINT ( 'NONE',  ( 24.87127057246125972, -9.548149280147088191, -14.79180087847266556 ) ) ;
#10067 = CARTESIAN_POINT ( 'NONE',  ( 17.15446488409023829, 10.64262399902749578, -18.76211774343175520 ) ) ;
#10068 = VECTOR ( 'NONE', #15856, 1000.000000000000000 ) ;
#10069 = CARTESIAN_POINT ( 'NONE',  ( 172.0152310637604387, -4.999999999999970690, -17.38167787843871182 ) ) ;
#10070 = CARTESIAN_POINT ( 'NONE',  ( 34.35798975979065517, -12.34328324435382207, -19.92780167937219815 ) ) ;
#10071 = CARTESIAN_POINT ( 'NONE',  ( 19.90313213008900206, 2.415960287222779890, -14.54935787103550560 ) ) ;
#10072 = CARTESIAN_POINT ( 'NONE',  ( 14.57776618122778700, 6.338444840345393239, -15.85465340776532095 ) ) ;
#10073 = ORIENTED_EDGE ( 'NONE', *, *, #2310, .T. ) ;
#10074 = CARTESIAN_POINT ( 'NONE',  ( 133.7287565553229172, -1.999999999999980904, -39.49999999999997158 ) ) ;
#10075 = VERTEX_POINT ( 'NONE', #2506 ) ;
#10076 = FACE_BOUND ( 'NONE', #7374, .T. ) ;
#10077 = VECTOR ( 'NONE', #23246, 1000.000000000000000 ) ;
#10078 = LINE ( 'NONE', #23848, #30195 ) ;
#10079 = DIRECTION ( 'NONE',  ( 0.5877852522924731371, 0.000000000000000000, 0.8090169943749474513 ) ) ;
#10080 = LINE ( 'NONE', #789, #14568 ) ;
#10081 = VECTOR ( 'NONE', #9910, 1000.000000000000000 ) ;
#10082 = CARTESIAN_POINT ( 'NONE',  ( -4.000000000000005329, 2.309401076758490934, -2.450000000000000178 ) ) ;
#10083 = CARTESIAN_POINT ( 'NONE',  ( 10.88291651000981730, 15.88766923650820928, -15.88715510423204513 ) ) ;
#10084 = DIRECTION ( 'NONE',  ( 0.000000000000000000, -0.5000000000000011102, -0.8660254037844379305 ) ) ;
#10085 = ORIENTED_EDGE ( 'NONE', *, *, #15928, .T. ) ;
#10086 = LINE ( 'NONE', #28604, #1266 ) ;
#10087 = ORIENTED_EDGE ( 'NONE', *, *, #3483, .T. ) ;
#10088 = CARTESIAN_POINT ( 'NONE',  ( 11.82447321682112751, 8.672047275158794477, -15.63808403058127006 ) ) ;
#10089 = ORIENTED_EDGE ( 'NONE', *, *, #1757, .T. ) ;
#10090 = CARTESIAN_POINT ( 'NONE',  ( 16.47391574482200483, 4.481796633190492152, -18.19319569287263150 ) ) ;
#10091 = CARTESIAN_POINT ( 'NONE',  ( 63.44486372867152824, -29.99999999999998934, -186.4312945166758482 ) ) ;
#10092 = DIRECTION ( 'NONE',  ( 0.000000000000000000, 0.000000000000000000, 1.000000000000000000 ) ) ;
#10093 = CARTESIAN_POINT ( 'NONE',  ( 139.5152310637605808, -1.999999999999979128, -2.627941064794695691 ) ) ;
#10094 = ORIENTED_EDGE ( 'NONE', *, *, #13854, .T. ) ;
#10095 = CARTESIAN_POINT ( 'NONE',  ( 167.2287565553229456, -1.999999999999970912, -20.83012701892220520 ) ) ;
#10096 = VERTEX_POINT ( 'NONE', #16810 ) ;
#10097 = CARTESIAN_POINT ( 'NONE',  ( 11.79482239888288042, 14.29840825880376265, -16.57005305382644877 ) ) ;
#10098 = EDGE_CURVE ( 'NONE', #1963, #25081, #11774, .T. ) ;
#10099 = VERTEX_POINT ( 'NONE', #1250 ) ;
#10100 = EDGE_CURVE ( 'NONE', #6453, #10227, #7812, .T. ) ;
#10101 = CARTESIAN_POINT ( 'NONE',  ( 32.72889690553877529, -10.93821547844579634, -14.37279655741261486 ) ) ;
#10102 = CARTESIAN_POINT ( 'NONE',  ( 21.04385110482095200, 5.766204710259658306, -15.30406332615466347 ) ) ;
#10103 = VERTEX_POINT ( 'NONE', #25020 ) ;
#10104 = EDGE_CURVE ( 'NONE', #28670, #26561, #19550, .T. ) ;
#10105 = VECTOR ( 'NONE', #14728, 1000.000000000000000 ) ;
#10106 = LINE ( 'NONE', #8121, #21333 ) ;
#10107 = ADVANCED_FACE ( 'NONE', ( #3388 ), #24008, .F. ) ;
#10108 = CARTESIAN_POINT ( 'NONE',  ( 16.06097560829885040, 7.604535090956617616, -20.76572858943923094 ) ) ;
#10109 = ORIENTED_EDGE ( 'NONE', *, *, #16518, .T. ) ;
#10110 = DIRECTION ( 'NONE',  ( 0.9510565162951535312, 2.566386769018988816E-16, -0.3090169943749475623 ) ) ;
#10111 = CARTESIAN_POINT ( 'NONE',  ( 21.12965431673027794, -4.223434333162931154, -14.75790768142083031 ) ) ;
#10112 = AXIS2_PLACEMENT_3D ( 'NONE', #16684, #7678, #23406 ) ;
#10113 = CARTESIAN_POINT ( 'NONE',  ( 17.50199379865806293, 2.211901401554522639, -18.92990045904890550 ) ) ;
#10114 = ORIENTED_EDGE ( 'NONE', *, *, #28621, .T. ) ;
#10115 = PLANE ( 'NONE',  #16708 ) ;
#10116 = ORIENTED_EDGE ( 'NONE', *, *, #1075, .F. ) ;
#10117 = DIRECTION ( 'NONE',  ( 0.5877852522924731371, 1.586114251531760728E-16, 0.8090169943749474513 ) ) ;
#10118 = VECTOR ( 'NONE', #29054, 1000.000000000000000 ) ;
#10119 = CARTESIAN_POINT ( 'NONE',  ( 147.0152310637606092, -1.999999999999976241, -24.27857615940569502 ) ) ;
#10120 = CARTESIAN_POINT ( 'NONE',  ( 142.0152310637605808, -4.999999999999979572, -1.576685793744487594E-14 ) ) ;
#10121 = LINE ( 'NONE', #7691, #28244 ) ;
#10122 = CARTESIAN_POINT ( 'NONE',  ( 10.04317065217474436, -5.000000000000015099, 30.90970097723984722 ) ) ;
#10123 = AXIS2_PLACEMENT_3D ( 'NONE', #13210, #27584, #20663 ) ;
#10124 = CARTESIAN_POINT ( 'NONE',  ( 10.56508425215480074, 13.43253182900300402, -16.23631622730588830 ) ) ;
#10125 = CARTESIAN_POINT ( 'NONE',  ( 28.43808809371321189, -7.037065510061861318, -17.41003659457544117 ) ) ;
#10126 = CARTESIAN_POINT ( 'NONE',  ( 26.83671086236671144, -5.482767762337403816, -13.01846673106422436 ) ) ;
#10128 = EDGE_LOOP ( 'NONE', ( #26608, #26061, #16980, #9437 ) ) ;
#10127 = CARTESIAN_POINT ( 'NONE',  ( 35.54859390953724585, -23.18451583373416014, -17.22552805718784441 ) ) ;
#10129 = CARTESIAN_POINT ( 'NONE',  ( 5.200000000000002842, 0.000000000000000000, 0.000000000000000000 ) ) ;
#10130 = AXIS2_PLACEMENT_3D ( 'NONE', #26774, #7972, #15131 ) ;
#10131 = DIRECTION ( 'NONE',  ( -2.698458740408366372E-16, 1.000000000000000000, 0.000000000000000000 ) ) ;
#10132 = CARTESIAN_POINT ( 'NONE',  ( 172.2287565553229172, -1.999999999999969580, -20.83012701892220520 ) ) ;
#10133 = PLANE ( 'NONE',  #24447 ) ;
#10134 = CARTESIAN_POINT ( 'NONE',  ( 0.000000000000000000, 0.000000000000000000, -18.00000000000000000 ) ) ;
#10135 = CARTESIAN_POINT ( 'NONE',  ( 18.88762249820254624, 5.002188274287570735, -13.90571046850145542 ) ) ;
#10136 = ORIENTED_EDGE ( 'NONE', *, *, #23014, .T. ) ;
#10137 = FACE_OUTER_BOUND ( 'NONE', #15974, .T. ) ;
#10138 = CARTESIAN_POINT ( 'NONE',  ( 12.27692691330339514, 9.494559429826583852, -15.31068279593241144 ) ) ;
#10139 = CARTESIAN_POINT ( 'NONE',  ( -16.00000000000017053, 34.64101615137744972, 9.999999999999998224 ) ) ;
#10140 = CARTESIAN_POINT ( 'NONE',  ( 169.7287565553229456, -4.999999999999971578, -16.50000000000000000 ) ) ;
#10141 = EDGE_CURVE ( 'NONE', #15686, #14718, #28919, .T. ) ;
#10142 = CARTESIAN_POINT ( 'NONE',  ( 18.97268594440662426, -2.511067197207834667, -17.06021009607598415 ) ) ;
#10143 = EDGE_CURVE ( 'NONE', #3931, #10985, #8097, .T. ) ;
#10144 = CARTESIAN_POINT ( 'NONE',  ( 18.39217644224905257, 0.04847210594158309072, -18.71474297224575878 ) ) ;
#10145 = ORIENTED_EDGE ( 'NONE', *, *, #308, .F. ) ;
#10146 = CARTESIAN_POINT ( 'NONE',  ( 35.02155038278115740, -19.81678845073966500, -20.19863594638463411 ) ) ;
#10147 = SURFACE_SIDE_STYLE ('',( #5587 ) ) ;
#10148 = CARTESIAN_POINT ( 'NONE',  ( 22.02790516022008660, -6.446180030103099590, -16.19395709203531197 ) ) ;
#10149 = CARTESIAN_POINT ( 'NONE',  ( 19.60537025999656890, 4.505197036469223981, -15.34927506990110047 ) ) ;
#10150 = CONICAL_SURFACE ( 'NONE', #15509, 2.500000000000002665, 0.9599310885968781459 ) ;
#10151 = VECTOR ( 'NONE', #19676, 999.9999999999998863 ) ;
#10152 = ORIENTED_EDGE ( 'NONE', *, *, #12976, .F. ) ;
#10153 = CARTESIAN_POINT ( 'NONE',  ( 176.1922820468853104, -9.999999999999994671, -22.25671179336496053 ) ) ;
#10154 = VECTOR ( 'NONE', #11564, 1000.000000000000000 ) ;
#10155 = VECTOR ( 'NONE', #13212, 1000.000000000000000 ) ;
#10157 = ORIENTED_EDGE ( 'NONE', *, *, #15593, .F. ) ;
#10156 = SURFACE_STYLE_USAGE ( .BOTH. , #869 ) ;
#10158 = DIRECTION ( 'NONE',  ( -2.698458740408365879E-16, 1.000000000000000000, 0.000000000000000000 ) ) ;
#10159 = DIRECTION ( 'NONE',  ( -0.8090169943749474513, -2.183098979609982436E-16, 0.5877852522924731371 ) ) ;
#10160 = CARTESIAN_POINT ( 'NONE',  ( -22.75000000000017053, 34.64101615137744972, -10.00000000000000000 ) ) ;
#10161 = EDGE_CURVE ( 'NONE', #14150, #21061, #5378, .T. ) ;
#10162 = CARTESIAN_POINT ( 'NONE',  ( 36.54222296954648641, -22.15589457513855010, -18.69601260479128513 ) ) ;
#10163 = CARTESIAN_POINT ( 'NONE',  ( 9.870716668364401869, 16.61699007954640805, -16.53972800451630931 ) ) ;
#10164 = CARTESIAN_POINT ( 'NONE',  ( 167.0152310637605240, -4.999999999999972466, -34.70218595412750773 ) ) ;
#10165 = LINE ( 'NONE', #28536, #30044 ) ;
#10166 = CARTESIAN_POINT ( 'NONE',  ( 13.11546866977305825, 8.567317423965196355, -15.91839467484043880 ) ) ;
#10167 = DIRECTION ( 'NONE',  ( 0.9510565162951535312, 2.566386769018988816E-16, -0.3090169943749475623 ) ) ;
#10168 = CARTESIAN_POINT ( 'NONE',  ( 10.28378231829363898, -5.000000000000015099, 31.65022754090628254 ) ) ;
#10169 = ORIENTED_EDGE ( 'NONE', *, *, #4643, .T. ) ;
#10170 = AXIS2_PLACEMENT_3D ( 'NONE', #15004, #6016, #22344 ) ;
#10171 = DIRECTION ( 'NONE',  ( -1.000000000000000000, -0.000000000000000000, -1.387778780781445922E-16 ) ) ;
#10172 = CARTESIAN_POINT ( 'NONE',  ( 172.2287565553228603, -1.999999999999970468, -3.509618943233403510 ) ) ;
#10173 = ADVANCED_FACE ( 'NONE', ( #19697 ), #14661, .T. ) ;
#10174 = ADVANCED_FACE ( 'NONE', ( #22001 ), #10890, .T. ) ;
#10175 = CARTESIAN_POINT ( 'NONE',  ( 101.2386341848420699, -4.999999999999990230, 73.55417321246510198 ) ) ;
#10176 = VERTEX_POINT ( 'NONE', #14960 ) ;
#10177 = ADVANCED_FACE ( 'NONE', ( #26591 ), #21690, .T. ) ;
#10178 = VECTOR ( 'NONE', #16618, 1000.000000000000000 ) ;
#10179 = EDGE_LOOP ( 'NONE', ( #18600, #7004, #12684, #20865 ) ) ;
#10180 = ADVANCED_FACE ( 'NONE', ( #21546 ), #7953, .T. ) ;
#10181 = CARTESIAN_POINT ( 'NONE',  ( 11.22298328736398965, 9.095422004326360721, -17.24198125015536576 ) ) ;
#10182 = VECTOR ( 'NONE', #26776, 1000.000000000000000 ) ;
#10183 = CARTESIAN_POINT ( 'NONE',  ( 17.86674704105132605, 10.80914456302241788, -19.54358591003751755 ) ) ;
#10184 = CARTESIAN_POINT ( 'NONE',  ( 24.52508672555368463, -0.3756359333432500169, -18.08805785897195051 ) ) ;
#10185 = LINE ( 'NONE', #19496, #28754 ) ;
#10186 = DIRECTION ( 'NONE',  ( -2.698458740408365879E-16, 1.000000000000000000, 0.000000000000000000 ) ) ;
#10187 = FACE_OUTER_BOUND ( 'NONE', #5556, .T. ) ;
#10188 = CARTESIAN_POINT ( 'NONE',  ( 147.0152310637606092, -4.999999999999976907, -24.27857615940569502 ) ) ;
#10189 = CARTESIAN_POINT ( 'NONE',  ( -13.00000000000000178, -2.870178842070716726E-15, 23.00000000000000000 ) ) ;
#10190 = VECTOR ( 'NONE', #8286, 1000.000000000000000 ) ;
#10191 = DIRECTION ( 'NONE',  ( -0.000000000000000000, -0.000000000000000000, 1.000000000000000000 ) ) ;
#10192 = ORIENTED_EDGE ( 'NONE', *, *, #12719, .T. ) ;
#10193 = DIRECTION ( 'NONE',  ( 0.000000000000000000, 0.000000000000000000, 1.000000000000000000 ) ) ;
#10194 = DIRECTION ( 'NONE',  ( 1.000000000000000000, 4.440892098500622217E-16, 0.000000000000000000 ) ) ;
#10195 = AXIS2_PLACEMENT_3D ( 'NONE', #19171, #9548, #28230 ) ;
#10196 = CARTESIAN_POINT ( 'NONE',  ( 11.89844042902047505, 9.910446108148166289, -16.74492965742949835 ) ) ;
#10197 = CARTESIAN_POINT ( 'NONE',  ( 33.36629945566365052, -11.89386221509426633, -18.35752312617820081 ) ) ;
#10198 = EDGE_LOOP ( 'NONE', ( #3753, #19408, #3663, #725 ) ) ;
#10199 = CARTESIAN_POINT ( 'NONE',  ( 10.02031722384195156, 12.01814620627372143, -16.67932286086919902 ) ) ;
#10200 = CARTESIAN_POINT ( 'NONE',  ( 23.11440248821028831, -7.346120041196752659, -16.32852059634029018 ) ) ;
#10201 = CARTESIAN_POINT ( 'NONE',  ( 12.83240265444113071, 9.539962209189782882, -16.14097488725632346 ) ) ;
#10202 = FACE_BOUND ( 'NONE', #20795, .T. ) ;
#10203 = VERTEX_POINT ( 'NONE', #5525 ) ;
#10204 = VERTEX_POINT ( 'NONE', #14806 ) ;
#10205 = CARTESIAN_POINT ( 'NONE',  ( -20.00000000000017053, 34.64101615137744972, 4.999999999999998224 ) ) ;
#10206 = CARTESIAN_POINT ( 'NONE',  ( 11.47250673971808688, 9.270976631574885829, -15.86106510822916249 ) ) ;
#10207 = DIRECTION ( 'NONE',  ( -0.9510565162951536422, -2.566386769018988323E-16, 0.3090169943749475623 ) ) ;
#10208 = VERTEX_POINT ( 'NONE', #26291 ) ;
#10209 = ADVANCED_FACE ( 'NONE', ( #6400 ), #15691, .T. ) ;
#10210 = CARTESIAN_POINT ( 'NONE',  ( 144.5152310637605240, -1.999999999999978018, -4.391296821672111328 ) ) ;
#10211 = VERTEX_POINT ( 'NONE', #10388 ) ;
#10212 = MECHANICAL_DESIGN_GEOMETRIC_PRESENTATION_REPRESENTATION (  '', ( #20957 ), #3416 ) ;
#10213 = EDGE_CURVE ( 'NONE', #20918, #18221, #12831, .T. ) ;
#10214 = CARTESIAN_POINT ( 'NONE',  ( 12.02748425217687789, 9.318634685891279190, -16.69156549717016702 ) ) ;
#10215 = ORIENTED_EDGE ( 'NONE', *, *, #2009, .T. ) ;
#10216 = AXIS2_PLACEMENT_3D ( 'NONE', #2428, #428, #23315 ) ;
#10217 = CARTESIAN_POINT ( 'NONE',  ( 35.76309413546784555, -19.65568143964299352, -21.39484760613106573 ) ) ;
#10218 = CARTESIAN_POINT ( 'NONE',  ( 22.64650317123243894, 5.657944777580039997, -17.08144094666319646 ) ) ;
#10219 = CARTESIAN_POINT ( 'NONE',  ( 13.26656245924271005, 6.725567473591735457, -17.69027979179009691 ) ) ;
#10220 = CARTESIAN_POINT ( 'NONE',  ( 63.44486372867149981, -20.00000000000000355, -17.99999999999998934 ) ) ;
#10221 = ORIENTED_EDGE ( 'NONE', *, *, #27973, .F. ) ;
#10222 = VECTOR ( 'NONE', #26835, 1000.000000000000000 ) ;
#10223 = LINE ( 'NONE', #29669, #27919 ) ;
#10224 = APPLICATION_PROTOCOL_DEFINITION ( 'draft international standard', 'automotive_design', 1998, #16112 ) ;
#10225 = CARTESIAN_POINT ( 'NONE',  ( 19.18059203083059217, 2.087369379035357575, -14.72322290489779917 ) ) ;
#10226 = CARTESIAN_POINT ( 'NONE',  ( 21.41025690189560748, 5.821651141963339882, -16.00656683556521998 ) ) ;
#10227 = VERTEX_POINT ( 'NONE', #16966 ) ;
#10228 = FACE_BOUND ( 'NONE', #20948, .T. ) ;
#10229 = AXIS2_PLACEMENT_3D ( 'NONE', #30176, #9339, #20791 ) ;
#10230 = EDGE_CURVE ( 'NONE', #10227, #12932, #3250, .T. ) ;
#10231 = PLANE ( 'NONE',  #28225 ) ;
#10232 = CARTESIAN_POINT ( 'NONE',  ( 129.5152310637605808, -1.999999999999982236, -28.60870317832789311 ) ) ;
#10233 = CIRCLE ( 'NONE', #29297, 5.000000000000000888 ) ;
#10234 = FACE_OUTER_BOUND ( 'NONE', #27158, .T. ) ;
#10235 = CARTESIAN_POINT ( 'NONE',  ( 137.2287565553230309, -1.999999999999979572, -3.509618943233403510 ) ) ;
#10236 = CARTESIAN_POINT ( 'NONE',  ( 12.27441163154304071, 9.506095234784829984, -15.31172292274672664 ) ) ;
#10237 = CARTESIAN_POINT ( 'NONE',  ( -4.681481898397005459, 6.534749472788154101, -2.430984558619841973E-15 ) ) ;
#10238 = CARTESIAN_POINT ( 'NONE',  ( 8.000000000000000000, -4.618802153517027165, -4.285468820183664818 ) ) ;
#10239 = ORIENTED_EDGE ( 'NONE', *, *, #25757, .T. ) ;
#10240 = CARTESIAN_POINT ( 'NONE',  ( 12.50140887008201851, 8.571324787501421127, -15.12905211845398412 ) ) ;
#10241 = CARTESIAN_POINT ( 'NONE',  ( 10.60386377644718614, 9.341927331141327784, -16.43800583390468262 ) ) ;
#10242 = LINE ( 'NONE', #29537, #12696 ) ;
#10243 = DIRECTION ( 'NONE',  ( -2.908569913943825554E-16, 1.000000000000000000, -0.000000000000000000 ) ) ;
#10244 = CARTESIAN_POINT ( 'NONE',  ( 132.0152310637605524, -1.999999999999981348, -34.70218595412750773 ) ) ;
#10245 = EDGE_CURVE ( 'NONE', #8203, #19707, #1453, .T. ) ;
#10246 = LINE ( 'NONE', #19561, #16390 ) ;
#10247 = ORIENTED_EDGE ( 'NONE', *, *, #19312, .F. ) ;
#10248 = CARTESIAN_POINT ( 'NONE',  ( 12.83021228909557010, 9.549978240774745331, -16.14188291223562288 ) ) ;
#10249 = AXIS2_PLACEMENT_3D ( 'NONE', #28087, #4849, #14149 ) ;
#10250 = ORIENTED_EDGE ( 'NONE', *, *, #27396, .F. ) ;
#10252 = VECTOR ( 'NONE', #1005, 1000.000000000000000 ) ;
#10251 = CARTESIAN_POINT ( 'NONE',  ( 35.54859390954303677, -21.18451583373416014, -15.55638201429745848 ) ) ;
#10253 = CARTESIAN_POINT ( 'NONE',  ( 18.21616227284554057, 4.699354889203569918, -13.86658597208997179 ) ) ;
#10254 = ORIENTED_EDGE ( 'NONE', *, *, #7198, .F. ) ;
#10255 = CARTESIAN_POINT ( 'NONE',  ( 113.2356977018776263, -4.999999999999986677, -82.27055006877300514 ) ) ;
#10256 = CARTESIAN_POINT ( 'NONE',  ( 19.42071131597032974, 7.574497315622086724, -15.00200944635056644 ) ) ;
#10257 = FACE_OUTER_BOUND ( 'NONE', #13592, .T. ) ;
#10258 = DIRECTION ( 'NONE',  ( 1.000000000000000000, 0.000000000000000000, 0.000000000000000000 ) ) ;
#10259 = SHAPE_REPRESENTATION_RELATIONSHIP ( 'NONE' , 'NONE' ,  #11460, #17465 ) ;
#10260 = AXIS2_PLACEMENT_3D ( 'NONE', #5782, #5936, #24552 ) ;
#10261 = CARTESIAN_POINT ( 'NONE',  ( 25.46127020808262387, -4.208148299910691392, -19.59612275642668777 ) ) ;
#10262 = CARTESIAN_POINT ( 'NONE',  ( 20.43163981785493988, 0.2187255735321424754, -20.49791845872360341 ) ) ;
#10263 = VERTEX_POINT ( 'NONE', #18734 ) ;
#10264 = DIRECTION ( 'NONE',  ( -0.5877852522924731371, 0.000000000000000000, 0.8090169943749474513 ) ) ;
#10265 = DIRECTION ( 'NONE',  ( -1.000000000000000000, 0.000000000000000000, -0.000000000000000000 ) ) ;
#10266 = AXIS2_PLACEMENT_3D ( 'NONE', #10463, #19769, #19179 ) ;
#10267 = ADVANCED_FACE ( 'NONE', ( #2278 ), #23313, .T. ) ;
#10268 = EDGE_CURVE ( 'NONE', #21323, #16948, #30244, .T. ) ;
#10269 = LINE ( 'NONE', #12264, #16373 ) ;
#10270 = CARTESIAN_POINT ( 'NONE',  ( -7.999999999999994671, -1.555946510856153431, -4.932911297836646725 ) ) ;
#10271 = VECTOR ( 'NONE', #25807, 1000.000000000000000 ) ;
#10272 = ADVANCED_FACE ( 'NONE', ( #27784 ), #11703, .T. ) ;
#10273 = CARTESIAN_POINT ( 'NONE',  ( 149.5152310637605524, -10.00000000000000178, -21.71180489736091346 ) ) ;
#10274 = ORIENTED_EDGE ( 'NONE', *, *, #8357, .F. ) ;
#10275 = CARTESIAN_POINT ( 'NONE',  ( 9.936961226781097167, 16.31318409042999917, -16.49606719383117337 ) ) ;
#10276 = CARTESIAN_POINT ( 'NONE',  ( 26.02011856185544048, -9.832954462109395166, -14.66174570188732140 ) ) ;
#10277 = CARTESIAN_POINT ( 'NONE',  ( 28.56881743257453721, -8.627791766613455593, -12.78522491232925873 ) ) ;
#10278 = CARTESIAN_POINT ( 'NONE',  ( 32.96569147872224903, -11.36116021242123608, -19.12347989294568151 ) ) ;
#10280 = DIRECTION ( 'NONE',  ( 1.000000000000000000, 0.000000000000000000, 0.000000000000000000 ) ) ;
#10279 =( GEOMETRIC_REPRESENTATION_CONTEXT ( 3 ) GLOBAL_UNCERTAINTY_ASSIGNED_CONTEXT ( ( #17738 ) ) GLOBAL_UNIT_ASSIGNED_CONTEXT ( ( #18528, #6940, #26014 ) ) REPRESENTATION_CONTEXT ( 'NONE', 'WORKASPACE' ) );
#10281 = CARTESIAN_POINT ( 'NONE',  ( 180.7287565553229740, -84.33034373659253902, -33.50000000000000000 ) ) ;
#10282 = CARTESIAN_POINT ( 'NONE',  ( 154.5152310637605240, -10.00000000000000000, -21.71180489736091346 ) ) ;
#10283 = CARTESIAN_POINT ( 'NONE',  ( 164.5152310637604955, -9.999999999999996447, -30.37205893520531319 ) ) ;
#10284 = CARTESIAN_POINT ( 'NONE',  ( 143.6922820468854241, -1.999999999999978462, -9.266330736598359152 ) ) ;
#10285 = DIRECTION ( 'NONE',  ( 1.000000000000000000, 4.440892098500622217E-16, 0.000000000000000000 ) ) ;
#10287 = ORIENTED_EDGE ( 'NONE', *, *, #23243, .T. ) ;
#10286 = CARTESIAN_POINT ( 'NONE',  ( 17.96884874826282186, 1.586046385177752871, -19.67104016136476119 ) ) ;
#10288 = ORIENTED_EDGE ( 'NONE', *, *, #11656, .F. ) ;
#10289 = CARTESIAN_POINT ( 'NONE',  ( 168.6922820468853956, -9.999999999999996447, -35.24709285013155835 ) ) ;
#10290 = CARTESIAN_POINT ( 'NONE',  ( 12.26073475921635669, 9.568819114670704451, -15.31737879056614737 ) ) ;
#10291 = CARTESIAN_POINT ( 'NONE',  ( 33.17819505895439391, -11.78846528140086924, -19.49437495119144259 ) ) ;
#10292 = DIRECTION ( 'NONE',  ( 0.9510565162951536422, 0.000000000000000000, -0.3090169943749475623 ) ) ;
#10293 = CARTESIAN_POINT ( 'NONE',  ( 19.38992137333195842, 2.881095379261479739, -20.30776781288435373 ) ) ;
#10294 = LINE ( 'NONE', #22358, #4734 ) ;
#10295 = CARTESIAN_POINT ( 'NONE',  ( 19.69411524970139737, 8.437195840132273972, -14.56566581881308409 ) ) ;
#10296 = VERTEX_POINT ( 'NONE', #1982 ) ;
#10298 = VECTOR ( 'NONE', #26037, 1000.000000000000000 ) ;
#10297 = CARTESIAN_POINT ( 'NONE',  ( 33.48796008207983022, -12.92717959506727965, -19.73506838908087246 ) ) ;
#10299 = AXIS2_PLACEMENT_3D ( 'NONE', #25390, #17893, #2203 ) ;
#10300 = CARTESIAN_POINT ( 'NONE',  ( 31.00997733146710900, -7.209757123251725019, -15.04105334301871011 ) ) ;
#10301 = AXIS2_PLACEMENT_3D ( 'NONE', #4970, #560, #21143 ) ;
#10302 = CARTESIAN_POINT ( 'NONE',  ( 19.28943675834911531, -1.002762487816046155, -14.40755329178536037 ) ) ;
#10303 = CARTESIAN_POINT ( 'NONE',  ( 29.62588713853392264, -10.65184931322849060, -12.76488833982454629 ) ) ;
#10304 = CARTESIAN_POINT ( 'NONE',  ( 25.00000000000001066, 60.00000000000000711, 24.99999999999998579 ) ) ;
#10305 = EDGE_LOOP ( 'NONE', ( #10023, #27467, #18763, #15744 ) ) ;
#10306 = EDGE_CURVE ( 'NONE', #3603, #28443, #9105, .T. ) ;
#10307 = ORIENTED_EDGE ( 'NONE', *, *, #18379, .T. ) ;
#10308 = DIRECTION ( 'NONE',  ( 0.3090169943749475623, 8.338696094058001131E-17, 0.9510565162951536422 ) ) ;
#10309 = EDGE_CURVE ( 'NONE', #24750, #3893, #18189, .T. ) ;
#10310 = CARTESIAN_POINT ( 'NONE',  ( 84.87592175515526094, -4.999999999999994671, 61.66596675877570988 ) ) ;
#10311 = ADVANCED_FACE ( 'NONE', ( #11263 ), #4689, .T. ) ;
#10312 = B_SPLINE_CURVE_WITH_KNOTS ( 'NONE', 3,
 ( #6020, #15463, #1607, #3733, #18056, #6472 ),
 .UNSPECIFIED., .F., .F.,
 ( 4, 2, 4 ),
 ( 0.004120275011746852255, 0.005288420935197119671, 0.006456566858647387955 ),
 .UNSPECIFIED. ) ;
#10313 = DIRECTION ( 'NONE',  ( -1.110223024625156540E-16, 0.000000000000000000, -1.000000000000000000 ) ) ;
#10314 = CARTESIAN_POINT ( 'NONE',  ( 35.98907965336992731, -19.67091466371804742, -20.42083605867238205 ) ) ;
#10315 = CARTESIAN_POINT ( 'NONE',  ( 11.31072706937237982, 10.01291882189198112, -15.92796669285280764 ) ) ;
#10316 = CARTESIAN_POINT ( 'NONE',  ( 174.7287565553229456, -4.999999999999969802, -33.82050807568879947 ) ) ;
#10317 = CARTESIAN_POINT ( 'NONE',  ( 1.313474075707222966, 8.479269695850875976, -4.683279549040151757 ) ) ;
#10318 = CARTESIAN_POINT ( 'NONE',  ( 9.661883135045433946, 16.25482629684424296, -17.91562380025844803 ) ) ;
#10319 = DIRECTION ( 'NONE',  ( 0.5877852522924731371, 0.000000000000000000, 0.8090169943749474513 ) ) ;
#10320 = ORIENTED_EDGE ( 'NONE', *, *, #13610, .T. ) ;
#10321 = LINE ( 'NONE', #5761, #281 ) ;
#10322 = ORIENTED_EDGE ( 'NONE', *, *, #26256, .F. ) ;
#10323 = ORIENTED_EDGE ( 'NONE', *, *, #27730, .F. ) ;
#10324 = DIRECTION ( 'NONE',  ( 1.000000000000000000, 4.440892098500622217E-16, 0.000000000000000000 ) ) ;
#10325 = CARTESIAN_POINT ( 'NONE',  ( 167.2287565553229740, -9.999999999999996447, -29.49038105676660493 ) ) ;
#10326 = VECTOR ( 'NONE', #13162, 1000.000000000000000 ) ;
#10327 = DIRECTION ( 'NONE',  ( 1.000000000000000000, 2.698458740408365879E-16, -1.110223024625156540E-16 ) ) ;
#10328 = ORIENTED_EDGE ( 'NONE', *, *, #29293, .T. ) ;
#10329 = ORIENTED_EDGE ( 'NONE', *, *, #10522, .F. ) ;
#10330 = CARTESIAN_POINT ( 'NONE',  ( 13.16425014233558954, 7.550783913790151125, -15.87799427043765021 ) ) ;
#10331 = CARTESIAN_POINT ( 'NONE',  ( 17.99586569009407455, 10.99629947005995767, -19.18704736271931210 ) ) ;
#10332 = CARTESIAN_POINT ( 'NONE',  ( 30.78125299044525320, -8.317598597646391312, -16.28273480984023891 ) ) ;
#10333 = CARTESIAN_POINT ( 'NONE',  ( 169.5152310637604671, -4.999999999999971578, -11.28819510263909542 ) ) ;
#10334 = DIRECTION ( 'NONE',  ( -2.698458740408365879E-16, 1.000000000000000000, 0.000000000000000000 ) ) ;
#10335 = VECTOR ( 'NONE', #6870, 1000.000000000000000 ) ;
#10336 = CARTESIAN_POINT ( 'NONE',  ( 133.6922820468854241, -4.999999999999982236, -0.6060766987539614181 ) ) ;
#10337 = ORIENTED_EDGE ( 'NONE', *, *, #26498, .F. ) ;
#10338 = DIRECTION ( 'NONE',  ( 1.110223024625156540E-16, 2.995891024602366092E-32, 1.000000000000000000 ) ) ;
#10339 = VERTEX_POINT ( 'NONE', #1831 ) ;
#10340 = DIRECTION ( 'NONE',  ( -0.5877852522924731371, -1.586114251531760235E-16, 0.8090169943749474513 ) ) ;
#10342 = VERTEX_POINT ( 'NONE', #11400 ) ;
#10341 = CARTESIAN_POINT ( 'NONE',  ( 91.48631020676766923, -4.999999999999992895, -66.46869509550764121 ) ) ;
#10343 = EDGE_CURVE ( 'NONE', #20011, #28465, #23161, .T. ) ;
#10344 = CARTESIAN_POINT ( 'NONE',  ( 141.1922820468854525, -10.00000000000000533, -10.74328820663507678 ) ) ;
#10345 = CARTESIAN_POINT ( 'NONE',  ( 168.6922820468853104, -4.999999999999972466, -9.266330736598359152 ) ) ;
#10346 = EDGE_CURVE ( 'NONE', #15181, #19023, #4549, .T. ) ;
#10347 = EDGE_CURVE ( 'NONE', #18869, #29035, #5442, .T. ) ;
#10348 = EDGE_CURVE ( 'NONE', #9725, #26738, #18125, .T. ) ;
#10349 = CARTESIAN_POINT ( 'NONE',  ( 12.72883512080982804, 8.524354266104470668, -16.21679389071614352 ) ) ;
#10350 = VERTEX_POINT ( 'NONE', #16282 ) ;
#10351 = CARTESIAN_POINT ( 'NONE',  ( 35.45944968151609800, -21.78403803824750185, -19.54251958818673174 ) ) ;
#10352 = VERTEX_POINT ( 'NONE', #30096 ) ;
#10353 = CARTESIAN_POINT ( 'NONE',  ( 8.944914148442956403, 16.95008179206086396, -17.86239244656949765 ) ) ;
#10354 = VECTOR ( 'NONE', #28409, 1000.000000000000000 ) ;
#10355 = CARTESIAN_POINT ( 'NONE',  ( 23.61827771231835982, -0.6465389018800060672, -13.57143891608981612 ) ) ;
#10356 = CARTESIAN_POINT ( 'NONE',  ( 12.83224840168406544, 9.540640483216481726, -16.14104089933701758 ) ) ;
#10357 = FACE_BOUND ( 'NONE', #21085, .T. ) ;
#10358 = ORIENTED_EDGE ( 'NONE', *, *, #21166, .F. ) ;
#10359 = ORIENTED_EDGE ( 'NONE', *, *, #23419, .T. ) ;
#10360 = CARTESIAN_POINT ( 'NONE',  ( 0.2500000000000002220, 0.000000000000000000, 0.000000000000000000 ) ) ;
#10361 = CARTESIAN_POINT ( 'NONE',  ( 12.48799528366842360, 8.565546312597838607, -15.13973160209665991 ) ) ;
#10362 = DIRECTION ( 'NONE',  ( -2.698458740408365879E-16, 1.000000000000000000, 0.000000000000000000 ) ) ;
#10363 = ORIENTED_EDGE ( 'NONE', *, *, #14912, .F. ) ;
#10364 = DIRECTION ( 'NONE',  ( -2.698458740408365879E-16, 1.000000000000000000, 0.000000000000000000 ) ) ;
#10365 = ORIENTED_EDGE ( 'NONE', *, *, #28976, .T. ) ;
#10366 = CARTESIAN_POINT ( 'NONE',  ( 11.89844042902047505, 9.910446108148166289, -16.74492965742949835 ) ) ;
#10367 = VERTEX_POINT ( 'NONE', #6543 ) ;
#10368 = CARTESIAN_POINT ( 'NONE',  ( 18.97315296117551497, 8.914538345978252565, -15.07232217507325345 ) ) ;
#10369 = CARTESIAN_POINT ( 'NONE',  ( 15.57351372253994271, 10.71565324155555388, -15.28765949597478624 ) ) ;
#10370 = VECTOR ( 'NONE', #23962, 1000.000000000000000 ) ;
#10371 = LINE ( 'NONE', #8081, #30200 ) ;
#10372 = ORIENTED_EDGE ( 'NONE', *, *, #16179, .T. ) ;
#10373 = CARTESIAN_POINT ( 'NONE',  ( 36.54859390953723874, -22.18451583373416014, -15.00000000000000000 ) ) ;
#10374 = ADVANCED_FACE ( 'NONE', ( #28081 ), #25163, .T. ) ;
#10375 = CARTESIAN_POINT ( 'NONE',  ( 18.46387099684246635, 2.251061286204190992, -18.51322769290417369 ) ) ;
#10376 = CARTESIAN_POINT ( 'NONE',  ( 14.24706144987486667, 6.238427219560604087, -16.72753349211556184 ) ) ;
#10377 = AXIS2_PLACEMENT_3D ( 'NONE', #28072, #13688, #9095 ) ;
#10378 = DIRECTION ( 'NONE',  ( -1.110223024625156540E-16, 0.000000000000000000, -1.000000000000000000 ) ) ;
#10379 = FACE_BOUND ( 'NONE', #7632, .T. ) ;
#10380 = EDGE_CURVE ( 'NONE', #5681, #17796, #6848, .T. ) ;
#10381 = EDGE_CURVE ( 'NONE', #20167, #6302, #21020, .T. ) ;
#10382 = EDGE_CURVE ( 'NONE', #15160, #30082, #7138, .T. ) ;
#10383 = CARTESIAN_POINT ( 'NONE',  ( 164.5152310637604955, -9.999999999999998224, -19.94844914048349693 ) ) ;
#10384 = CARTESIAN_POINT ( 'NONE',  ( 154.7287565553230309, -10.00000000000000000, -33.82050807568879947 ) ) ;
#10385 = CARTESIAN_POINT ( 'NONE',  ( 80.75772623742359713, -4.999999999999995559, 58.67392257650259779 ) ) ;
#10386 = DIRECTION ( 'NONE',  ( -0.000000000000000000, -0.000000000000000000, 1.000000000000000000 ) ) ;
#10387 = CARTESIAN_POINT ( 'NONE',  ( 12.11484812106508713, 10.23787383345373136, -15.37770804730690166 ) ) ;
#10388 = CARTESIAN_POINT ( 'NONE',  ( 171.1922820468853388, -1.999999999999970912, -19.40354224447947828 ) ) ;
#10389 = ORIENTED_EDGE ( 'NONE', *, *, #9544, .F. ) ;
#10390 = CARTESIAN_POINT ( 'NONE',  ( 144.5152310637605808, -4.999999999999978684, -11.28819510263909542 ) ) ;
#10391 = ORIENTED_EDGE ( 'NONE', *, *, #28844, .T. ) ;
#10392 = CARTESIAN_POINT ( 'NONE',  ( 11.47372892693763902, 9.265404009280679531, -15.86055721330185619 ) ) ;
#10393 = VERTEX_POINT ( 'NONE', #23028 ) ;
#10394 = VECTOR ( 'NONE', #21580, 1000.000000000000000 ) ;
#10395 = CARTESIAN_POINT ( 'NONE',  ( 10.65249265583095095, 9.118909091547207524, -16.41789608165773728 ) ) ;
#10396 = LINE ( 'NONE', #17715, #10763 ) ;
#10397 = CARTESIAN_POINT ( 'NONE',  ( 164.5152310637604671, -1.999999999999972689, -2.627941064794695691 ) ) ;
#10398 = ORIENTED_EDGE ( 'NONE', *, *, #28071, .T. ) ;
#10399 = LINE ( 'NONE', #3116, #4685 ) ;
#10400 = ORIENTED_EDGE ( 'NONE', *, *, #5511, .F. ) ;
#10401 = CARTESIAN_POINT ( 'NONE',  ( 12.83198842527593087, 9.541832653742346793, -16.14114841745374562 ) ) ;
#10402 = CARTESIAN_POINT ( 'NONE',  ( 34.71713976128472723, -12.95676249388076329, -18.99403759477717557 ) ) ;
#10403 = CARTESIAN_POINT ( 'NONE',  ( 21.58242789233717573, 5.264303332692052528, -18.32037006577847293 ) ) ;
#10404 = VERTEX_POINT ( 'NONE', #13399 ) ;
#10405 = VERTEX_POINT ( 'NONE', #22727 ) ;
#10406 = DIRECTION ( 'NONE',  ( 0.9510565162951536422, 2.566386769018988816E-16, 0.3090169943749472292 ) ) ;
#10407 = CARTESIAN_POINT ( 'NONE',  ( 13.98191416104776685, 5.331502061239655532, -16.22335970869868760 ) ) ;
#10408 = CARTESIAN_POINT ( 'NONE',  ( 8.000000000000014211, -0.7805016046290974563, -4.999999999999993783 ) ) ;
#10409 = CARTESIAN_POINT ( 'NONE',  ( 0.000000000000000000, 0.000000000000000000, 9.999999999999998224 ) ) ;
#10410 = EDGE_CURVE ( 'NONE', #19213, #26420, #15832, .T. ) ;
#10411 =( NAMED_UNIT ( * ) SI_UNIT ( $, .STERADIAN. ) SOLID_ANGLE_UNIT ( ) );
#10412 = CARTESIAN_POINT ( 'NONE',  ( 23.07678757892180244, -0.1267571646896241688, -14.23703129728563965 ) ) ;
#10413 = CARTESIAN_POINT ( 'NONE',  ( 21.41414477019618090, -0.8106431452899078849, -12.56463806509592018 ) ) ;
#10414 = VERTEX_POINT ( 'NONE', #2715 ) ;
#10415 = ORIENTED_EDGE ( 'NONE', *, *, #28278, .T. ) ;
#10416 = FACE_OUTER_BOUND ( 'NONE', #22691, .T. ) ;
#10417 = VECTOR ( 'NONE', #24403, 1000.000000000000000 ) ;
#10418 = DIRECTION ( 'NONE',  ( -1.000000000000000000, -4.440892098500622217E-16, 0.000000000000000000 ) ) ;
#10419 = FACE_OUTER_BOUND ( 'NONE', #1502, .T. ) ;
#10420 = CARTESIAN_POINT ( 'NONE',  ( 10.55189716074911921, 7.593251366112848899, 4.999999999999998224 ) ) ;
#10421 = CARTESIAN_POINT ( 'NONE',  ( 138.6922820468854525, -10.00000000000000533, -26.58683881228715506 ) ) ;
#10422 = CARTESIAN_POINT ( 'NONE',  ( 9.957223259857686415, 16.22025982393231303, -16.48768813039480818 ) ) ;
#10423 = CARTESIAN_POINT ( 'NONE',  ( 16.09764958744793262, 8.143416238145906760, -19.84970969296679044 ) ) ;
#10424 = CARTESIAN_POINT ( 'NONE',  ( 22.24201797625671517, -7.474445146391827777, -15.38054711335415803 ) ) ;
#10425 = ORIENTED_EDGE ( 'NONE', *, *, #29866, .T. ) ;
#10426 = CARTESIAN_POINT ( 'NONE',  ( 177.2287565553228319, -1.999999999999969358, -3.509618943233403510 ) ) ;
#10427 = DIRECTION ( 'NONE',  ( -2.698458740408365879E-16, 1.000000000000000000, 0.000000000000000000 ) ) ;
#10428 = CARTESIAN_POINT ( 'NONE',  ( 159.5152310637605524, -1.999999999999972689, -28.60870317832789667 ) ) ;
#10429 = FACE_OUTER_BOUND ( 'NONE', #11589, .T. ) ;
#10430 = DIRECTION ( 'NONE',  ( 1.000000000000000000, 0.000000000000000000, 0.000000000000000000 ) ) ;
#10431 = CARTESIAN_POINT ( 'NONE',  ( 147.0152310637606092, -1.999999999999976241, -32.93883019725009120 ) ) ;
#10432 = CARTESIAN_POINT ( 'NONE',  ( 20.24985932600369409, 3.694099309552050237, -20.13309853732883781 ) ) ;
#10433 = ORIENTED_EDGE ( 'NONE', *, *, #8104, .T. ) ;
#10434 = LINE ( 'NONE', #8002, #23187 ) ;
#10435 = CARTESIAN_POINT ( 'NONE',  ( 12.27681432698556918, 9.495076167121005994, -15.31072932366845407 ) ) ;
#10436 = DIRECTION ( 'NONE',  ( 0.000000000000000000, 0.000000000000000000, 1.000000000000000000 ) ) ;
#10437 = PLANE ( 'NONE',  #6420 ) ;
#10438 = ORIENTED_EDGE ( 'NONE', *, *, #5852, .T. ) ;
#10439 = CARTESIAN_POINT ( 'NONE',  ( 23.16390915794477223, 2.882539813099532555, -14.99485278278146438 ) ) ;
#10440 = AXIS2_PLACEMENT_3D ( 'NONE', #15332, #24517, #20370 ) ;
#10441 = CARTESIAN_POINT ( 'NONE',  ( 420.0000000000002274, 34.64101615137744972, 14.00000000000000178 ) ) ;
#10442 = CARTESIAN_POINT ( 'NONE',  ( 18.04051923446642292, -0.4597542321540471488, -16.60176153622942508 ) ) ;
#10443 = EDGE_LOOP ( 'NONE', ( #14361, #29033, #21426, #17011 ) ) ;
#10444 = DIRECTION ( 'NONE',  ( -0.9510565162951536422, 0.000000000000000000, -0.3090169943749472292 ) ) ;
#10445 = ADVANCED_FACE ( 'NONE', ( #9709 ), #14735, .F. ) ;
#10446 = DIRECTION ( 'NONE',  ( 1.000000000000000000, 0.000000000000000000, 0.000000000000000000 ) ) ;
#10447 = CARTESIAN_POINT ( 'NONE',  ( 30.62308825650849187, -7.210737555064373083, -14.15269394828060889 ) ) ;
#10448 = EDGE_CURVE ( 'NONE', #22172, #8011, #24079, .T. ) ;
#10449 = CARTESIAN_POINT ( 'NONE',  ( 20.16317987096495656, -0.6177526724804084379, -13.65447574297484223 ) ) ;
#10450 = APPLICATION_CONTEXT ( 'automotive_design' ) ;
#10451 = B_SPLINE_CURVE_WITH_KNOTS ( 'NONE', 3,
 ( #28133, #7191, #9456, #16333, #21367, #13885, #9151, #14332 ),
 .UNSPECIFIED., .F., .F.,
 ( 4, 2, 2, 4 ),
 ( 0.004673709593152178265, 0.005837709341827659881, 0.007001709090503141497, 0.009329708587854104729 ),
 .UNSPECIFIED. ) ;
#10452 = VERTEX_POINT ( 'NONE', #5302 ) ;
#10453 = LINE ( 'NONE', #24661, #29856 ) ;
#10454 = ORIENTED_EDGE ( 'NONE', *, *, #25072, .T. ) ;
#10455 = DIRECTION ( 'NONE',  ( -2.698458740408365879E-16, 1.000000000000000000, 0.000000000000000000 ) ) ;
#10456 = ORIENTED_EDGE ( 'NONE', *, *, #3113, .F. ) ;
#10457 = DIRECTION ( 'NONE',  ( 1.000000000000000000, 0.000000000000000000, 0.000000000000000000 ) ) ;
#10458 = DIRECTION ( 'NONE',  ( 0.000000000000000000, 0.000000000000000000, 1.000000000000000000 ) ) ;
#10459 = PLANE ( 'NONE',  #14328 ) ;
#10460 = CARTESIAN_POINT ( 'NONE',  ( 20.00000000000017053, 34.64101615137744972, 10.00000000000000178 ) ) ;
#10461 = CARTESIAN_POINT ( 'NONE',  ( 34.39307579391925174, -12.50091474996580487, -19.93840237985029162 ) ) ;
#10462 = CARTESIAN_POINT ( 'NONE',  ( 10.04637620539468124, 15.81139305134258599, -16.45082025127570091 ) ) ;
#10463 = CARTESIAN_POINT ( 'NONE',  ( 3.999999999999998224, 2.309401076758477167, -2.450000000000000178 ) ) ;
#10464 = FACE_OUTER_BOUND ( 'NONE', #1219, .T. ) ;
#10465 = CARTESIAN_POINT ( 'NONE',  ( 9.661883107508126400, 16.25482642313383508, -17.91565355200308218 ) ) ;
#10466 = CARTESIAN_POINT ( 'NONE',  ( 0.000000000000000000, 0.000000000000000000, 9.480888224575629408 ) ) ;
#10467 = FACE_OUTER_BOUND ( 'NONE', #1849, .T. ) ;
#10468 = ORIENTED_EDGE ( 'NONE', *, *, #21306, .F. ) ;
#10469 = DIRECTION ( 'NONE',  ( -1.000000000000000000, -2.908569913943825554E-16, 0.000000000000000000 ) ) ;
#10470 = LINE ( 'NONE', #17646, #2990 ) ;
#10471 = EDGE_LOOP ( 'NONE', ( #12730, #24869, #14196, #29894 ) ) ;
#10472 = DIRECTION ( 'NONE',  ( -0.5877852522924731371, 0.000000000000000000, 0.8090169943749474513 ) ) ;
#10473 = VERTEX_POINT ( 'NONE', #3028 ) ;
#10474 = ORIENTED_EDGE ( 'NONE', *, *, #1761, .T. ) ;
#10475 = ORIENTED_EDGE ( 'NONE', *, *, #17818, .F. ) ;
#10476 = CARTESIAN_POINT ( 'NONE',  ( 13.38350887602579142, 7.627675785621035764, -15.70476675302002612 ) ) ;
#10477 = EDGE_CURVE ( 'NONE', #25465, #21788, #16748, .T. ) ;
#10478 = EDGE_CURVE ( 'NONE', #14190, #27415, #16593, .T. ) ;
#10479 = CARTESIAN_POINT ( 'NONE',  ( 29.95565488329840775, -10.73317148848732039, -11.80569981112315325 ) ) ;
#10480 = EDGE_CURVE ( 'NONE', #7930, #563, #2873, .T. ) ;
#10481 = CARTESIAN_POINT ( 'NONE',  ( 26.00956027078203192, -8.595392566010074731, -19.46287731774799212 ) ) ;
#10482 = LINE ( 'NONE', #19790, #13554 ) ;
#10483 = CARTESIAN_POINT ( 'NONE',  ( -24.00000000000017053, 34.64101615137744972, -10.00000000000000000 ) ) ;
#10484 = AXIS2_PLACEMENT_3D ( 'NONE', #11146, #10986, #2159 ) ;
#10485 = EDGE_CURVE ( 'NONE', #18105, #29393, #26220, .T. ) ;
#10486 = DIRECTION ( 'NONE',  ( -0.9510565162951536422, 0.000000000000000000, -0.3090169943749472292 ) ) ;
#10487 = ORIENTED_EDGE ( 'NONE', *, *, #20775, .F. ) ;
#10488 = CARTESIAN_POINT ( 'NONE',  ( 173.6922820468853388, -9.999999999999994671, -23.73366926340167637 ) ) ;
#10489 = AXIS2_PLACEMENT_3D ( 'NONE', #11228, #20530, #25276 ) ;
#10491 = ORIENTED_EDGE ( 'NONE', *, *, #21791, .F. ) ;
#10490 = DIRECTION ( 'NONE',  ( 1.000000000000000000, 2.698458740408367851E-16, 0.000000000000000000 ) ) ;
#10492 = DIRECTION ( 'NONE',  ( -2.698458740408365879E-16, 1.000000000000000000, 0.000000000000000000 ) ) ;
#10493 = LINE ( 'NONE', #5175, #27529 ) ;
#10494 = CARTESIAN_POINT ( 'NONE',  ( 12.90142504057275197, 8.513187104919181181, -16.08590544042818493 ) ) ;
#10495 = CARTESIAN_POINT ( 'NONE',  ( 32.01580575020638975, -11.60503005433848500, -14.58926670671732673 ) ) ;
#10496 = ORIENTED_EDGE ( 'NONE', *, *, #23011, .T. ) ;
#10497 = VECTOR ( 'NONE', #24294, 1000.000000000000000 ) ;
#10498 = CARTESIAN_POINT ( 'NONE',  ( 9.111692801717447665, 16.18521362881060455, -17.05508072787638696 ) ) ;
#10499 = CARTESIAN_POINT ( 'NONE',  ( 24.79644250101478065, -1.608028467720058918, -19.02763285027648976 ) ) ;
#10500 = CARTESIAN_POINT ( 'NONE',  ( 12.86924247997729687, 9.516471784987144744, -16.11464614809275631 ) ) ;
#10501 = FACE_BOUND ( 'NONE', #4262, .T. ) ;
#10502 = EDGE_CURVE ( 'NONE', #2770, #9840, #14587, .T. ) ;
#10503 = ORIENTED_EDGE ( 'NONE', *, *, #12931, .T. ) ;
#10504 = EDGE_LOOP ( 'NONE', ( #1122, #26852, #1280, #10556, #1426 ) ) ;
#10505 = CARTESIAN_POINT ( 'NONE',  ( 13.00000000000000178, 1.592040838891559293E-15, -15.00000000000000000 ) ) ;
#10506 = CARTESIAN_POINT ( 'NONE',  ( 11.47395765415086188, 9.264374527449886543, -15.86046114005151075 ) ) ;
#10507 = LINE ( 'NONE', #5650, #11093 ) ;
#10508 = VERTEX_POINT ( 'NONE', #21163 ) ;
#10509 = ORIENTED_EDGE ( 'NONE', *, *, #14268, .T. ) ;
#10510 = CARTESIAN_POINT ( 'NONE',  ( -24.00000000000017053, 34.64101615137744972, 4.999999999999998224 ) ) ;
#10511 = ORIENTED_EDGE ( 'NONE', *, *, #12371, .T. ) ;
#10512 = CARTESIAN_POINT ( 'NONE',  ( 12.02780084644370007, 9.317182744227245905, -16.69143457430396893 ) ) ;
#10513 = ORIENTED_EDGE ( 'NONE', *, *, #8833, .F. ) ;
#10514 = CARTESIAN_POINT ( 'NONE',  ( 14.47211339546095488, 7.927559549074161716, -19.99378091926031686 ) ) ;
#10515 = CARTESIAN_POINT ( 'NONE',  ( 15.30633068984937317, 3.801504677414661693, -19.72534293519717608 ) ) ;
#10516 = ORIENTED_EDGE ( 'NONE', *, *, #5850, .T. ) ;
#10517 = EDGE_CURVE ( 'NONE', #506, #21151, #9867, .T. ) ;
#10518 = VECTOR ( 'NONE', #6406, 1000.000000000000000 ) ;
#10519 = CARTESIAN_POINT ( 'NONE',  ( 18.15135754085015662, -5.000000000000012434, -55.86413428085646160 ) ) ;
#10520 = EDGE_CURVE ( 'NONE', #1114, #22451, #10165, .T. ) ;
#10521 = ORIENTED_EDGE ( 'NONE', *, *, #20242, .F. ) ;
#10522 = EDGE_CURVE ( 'NONE', #11518, #17686, #26374, .T. ) ;
#10523 = EDGE_CURVE ( 'NONE', #29689, #12166, #25918, .T. ) ;
#10524 = CARTESIAN_POINT ( 'NONE',  ( 36.54859390953724585, -22.18451583373416014, -17.78191007148576475 ) ) ;
#10525 = VECTOR ( 'NONE', #16107, 1000.000000000000000 ) ;
#10526 = CARTESIAN_POINT ( 'NONE',  ( 17.54642605795894994, 9.676486402519270058, -18.74681543856335608 ) ) ;
#10527 = CIRCLE ( 'NONE', #3256, 8.000000000000007105 ) ;
#10528 = PRESENTATION_STYLE_ASSIGNMENT (( #22133 ) ) ;
#10529 = FACE_BOUND ( 'NONE', #14123, .T. ) ;
#10530 = ORIENTED_EDGE ( 'NONE', *, *, #20329, .F. ) ;
#10531 = CARTESIAN_POINT ( 'NONE',  ( 20.00000000000017053, 41.64101615137744972, 12.00000000000000178 ) ) ;
#10532 = DIRECTION ( 'NONE',  ( 0.5877852522924731371, 1.586114251531760728E-16, 0.8090169943749474513 ) ) ;
#10533 = CARTESIAN_POINT ( 'NONE',  ( -11.85189716074912880, -5.341585316273318895, 4.999999999999998224 ) ) ;
#10534 = FACE_OUTER_BOUND ( 'NONE', #12403, .T. ) ;
#10535 = VECTOR ( 'NONE', #24811, 1000.000000000000000 ) ;
#10536 = CARTESIAN_POINT ( 'NONE',  ( 11.05541531668977662, 17.68942339022145305, -17.91664992932185996 ) ) ;
#10537 = CARTESIAN_POINT ( 'NONE',  ( 0.000000000000000000, 0.000000000000000000, -2.450000000000000622 ) ) ;
#10538 = ORIENTED_EDGE ( 'NONE', *, *, #19448, .T. ) ;
#10539 = DIRECTION ( 'NONE',  ( 0.3090169943749472292, 8.338696094057992503E-17, -0.9510565162951536422 ) ) ;
#10540 = VERTEX_POINT ( 'NONE', #12306 ) ;
#10541 = AXIS2_PLACEMENT_3D ( 'NONE', #21409, #19116, #25691 ) ;
#10542 = CARTESIAN_POINT ( 'NONE',  ( 11.47304865262203499, 9.268493388164605662, -15.86084085272616484 ) ) ;
#10543 = ORIENTED_EDGE ( 'NONE', *, *, #28912, .F. ) ;
#10544 = AXIS2_PLACEMENT_3D ( 'NONE', #6872, #2598, #18296 ) ;
#10545 = CARTESIAN_POINT ( 'NONE',  ( 11.11829553246053770, 8.091015213210848600, -16.14073874907621331 ) ) ;
#10546 = PLANE ( 'NONE',  #13206 ) ;
#10547 = LINE ( 'NONE', #17567, #6703 ) ;
#10548 = EDGE_LOOP ( 'NONE', ( #12998, #12952, #25242, #27686, #29327 ) ) ;
#10549 = VERTEX_POINT ( 'NONE', #12452 ) ;
#10550 = DIRECTION ( 'NONE',  ( 0.000000000000000000, 0.000000000000000000, -1.000000000000000000 ) ) ;
#10551 = ORIENTED_EDGE ( 'NONE', *, *, #11534, .T. ) ;
#10552 = CARTESIAN_POINT ( 'NONE',  ( 12.70256148071318414, 10.13540111970991653, -16.19467101188346092 ) ) ;
#10553 = ORIENTED_EDGE ( 'NONE', *, *, #10697, .F. ) ;
#10554 = CARTESIAN_POINT ( 'NONE',  ( 33.45149595566165601, -11.04796323883829423, -16.41509932566969354 ) ) ;
#10555 = CARTESIAN_POINT ( 'NONE',  ( 22.16846437878366061, -4.107540447007581363, -19.06500358040360865 ) ) ;
#10556 = ORIENTED_EDGE ( 'NONE', *, *, #13107, .T. ) ;
#10557 = EDGE_CURVE ( 'NONE', #19068, #14895, #21622, .T. ) ;
#10558 = VERTEX_POINT ( 'NONE', #21778 ) ;
#10559 = EDGE_CURVE ( 'NONE', #11271, #23695, #12158, .T. ) ;
#10560 = CARTESIAN_POINT ( 'NONE',  ( 91.06348369087051253, -4.999999999999992895, -66.16149364974000946 ) ) ;
#10561 = CARTESIAN_POINT ( 'NONE',  ( 16.94700227795405212, 10.49100606271714931, -14.51747230701220559 ) ) ;
#10562 = ADVANCED_FACE ( 'NONE', ( #25761 ), #28237, .T. ) ;
#10563 = FACE_OUTER_BOUND ( 'NONE', #24198, .T. ) ;
#10564 = EDGE_CURVE ( 'NONE', #22699, #18794, #5146, .T. ) ;
#10565 = DIRECTION ( 'NONE',  ( 0.000000000000000000, 0.000000000000000000, 1.000000000000000000 ) ) ;
#10566 = VERTEX_POINT ( 'NONE', #14285 ) ;
#10567 = CARTESIAN_POINT ( 'NONE',  ( 20.05514754915220266, -1.452567280579552866, -14.87399747198034738 ) ) ;
#10568 = CARTESIAN_POINT ( 'NONE',  ( 18.07093408371026300, -2.157424655934858215, -16.53044640867639359 ) ) ;
#10569 = VECTOR ( 'NONE', #27434, 1000.000000000000000 ) ;
#10570 = ORIENTED_EDGE ( 'NONE', *, *, #28738, .T. ) ;
#10571 = CARTESIAN_POINT ( 'NONE',  ( 159.5152310637604671, -4.999999999999974243, -2.627941064794695691 ) ) ;
#10572 = AXIS2_PLACEMENT_3D ( 'NONE', #25507, #18932, #20755 ) ;
#10573 = DIRECTION ( 'NONE',  ( 0.000000000000000000, 0.000000000000000000, 1.000000000000000000 ) ) ;
#10574 = VECTOR ( 'NONE', #22301, 1000.000000000000000 ) ;
#10575 = CARTESIAN_POINT ( 'NONE',  ( 161.1922820468853388, -1.999999999999974021, -19.40354224447947473 ) ) ;
#10576 = DIRECTION ( 'NONE',  ( -2.698458740408365879E-16, 1.000000000000000000, 0.000000000000000000 ) ) ;
#10577 = CARTESIAN_POINT ( 'NONE',  ( 164.5152310637605240, -1.999999999999971356, -28.60870317832789667 ) ) ;
#10578 = CARTESIAN_POINT ( 'NONE',  ( 151.1922820468854525, -10.00000000000000178, -28.06379628232387802 ) ) ;
#10579 = CARTESIAN_POINT ( 'NONE',  ( 11.45661370752365116, 9.343864103108954211, -15.86763743611193789 ) ) ;
#10580 = CARTESIAN_POINT ( 'NONE',  ( 26.39122182234759961, -2.132411660323914049, -15.07701415690354274 ) ) ;
#10581 = EDGE_CURVE ( 'NONE', #10720, #27442, #23618, .T. ) ;
#10582 = ORIENTED_EDGE ( 'NONE', *, *, #20369, .F. ) ;
#10583 = CARTESIAN_POINT ( 'NONE',  ( 172.7287565553229456, -4.999999999999970690, -33.50000000000000000 ) ) ;
#10584 = CARTESIAN_POINT ( 'NONE',  ( 148.6922820468854525, -1.999999999999976241, -35.24709285013155835 ) ) ;
#10585 = CARTESIAN_POINT ( 'NONE',  ( 147.0152310637606092, -10.00000000000000178, -24.27857615940569502 ) ) ;
#10586 = CARTESIAN_POINT ( 'NONE',  ( -2.000000000000032863, -3.464101615137743728, 8.673617379884035472E-16 ) ) ;
#10587 = AXIS2_PLACEMENT_3D ( 'NONE', #29538, #20607, #13597 ) ;
#10588 = DIRECTION ( 'NONE',  ( 0.3090169943749475623, 8.338696094058001131E-17, 0.9510565162951536422 ) ) ;
#10590 = ORIENTED_EDGE ( 'NONE', *, *, #27038, .T. ) ;
#10589 = CARTESIAN_POINT ( 'NONE',  ( 20.51249478307574847, 1.942573248051725709, -13.31196225760961838 ) ) ;
#10591 = ORIENTED_EDGE ( 'NONE', *, *, #7943, .F. ) ;
#10592 = CARTESIAN_POINT ( 'NONE',  ( 36.04859390953723874, -22.18451583373416014, -18.00000000000000000 ) ) ;
#10593 = CARTESIAN_POINT ( 'NONE',  ( 12.27691367651725862, 9.494620545951883983, -15.31068823849801319 ) ) ;
#10594 = AXIS2_PLACEMENT_3D ( 'NONE', #4042, #2369, #25542 ) ;
#10595 = CARTESIAN_POINT ( 'NONE',  ( 32.48283477683061449, -11.02614750807341260, -17.91093295056291979 ) ) ;
#10596 = CARTESIAN_POINT ( 'NONE',  ( 168.6922820468853956, -1.999999999999970468, -35.24709285013155835 ) ) ;
#10597 = CARTESIAN_POINT ( 'NONE',  ( 19.12501085131992085, -2.578449613843157184, -15.80510918775627438 ) ) ;
#10598 = CARTESIAN_POINT ( 'NONE',  ( 134.5152310637605808, -1.999999999999980460, -11.28819510263909187 ) ) ;
#10599 = CARTESIAN_POINT ( 'NONE',  ( 21.82606822486871323, 1.157895394498012154, -14.17951425939655508 ) ) ;
#10600 = ORIENTED_EDGE ( 'NONE', *, *, #11831, .F. ) ;
#10601 = EDGE_CURVE ( 'NONE', #5840, #4938, #23779, .T. ) ;
#10602 = DIRECTION ( 'NONE',  ( -1.000000000000000000, -2.891205793294689173E-16, 0.000000000000000000 ) ) ;
#10603 =( NAMED_UNIT ( * ) PLANE_ANGLE_UNIT ( ) SI_UNIT ( $, .RADIAN. ) );
#10604 = CARTESIAN_POINT ( 'NONE',  ( 23.86193934616450818, -4.638293873783104537, -19.03466029786466152 ) ) ;
#10605 = EDGE_CURVE ( 'NONE', #21255, #27873, #24526, .T. ) ;
#10606 = CARTESIAN_POINT ( 'NONE',  ( 24.13298513268436452, -7.720266465098472253, -12.91035621449759496 ) ) ;
#10607 = B_SPLINE_CURVE_WITH_KNOTS ( 'NONE', 3,
 ( #20380, #8486, #6210, #27147, #18094, #15502, #24833, #3924 ),
 .UNSPECIFIED., .F., .F.,
 ( 4, 2, 2, 4 ),
 ( 0.004673709593152139234, 0.005837709341827639065, 0.007001709090503138895, 0.009329708587854137689 ),
 .UNSPECIFIED. ) ;
#10608 = ORIENTED_EDGE ( 'NONE', *, *, #14689, .T. ) ;
#10609 = CARTESIAN_POINT ( 'NONE',  ( -4.000000000000020428, -6.928203230275511437, 0.000000000000000000 ) ) ;
#10610 = VECTOR ( 'NONE', #10158, 1000.000000000000000 ) ;
#10611 = DIRECTION ( 'NONE',  ( -2.698458740408365879E-16, 1.000000000000000000, 0.000000000000000000 ) ) ;
#10612 = ORIENTED_EDGE ( 'NONE', *, *, #8693, .T. ) ;
#10613 = LINE ( 'NONE', #17328, #27338 ) ;
#10614 = VECTOR ( 'NONE', #10406, 1000.000000000000000 ) ;
#10615 = PLANE ( 'NONE',  #27710 ) ;
#10616 = LINE ( 'NONE', #20220, #23129 ) ;
#10617 = LINE ( 'NONE', #29291, #25299 ) ;
#10618 = CARTESIAN_POINT ( 'NONE',  ( 29.60394739741320080, -6.827861936862228198, -14.22031441372854843 ) ) ;
#10619 = DIRECTION ( 'NONE',  ( 1.000000000000000000, 0.000000000000000000, 0.000000000000000000 ) ) ;
#10620 = EDGE_CURVE ( 'NONE', #20836, #6999, #22543, .T. ) ;
#10621 = CARTESIAN_POINT ( 'NONE',  ( 36.54859195715578579, -22.18450706271777406, -18.40832622446962930 ) ) ;
#10622 = PLANE ( 'NONE',  #9514 ) ;
#10623 = CARTESIAN_POINT ( 'NONE',  ( 9.917965570771830386, 16.40030059027150600, -16.50392256580263606 ) ) ;
#10624 = DIRECTION ( 'NONE',  ( 1.000000000000000000, 4.440892098500622217E-16, 0.000000000000000000 ) ) ;
#10625 = DIRECTION ( 'NONE',  ( -2.698458740408365879E-16, 1.000000000000000000, 0.000000000000000000 ) ) ;
#10626 = CARTESIAN_POINT ( 'NONE',  ( 9.661883061612440926, 16.25482663361732705, -21.33333333332589632 ) ) ;
#10627 = FACE_OUTER_BOUND ( 'NONE', #28163, .T. ) ;
#10628 = LINE ( 'NONE', #1188, #27674 ) ;
#10629 = CARTESIAN_POINT ( 'NONE',  ( 9.932908820165812003, 16.33176894372950727, -16.49774300651844072 ) ) ;
#10630 = EDGE_LOOP ( 'NONE', ( #18972, #27063, #17217, #5922 ) ) ;
#10631 = CARTESIAN_POINT ( 'NONE',  ( 22.04996626933243675, -5.000000000000011546, -67.86281818239412189 ) ) ;
#10632 = DIRECTION ( 'NONE',  ( 0.5877852522924731371, 0.000000000000000000, 0.8090169943749474513 ) ) ;
#10633 = VECTOR ( 'NONE', #28454, 1000.000000000000000 ) ;
#10634 = LINE ( 'NONE', #26850, #14144 ) ;
#10635 = ORIENTED_EDGE ( 'NONE', *, *, #21425, .F. ) ;
#10636 = VERTEX_POINT ( 'NONE', #5758 ) ;
#10637 = CARTESIAN_POINT ( 'NONE',  ( 13.38012098442259834, 7.626178612778168109, -15.70746696265163145 ) ) ;
#10638 = ORIENTED_EDGE ( 'NONE', *, *, #21482, .F. ) ;
#10639 = VECTOR ( 'NONE', #26860, 1000.000000000000000 ) ;
#10640 = CARTESIAN_POINT ( 'NONE',  ( 28.80153578082395427, -7.039779562103731791, -13.29052886957691371 ) ) ;
#10641 = CARTESIAN_POINT ( 'NONE',  ( 28.56881743257453721, -8.627791766613455593, -12.78522491232925873 ) ) ;
#10642 = LINE ( 'NONE', #6072, #21381 ) ;
#10643 = CARTESIAN_POINT ( 'NONE',  ( 142.0152310637605240, -1.999999999999978684, -0.06116980274991495881 ) ) ;
#10644 = CARTESIAN_POINT ( 'NONE',  ( 0.000000000000000000, 0.000000000000000000, 18.00000000000000000 ) ) ;
#10645 = ORIENTED_EDGE ( 'NONE', *, *, #22203, .T. ) ;
#10646 = ORIENTED_EDGE ( 'NONE', *, *, #30124, .T. ) ;
#10647 = CARTESIAN_POINT ( 'NONE',  ( 152.0152310637605240, -10.00000000000000178, -6.958068083716895558 ) ) ;
#10648 = EDGE_LOOP ( 'NONE', ( #22250, #16734, #1383, #3450 ) ) ;
#10649 = DIRECTION ( 'NONE',  ( -0.9510565162951536422, 0.000000000000000000, -0.3090169943749472292 ) ) ;
#10650 = DIRECTION ( 'NONE',  ( 1.110223024625156540E-16, 2.995891024602366092E-32, 1.000000000000000000 ) ) ;
#10651 = CYLINDRICAL_SURFACE ( 'NONE', #4570, 3.000000000000002665 ) ;
#10652 = CARTESIAN_POINT ( 'NONE',  ( 13.11546866977305825, 8.567317423965196355, -15.91839467484043880 ) ) ;
#10653 = EDGE_CURVE ( 'NONE', #28202, #16318, #26683, .T. ) ;
#10654 = EDGE_CURVE ( 'NONE', #15239, #10099, #22081, .T. ) ;
#10655 = CARTESIAN_POINT ( 'NONE',  ( 33.25502826659400313, -11.79853993747392771, -18.08863679259532731 ) ) ;
#10656 = VECTOR ( 'NONE', #5102, 1000.000000000000000 ) ;
#10657 = ORIENTED_EDGE ( 'NONE', *, *, #4609, .T. ) ;
#10658 = CARTESIAN_POINT ( 'NONE',  ( 9.112637166705713554, 16.18088265059586561, -17.05468042929993189 ) ) ;
#10659 = EDGE_CURVE ( 'NONE', #15781, #1679, #12670, .T. ) ;
#10660 = EDGE_LOOP ( 'NONE', ( #2164, #18627, #1270, #4368, #4968 ) ) ;
#10661 = EDGE_CURVE ( 'NONE', #19491, #5542, #6124, .T. ) ;
#10662 = CARTESIAN_POINT ( 'NONE',  ( 25.36810815240369621, -0.9165050883202133791, -18.11329069065276443 ) ) ;
#10663 = CARTESIAN_POINT ( 'NONE',  ( 13.08618951557147803, 9.612344561400664844, -15.94173553134588595 ) ) ;
#10664 = FACE_BOUND ( 'NONE', #3017, .T. ) ;
#10665 = CIRCLE ( 'NONE', #11166, 4.000000000000004441 ) ;
#10666 = ORIENTED_EDGE ( 'NONE', *, *, #11412, .F. ) ;
#10667 = VECTOR ( 'NONE', #8330, 1000.000000000000000 ) ;
#10668 = ORIENTED_EDGE ( 'NONE', *, *, #2111, .T. ) ;
#10669 = FACE_OUTER_BOUND ( 'NONE', #17032, .T. ) ;
#10670 = CARTESIAN_POINT ( 'NONE',  ( 11.49350937636955372, 9.187954247928445284, -15.85136552863131421 ) ) ;
#10671 = CARTESIAN_POINT ( 'NONE',  ( 164.7287565553229456, -1.999999999999971356, -25.16025403784440329 ) ) ;
#10672 = ORIENTED_EDGE ( 'NONE', *, *, #17996, .T. ) ;
#10673 = PLANE ( 'NONE',  #826 ) ;
#10674 = ORIENTED_EDGE ( 'NONE', *, *, #11570, .F. ) ;
#10675 = CARTESIAN_POINT ( 'NONE',  ( 9.661883061612440926, 16.25482663361732705, -17.97192418671890835 ) ) ;
#10676 = ORIENTED_EDGE ( 'NONE', *, *, #23422, .F. ) ;
#10677 = CARTESIAN_POINT ( 'NONE',  ( 13.34169928452473819, 6.621333031661079005, -16.53230918748570488 ) ) ;
#10678 = CARTESIAN_POINT ( 'NONE',  ( 17.03934835405440751, -0.5873649402599611102, -16.44458879923593742 ) ) ;
#10679 = CARTESIAN_POINT ( 'NONE',  ( 133.6922820468854241, -1.999999999999981348, -32.39392330124607611 ) ) ;
#10680 = EDGE_LOOP ( 'NONE', ( #6706, #6211, #3623 ) ) ;
#10681 = CARTESIAN_POINT ( 'NONE',  ( 36.54859390953724585, -22.18451583373416014, -16.11276402859391865 ) ) ;
#10682 = VECTOR ( 'NONE', #3835, 1000.000000000000000 ) ;
#10683 = CARTESIAN_POINT ( 'NONE',  ( 18.76632379254337835, 6.868107169226369102, -19.55161205380106892 ) ) ;
#10684 = ORIENTED_EDGE ( 'NONE', *, *, #14542, .F. ) ;
#10685 = MECHANICAL_DESIGN_GEOMETRIC_PRESENTATION_REPRESENTATION (  '', ( #19945 ), #25820 ) ;
#10686 = DIRECTION ( 'NONE',  ( 0.9510565162951536422, 0.000000000000000000, -0.3090169943749475623 ) ) ;
#10687 = LINE ( 'NONE', #24286, #22063 ) ;
#10688 = ORIENTED_EDGE ( 'NONE', *, *, #3283, .T. ) ;
#10689 = CARTESIAN_POINT ( 'NONE',  ( 169.7287565553228887, -1.999999999999970912, -7.839745962155603820 ) ) ;
#10690 = ADVANCED_FACE ( 'NONE', ( #1335 ), #1641, .T. ) ;
#10691 = CARTESIAN_POINT ( 'NONE',  ( 33.96943610671532809, -15.09019632882451134, -19.88060704079178720 ) ) ;
#10692 = PLANE ( 'NONE',  #23366 ) ;
#10693 = ORIENTED_EDGE ( 'NONE', *, *, #20922, .F. ) ;
#10694 = ADVANCED_FACE ( 'NONE', ( #24229 ), #29617, .T. ) ;
#10695 = EDGE_CURVE ( 'NONE', #9455, #8020, #8337, .T. ) ;
#10696 = CARTESIAN_POINT ( 'NONE',  ( 2.500000000000000444, 2.357898499370430834, -3.469446951953614189E-15 ) ) ;
#10697 = EDGE_CURVE ( 'NONE', #26624, #28890, #19934, .T. ) ;
#10698 = CARTESIAN_POINT ( 'NONE',  ( 12.46291758456249354, 9.612344561400664844, -15.15973035232449462 ) ) ;
#10699 = AXIS2_PLACEMENT_3D ( 'NONE', #14620, #11579, #14014 ) ;
#10700 = DIRECTION ( 'NONE',  ( 1.000000000000000000, 0.000000000000000000, 0.000000000000000000 ) ) ;
#10701 = ORIENTED_EDGE ( 'NONE', *, *, #3749, .F. ) ;
#10702 = CARTESIAN_POINT ( 'NONE',  ( 142.0152310637605808, -1.999999999999978018, -34.70218595412750773 ) ) ;
#10703 = VERTEX_POINT ( 'NONE', #28992 ) ;
#10704 = CARTESIAN_POINT ( 'NONE',  ( 10.74080116101666427, 8.781381604732478863, -16.37623182050610993 ) ) ;
#10705 = FACE_OUTER_BOUND ( 'NONE', #19796, .T. ) ;
#10706 = CARTESIAN_POINT ( 'NONE',  ( 154.7287565553229456, -1.999999999999974909, -7.839745962155603820 ) ) ;
#10707 = CARTESIAN_POINT ( 'NONE',  ( 20.14013621308192015, -5.000000000000012434, -61.98496565946941672 ) ) ;
#10708 = ORIENTED_EDGE ( 'NONE', *, *, #27556, .T. ) ;
#10709 = CARTESIAN_POINT ( 'NONE',  ( 12.86826794643883609, 9.516041646402381815, -16.11542282846662388 ) ) ;
#10710 = CARTESIAN_POINT ( 'NONE',  ( 36.27242973171742335, -19.94385647102418702, -19.46417027601260230 ) ) ;
#10711 = CARTESIAN_POINT ( 'NONE',  ( 21.79935899731381710, -1.430375723040585356, -13.25318265510616733 ) ) ;
#10712 = VERTEX_POINT ( 'NONE', #3770 ) ;
#10713 = PLANE ( 'NONE',  #4267 ) ;
#10714 = CARTESIAN_POINT ( 'NONE',  ( -31.74999999999995737, 0.000000000000000000, 4.250000000000000000 ) ) ;
#10715 = DIRECTION ( 'NONE',  ( -2.908569913943825554E-16, 1.000000000000000000, -0.000000000000000000 ) ) ;
#10716 = FILL_AREA_STYLE_COLOUR ( '', #5853 ) ;
#10717 = CARTESIAN_POINT ( 'NONE',  ( 26.06583011202948441, -9.749651170145462231, -12.94692625511877182 ) ) ;
#10718 = CARTESIAN_POINT ( 'NONE',  ( 20.52698940127687877, 5.222567878441341627, -18.38034891569893503 ) ) ;
#10719 = PRODUCT_DEFINITION_FORMATION_WITH_SPECIFIED_SOURCE ( 'ANY', '', #22019, .NOT_KNOWN. ) ;
#10720 = VERTEX_POINT ( 'NONE', #3328 ) ;
#10721 = CARTESIAN_POINT ( 'NONE',  ( 157.2287565553229456, -4.999999999999976019, -3.509618943233400401 ) ) ;
#10722 = AXIS2_PLACEMENT_3D ( 'NONE', #29770, #22690, #1946 ) ;
#10724 = CARTESIAN_POINT ( 'NONE',  ( 154.7287565553229172, -1.999999999999975353, 0.8205080756887930260 ) ) ;
#10723 = VECTOR ( 'NONE', #19131, 1000.000000000000000 ) ;
#10725 = VECTOR ( 'NONE', #12153, 1000.000000000000000 ) ;
#10726 = CARTESIAN_POINT ( 'NONE',  ( 132.2287565553230024, -1.999999999999981348, -3.509618943233403510 ) ) ;
#10727 = CYLINDRICAL_SURFACE ( 'NONE', #25681, 5.000000000000000000 ) ;
#10728 = DIRECTION ( 'NONE',  ( 0.3090169943749472292, 8.338696094057992503E-17, -0.9510565162951536422 ) ) ;
#10729 = ADVANCED_FACE ( 'NONE', ( #10464 ), #12607, .T. ) ;
#10730 = EDGE_CURVE ( 'NONE', #29043, #24264, #12634, .T. ) ;
#10731 = CARTESIAN_POINT ( 'NONE',  ( 25.00000000000000000, 0.000000000000000000, 2.055000000000000160 ) ) ;
#10732 = CARTESIAN_POINT ( 'NONE',  ( 11.22518019566232716, 9.085373951847735441, -17.24107067304604257 ) ) ;
#10733 = EDGE_CURVE ( 'NONE', #2968, #1559, #20089, .T. ) ;
#10734 = CARTESIAN_POINT ( 'NONE',  ( 10.33811693838771717, 18.38618951776012267, -17.92981046679734547 ) ) ;
#10735 = ADVANCED_FACE ( 'NONE', ( #6208 ), #8484, .T. ) ;
#10737 = VECTOR ( 'NONE', #11153, 1000.000000000000000 ) ;
#10736 = CARTESIAN_POINT ( 'NONE',  ( 26.06583011202948441, -9.749651170145462231, -12.94692625511877182 ) ) ;
#10738 = ORIENTED_EDGE ( 'NONE', *, *, #22797, .T. ) ;
#10739 = DIRECTION ( 'NONE',  ( 0.3090169943749472292, 8.338696094057992503E-17, -0.9510565162951536422 ) ) ;
#10740 = DIRECTION ( 'NONE',  ( -0.9510565162951536422, 0.000000000000000000, -0.3090169943749472292 ) ) ;
#10741 = ORIENTED_EDGE ( 'NONE', *, *, #12338, .T. ) ;
#10742 = VECTOR ( 'NONE', #4775, 1000.000000000000000 ) ;
#10743 = CARTESIAN_POINT ( 'NONE',  ( 9.907423389235603395, 16.44864837861227969, -16.50891839478055090 ) ) ;
#10744 = FACE_OUTER_BOUND ( 'NONE', #2517, .T. ) ;
#10745 = CARTESIAN_POINT ( 'NONE',  ( 63.44486372867152824, 109.8897274573438096, -15.00000000000000000 ) ) ;
#10746 = CARTESIAN_POINT ( 'NONE',  ( 25.55230692589818631, -0.5649882819070038975, -17.32853901032857280 ) ) ;
#10747 = VERTEX_POINT ( 'NONE', #8178 ) ;
#10748 = CARTESIAN_POINT ( 'NONE',  ( 172.0152310637604103, -4.999999999999970690, 1.702185954127501066 ) ) ;
#10749 = CARTESIAN_POINT ( 'NONE',  ( 12.01759036229752553, 10.68391031264169122, -15.41792755180196473 ) ) ;
#10750 = CIRCLE ( 'NONE', #17557, 7.000000000000006217 ) ;
#10751 = CARTESIAN_POINT ( 'NONE',  ( 32.68951927270060764, -11.07419627511998605, -18.48540492261787449 ) ) ;
#10752 = CARTESIAN_POINT ( 'NONE',  ( -4.000000000000010658, -2.309401076758525573, -0.3572655899081716435 ) ) ;
#10753 = CARTESIAN_POINT ( 'NONE',  ( 23.84106988684860440, -4.080291168153947545, -13.50610408985603250 ) ) ;
#10754 = DIRECTION ( 'NONE',  ( -1.000000000000000000, 0.000000000000000000, 0.000000000000000000 ) ) ;
#10755 = CARTESIAN_POINT ( 'NONE',  ( 15.57379856253263206, 2.175854586521385858, -15.33309735461106094 ) ) ;
#10756 = VERTEX_POINT ( 'NONE', #17490 ) ;
#10757 = CARTESIAN_POINT ( 'NONE',  ( 144.7287565553230024, -1.999999999999977573, -7.839745962155603820 ) ) ;
#10758 = CARTESIAN_POINT ( 'NONE',  ( 14.73435313093308174, 9.569269045654692718, -13.91804818168885305 ) ) ;
#10759 = CARTESIAN_POINT ( 'NONE',  ( 21.36789492492977871, -4.378045371801569274, -13.15753336270543095 ) ) ;
#10760 = ORIENTED_EDGE ( 'NONE', *, *, #11110, .T. ) ;
#10761 = AXIS2_PLACEMENT_3D ( 'NONE', #7001, #2881, #23320 ) ;
#10762 = CARTESIAN_POINT ( 'NONE',  ( 29.90031526554274777, -7.862644070287768905, -16.42500436498598049 ) ) ;
#10763 = VECTOR ( 'NONE', #1259, 1000.000000000000000 ) ;
#10764 = VERTEX_POINT ( 'NONE', #26841 ) ;
#10765 = PLANE ( 'NONE',  #2128 ) ;
#10766 = PRESENTATION_LAYER_ASSIGNMENT (  '', '', ( #21489 ) ) ;
#10767 = DIRECTION ( 'NONE',  ( 1.000000000000000000, 2.698458740408365879E-16, -1.110223024625156540E-16 ) ) ;
#10768 = CARTESIAN_POINT ( 'NONE',  ( 139.5152310637606092, -10.00000000000000533, -19.94844914048349338 ) ) ;
#10769 = EDGE_CURVE ( 'NONE', #14522, #11598, #8550, .T. ) ;
#10770 = CARTESIAN_POINT ( 'NONE',  ( 177.2287565553228887, -9.999999999999994671, -20.83012701892220520 ) ) ;
#10771 = EDGE_CURVE ( 'NONE', #4670, #6014, #13803, .T. ) ;
#10772 = CARTESIAN_POINT ( 'NONE',  ( 420.0000000000002274, 41.64101615137744972, 12.00000000000000178 ) ) ;
#10773 = EDGE_CURVE ( 'NONE', #26056, #14986, #29060, .T. ) ;
#10774 = CARTESIAN_POINT ( 'NONE',  ( 24.88525782559502630, -5.606924519715485111, -13.99218633471889817 ) ) ;
#10775 = CARTESIAN_POINT ( 'NONE',  ( 85.61150514570974224, -4.999999999999993783, 62.20039937490791715 ) ) ;
#10776 = CARTESIAN_POINT ( 'NONE',  ( 32.45862320860160821, -9.597537451891041016, -17.61229109800368064 ) ) ;
#10777 = FACE_OUTER_BOUND ( 'NONE', #15549, .T. ) ;
#10778 = CARTESIAN_POINT ( 'NONE',  ( 9.932908820165812003, 16.33176894372950727, -16.49774300651844072 ) ) ;
#10779 = DIRECTION ( 'NONE',  ( 0.9510565162951536422, 0.000000000000000000, -0.3090169943749475623 ) ) ;
#10780 = DIRECTION ( 'NONE',  ( -0.9510565162951536422, -2.566386769018988323E-16, 0.3090169943749475623 ) ) ;
#10781 = CARTESIAN_POINT ( 'NONE',  ( 13.12468173219994760, 8.571325198882655982, -15.91105655537220009 ) ) ;
#10782 = CARTESIAN_POINT ( 'NONE',  ( 156.1922820468853672, -1.999999999999974465, -10.74328820663507678 ) ) ;
#10783 = DIRECTION ( 'NONE',  ( 1.000000000000000000, 0.000000000000000000, 0.000000000000000000 ) ) ;
#10784 = VECTOR ( 'NONE', #20228, 1000.000000000000000 ) ;
#10785 = CARTESIAN_POINT ( 'NONE',  ( 9.920751600319857033, 16.38752350362809551, -16.50277044458016107 ) ) ;
#10786 = VERTEX_POINT ( 'NONE', #1944 ) ;
#10787 = VECTOR ( 'NONE', #5885, 1000.000000000000000 ) ;
#10788 = CARTESIAN_POINT ( 'NONE',  ( 158.6922820468853956, -4.999999999999974243, -23.73366926340167637 ) ) ;
#10789 = DIRECTION ( 'NONE',  ( 0.9510565162951535312, 2.566386769018988816E-16, -0.3090169943749475623 ) ) ;
#10790 = PLANE ( 'NONE',  #21956 ) ;
#10791 = ORIENTED_EDGE ( 'NONE', *, *, #20768, .T. ) ;
#10792 = ORIENTED_EDGE ( 'NONE', *, *, #13563, .T. ) ;
#10793 = CARTESIAN_POINT ( 'NONE',  ( 15.26446397285951839, 8.458903494591371697, -14.20561233965910297 ) ) ;
#10794 = CARTESIAN_POINT ( 'NONE',  ( 31.83585693452864973, -10.27807049784803972, -18.08404909334234745 ) ) ;
#10795 = CARTESIAN_POINT ( 'NONE',  ( 32.00807787192805876, -10.01600718589171990, -13.21854031764240389 ) ) ;
#10796 = CARTESIAN_POINT ( 'NONE',  ( 24.16496757332932788, -10.42823604606268617, -16.34834267607407909 ) ) ;
#10797 = DIRECTION ( 'NONE',  ( -1.110223024625156540E-16, 0.000000000000000000, -1.000000000000000000 ) ) ;
#10798 = DIRECTION ( 'NONE',  ( 0.9510565162951536422, 0.000000000000000000, -0.3090169943749475623 ) ) ;
#10799 = CARTESIAN_POINT ( 'NONE',  ( 147.2287565553229740, -4.999999999999978684, -3.509618943233400401 ) ) ;
#10800 = EDGE_CURVE ( 'NONE', #7135, #8074, #25425, .T. ) ;
#10801 = EDGE_LOOP ( 'NONE', ( #6149, #14297, #16292, #3499 ) ) ;
#10802 = CARTESIAN_POINT ( 'NONE',  ( 114.3941076083291648, -4.999999999999985789, -83.11218413067275890 ) ) ;
#10803 = VECTOR ( 'NONE', #11040, 1000.000000000000000 ) ;
#10804 = DIRECTION ( 'NONE',  ( 0.5877852522924731371, 0.000000000000000000, 0.8090169943749474513 ) ) ;
#10805 = CARTESIAN_POINT ( 'NONE',  ( 13.23272240178861381, 8.619070305187777947, -15.82494623455082916 ) ) ;
#10806 = CARTESIAN_POINT ( 'NONE',  ( 33.63214571818804188, -11.07540017893869866, -16.92567501773416794 ) ) ;
#10807 = VERTEX_POINT ( 'NONE', #8925 ) ;
#10808 = CARTESIAN_POINT ( 'NONE',  ( 9.111869836743295537, 16.18440172361536611, -17.05500387803421702 ) ) ;
#10809 = VERTEX_POINT ( 'NONE', #2240 ) ;
#10810 = VECTOR ( 'NONE', #4613, 1000.000000000000000 ) ;
#10811 = CARTESIAN_POINT ( 'NONE',  ( 25.07290406138036687, -9.006318079059196791, -17.79994936451110732 ) ) ;
#10812 = CARTESIAN_POINT ( 'NONE',  ( 12.92285173585636215, 9.540162674316999158, -16.07191862488577527 ) ) ;
#10813 = FACE_BOUND ( 'NONE', #17536, .T. ) ;
#10814 = ORIENTED_EDGE ( 'NONE', *, *, #26789, .T. ) ;
#10815 = DIRECTION ( 'NONE',  ( -2.698458740408365879E-16, 1.000000000000000000, 0.000000000000000000 ) ) ;
#10816 = CARTESIAN_POINT ( 'NONE',  ( 11.47748818427356987, 9.248962635895034978, -15.85894168489154765 ) ) ;
#10818 = CARTESIAN_POINT ( 'NONE',  ( 134.5152310637605524, -4.999999999999981348, -1.493419066897600538E-14 ) ) ;
#10817 = VECTOR ( 'NONE', #2632, 1000.000000000000000 ) ;
#10819 = DIRECTION ( 'NONE',  ( -1.000000000000000000, 0.000000000000000000, -0.000000000000000000 ) ) ;
#10820 = ORIENTED_EDGE ( 'NONE', *, *, #18340, .T. ) ;
#10821 = CARTESIAN_POINT ( 'NONE',  ( 9.661883064511089358, 16.25482662032373327, -17.91571053624716470 ) ) ;
#10822 = CARTESIAN_POINT ( 'NONE',  ( 19.51424001318473245, 7.885341048999412017, -19.79681821819610832 ) ) ;
#10823 = CARTESIAN_POINT ( 'NONE',  ( 16.54285080251403173, 3.669380853427548939, -13.47387114519368012 ) ) ;
#10824 = CYLINDRICAL_SURFACE ( 'NONE', #17451, 4.000000000000000000 ) ;
#10825 = EDGE_LOOP ( 'NONE', ( #4702, #4921, #23581, #6214 ) ) ;
#10826 = CARTESIAN_POINT ( 'NONE',  ( 35.91774987194125401, -19.35046774019819438, -20.39927477693754554 ) ) ;
#10827 = EDGE_CURVE ( 'NONE', #28891, #5806, #2093, .T. ) ;
#10828 = EDGE_CURVE ( 'NONE', #20539, #2343, #30058, .T. ) ;
#10829 = CARTESIAN_POINT ( 'NONE',  ( 19.25770813156441008, -2.543370271471735222, -15.40753146551623587 ) ) ;
#10830 = AXIS2_PLACEMENT_3D ( 'NONE', #8841, #18001, #6874 ) ;
#10831 = CARTESIAN_POINT ( 'NONE',  ( 0.000000000000000000, 0.000000000000000000, 0.000000000000000000 ) ) ;
#10832 = PLANE ( 'NONE',  #123 ) ;
#10833 = VECTOR ( 'NONE', #450, 1000.000000000000000 ) ;
#10834 = ORIENTED_EDGE ( 'NONE', *, *, #12627, .T. ) ;
#10835 = CARTESIAN_POINT ( 'NONE',  ( 154.7287565553229172, -10.00000000000000178, 0.8205080756887930260 ) ) ;
#10836 = CARTESIAN_POINT ( 'NONE',  ( 33.44337896868773186, -12.72690026786775341, -19.72159258799634074 ) ) ;
#10837 = DIRECTION ( 'NONE',  ( -0.5000000000000056621, -0.8660254037844354880, 0.000000000000000000 ) ) ;
#10838 = ORIENTED_EDGE ( 'NONE', *, *, #10605, .F. ) ;
#10839 = VERTEX_POINT ( 'NONE', #25125 ) ;
#10840 = DIRECTION ( 'NONE',  ( -2.698458740408365879E-16, 1.000000000000000000, 0.000000000000000000 ) ) ;
#10841 = CARTESIAN_POINT ( 'NONE',  ( 12.24562038388194551, 9.516309650702005740, -15.33292062045688908 ) ) ;
#10842 = CARTESIAN_POINT ( 'NONE',  ( 34.74206752880779447, -19.56122003402509080, -21.15647653254228189 ) ) ;
#10843 = EDGE_LOOP ( 'NONE', ( #20002, #26411, #24954, #11738 ) ) ;
#10844 = DIRECTION ( 'NONE',  ( 1.000000000000000000, 4.440892098500622217E-16, 0.000000000000000000 ) ) ;
#10845 = CARTESIAN_POINT ( 'NONE',  ( 10.66743590522492369, 9.050377445005224786, -16.41171652237351353 ) ) ;
#10846 = DIRECTION ( 'NONE',  ( 1.110223024625156540E-16, 2.995891024602366092E-32, 1.000000000000000000 ) ) ;
#10847 = VERTEX_POINT ( 'NONE', #11511 ) ;
#10848 = LINE ( 'NONE', #1569, #1796 ) ;
#10849 = ORIENTED_EDGE ( 'NONE', *, *, #12763, .T. ) ;
#10850 = CARTESIAN_POINT ( 'NONE',  ( 10.35864918915110877, 16.97212501191939538, -21.33333333332589277 ) ) ;
#10851 = CARTESIAN_POINT ( 'NONE',  ( 34.18187006836440389, -11.68445768601494628, -19.79758194388510972 ) ) ;
#10852 = CARTESIAN_POINT ( 'NONE',  ( 21.57856661146780652, -4.666631351218505586, -18.28211233923166645 ) ) ;
#10853 = ORIENTED_EDGE ( 'NONE', *, *, #11950, .F. ) ;
#10854 = ORIENTED_EDGE ( 'NONE', *, *, #16143, .F. ) ;
#10855 = EDGE_LOOP ( 'NONE', ( #286, #1060, #27697, #17233, #15159 ) ) ;
#10856 = VECTOR ( 'NONE', #16124, 1000.000000000000000 ) ;
#10857 = EDGE_LOOP ( 'NONE', ( #17434, #28235, #12748, #7336, #19800, #5034 ) ) ;
#10858 = CARTESIAN_POINT ( 'NONE',  ( 168.6922820468853388, -9.999999999999996447, -15.07341522555727664 ) ) ;
#10859 = ORIENTED_EDGE ( 'NONE', *, *, #15893, .T. ) ;
#10860 = SURFACE_STYLE_USAGE ( .BOTH. , #27542 ) ;
#10861 = EDGE_CURVE ( 'NONE', #1407, #7486, #9219, .T. ) ;
#10862 = CARTESIAN_POINT ( 'NONE',  ( 28.02603357813017482, -6.678172375388682802, -19.11289830413424440 ) ) ;
#10863 = EDGE_CURVE ( 'NONE', #19955, #17748, #4070, .T. ) ;
#10864 = CARTESIAN_POINT ( 'NONE',  ( 27.32111546295355708, -6.651148440249742499, -13.76656720552121982 ) ) ;
#10865 = EDGE_CURVE ( 'NONE', #26865, #28553, #15852, .T. ) ;
#10866 = VERTEX_POINT ( 'NONE', #18547 ) ;
#10867 = CARTESIAN_POINT ( 'NONE',  ( 144.7287565553230309, -1.999999999999977129, -33.82050807568879947 ) ) ;
#10868 = PLANE ( 'NONE',  #26795 ) ;
#10869 = LINE ( 'NONE', #8283, #27511 ) ;
#10870 = CARTESIAN_POINT ( 'NONE',  ( 0.000000000000000000, 0.000000000000000000, 23.00000000000000000 ) ) ;
#10871 = LINE ( 'NONE', #20181, #10190 ) ;
#10872 = DIRECTION ( 'NONE',  ( 1.000000000000000000, 0.000000000000000000, 0.000000000000000000 ) ) ;
#10873 = VECTOR ( 'NONE', #1435, 1000.000000000000000 ) ;
#10874 = CARTESIAN_POINT ( 'NONE',  ( 11.22423757029256741, 9.089670537749404033, -17.24146249637195183 ) ) ;
#10875 = CARTESIAN_POINT ( 'NONE',  ( 12.49271550807400999, 8.567542729147559655, -15.13597632865050535 ) ) ;
#10876 = CARTESIAN_POINT ( 'NONE',  ( 31.37220973900873489, -11.08107799475175348, -13.94606079199652982 ) ) ;
#10877 = CARTESIAN_POINT ( 'NONE',  ( -13.00000000000001243, 55.00000000000000711, 23.00000000000000000 ) ) ;
#10878 = CARTESIAN_POINT ( 'NONE',  ( 172.7287565553229740, -84.33034373659253902, -33.50000000000000000 ) ) ;
#10879 = ORIENTED_EDGE ( 'NONE', *, *, #28317, .F. ) ;
#10880 = DIRECTION ( 'NONE',  ( -0.000000000000000000, -0.000000000000000000, -1.000000000000000000 ) ) ;
#10881 = CARTESIAN_POINT ( 'NONE',  ( 174.5152310637604671, -1.999999999999968914, -30.37205893520531319 ) ) ;
#10882 = DIRECTION ( 'NONE',  ( 0.000000000000000000, 0.000000000000000000, 1.000000000000000000 ) ) ;
#10883 = CARTESIAN_POINT ( 'NONE',  ( 137.0152310637605808, -1.999999999999980016, 1.702185954127501066 ) ) ;
#10885 = EDGE_LOOP ( 'NONE', ( #15823, #12310, #12168, #17902, #4520 ) ) ;
#10884 = CARTESIAN_POINT ( 'NONE',  ( 22.51149892830068211, -1.106640851078940502, -13.23823320067571885 ) ) ;
#10886 = EDGE_LOOP ( 'NONE', ( #14250, #26922, #26625, #15633, #17652 ) ) ;
#10887 = DIRECTION ( 'NONE',  ( -0.5877852522924731371, 0.000000000000000000, 0.8090169943749474513 ) ) ;
#10888 = CARTESIAN_POINT ( 'NONE',  ( 12.24670349824113380, 9.516721811805902931, -15.33206243003379754 ) ) ;
#10889 = ADVANCED_FACE ( 'NONE', ( #20827 ), #18396, .T. ) ;
#10890 = CONICAL_SURFACE ( 'NONE', #13309, 4.000000000000003553, 1.047197551196597853 ) ;
#10891 = PLANE ( 'NONE',  #30089 ) ;
#10892 = CARTESIAN_POINT ( 'NONE',  ( 11.50000000000008171, 17.32050807568872486, -23.00000000000000000 ) ) ;
#10893 = CARTESIAN_POINT ( 'NONE',  ( 27.83100014064079275, -5.545984359997562230, -15.13782040115233052 ) ) ;
#10894 = LINE ( 'NONE', #26079, #23768 ) ;
#10895 = CARTESIAN_POINT ( 'NONE',  ( 23.38119176934044674, -2.968156504308268495, -14.25447959695224043 ) ) ;
#10896 = ORIENTED_EDGE ( 'NONE', *, *, #14577, .T. ) ;
#10897 = CARTESIAN_POINT ( 'NONE',  ( 0.000000000000000000, 0.000000000000000000, 0.000000000000000000 ) ) ;
#10898 =( NAMED_UNIT ( * ) SI_UNIT ( $, .STERADIAN. ) SOLID_ANGLE_UNIT ( ) );
#10899 = CARTESIAN_POINT ( 'NONE',  ( 32.15747877504752950, -11.00374777879112642, -13.30332049327740052 ) ) ;
#10900 = CARTESIAN_POINT ( 'NONE',  ( 25.10166869626759123, -5.595937160916529152, -20.34551573546397307 ) ) ;
#10901 = ADVANCED_FACE ( 'NONE', ( #25563 ), #4364, .T. ) ;
#10902 = VECTOR ( 'NONE', #15066, 1000.000000000000000 ) ;
#10903 = EDGE_CURVE ( 'NONE', #15583, #11088, #15949, .T. ) ;
#10904 = EDGE_CURVE ( 'NONE', #15699, #19168, #13951, .T. ) ;
#10905 = EDGE_CURVE ( 'NONE', #10978, #19490, #3222, .T. ) ;
#10906 = VERTEX_POINT ( 'NONE', #27308 ) ;
#10907 = ORIENTED_EDGE ( 'NONE', *, *, #20924, .F. ) ;
#10908 = CARTESIAN_POINT ( 'NONE',  ( 24.78692427941192733, -9.284778175067517125, -17.23615439686343720 ) ) ;
#10909 = CARTESIAN_POINT ( 'NONE',  ( 152.0152310637605808, -10.00000000000000000, -34.70218595412750773 ) ) ;
#10910 = CARTESIAN_POINT ( 'NONE',  ( 172.0152310637604103, -4.999999999999970690, -8.721423840594312082 ) ) ;
#10911 = CARTESIAN_POINT ( 'NONE',  ( 0.000000000000000000, 0.000000000000000000, 1.699999999999996625 ) ) ;
#10912 = LINE ( 'NONE', #8768, #17762 ) ;
#10913 = CARTESIAN_POINT ( 'NONE',  ( 9.641350810849047548, 17.66889113945805789, -21.33333333332589277 ) ) ;
#10914 = CARTESIAN_POINT ( 'NONE',  ( 23.39779239333391914, -5.936415184958717894, -17.60678703246490429 ) ) ;
#10915 = CARTESIAN_POINT ( 'NONE',  ( 18.63710449947919301, 3.826706299981984305, -14.11708861520305192 ) ) ;
#10916 = CARTESIAN_POINT ( 'NONE',  ( 34.40782828833705054, -13.56718989277036691, -20.98518325316450372 ) ) ;
#10917 = CARTESIAN_POINT ( 'NONE',  ( 2.000000000000003553, -3.464101615137736623, 8.673617379884035472E-16 ) ) ;
#10918 = CARTESIAN_POINT ( 'NONE',  ( 11.48890098693651396, 9.204103201752445784, -15.85365151319587440 ) ) ;
#10919 = VECTOR ( 'NONE', #4394, 1000.000000000000000 ) ;
#10920 = CARTESIAN_POINT ( 'NONE',  ( 19.58373008303804141, -5.000000000000012434, -60.27252367304998870 ) ) ;
#10921 = DIRECTION ( 'NONE',  ( 1.000000000000000000, 2.698458740408365879E-16, -1.110223024625156540E-16 ) ) ;
#10922 = CARTESIAN_POINT ( 'NONE',  ( 9.661883061612440926, 16.25482663361732705, -17.98596209335946128 ) ) ;
#10923 = LINE ( 'NONE', #20231, #27357 ) ;
#10924 = CARTESIAN_POINT ( 'NONE',  ( 163.6922820468853672, -1.999999999999971800, -23.73366926340167637 ) ) ;
#10925 = CARTESIAN_POINT ( 'NONE',  ( 12.50396148805030627, 8.572452836447732594, -15.12701763676990119 ) ) ;
#10926 = VERTEX_POINT ( 'NONE', #13364 ) ;
#10927 = FACE_OUTER_BOUND ( 'NONE', #9876, .T. ) ;
#10928 = LINE ( 'NONE', #30068, #18565 ) ;
#10929 = CARTESIAN_POINT ( 'NONE',  ( 144.7287565553230309, -10.00000000000000355, -25.16025403784439973 ) ) ;
#10930 = VECTOR ( 'NONE', #16510, 1000.000000000000000 ) ;
#10931 = ORIENTED_EDGE ( 'NONE', *, *, #17913, .F. ) ;
#10932 = CARTESIAN_POINT ( 'NONE',  ( 8.944584683310379702, 16.95159276115599667, -17.97192418671890835 ) ) ;
#10933 = CARTESIAN_POINT ( 'NONE',  ( 36.54859390953724585, -23.18451583373416014, -18.19919658220850422 ) ) ;
#10934 = CARTESIAN_POINT ( 'NONE',  ( 20.90484242567171691, 8.469164366756103846, -17.19731680296963106 ) ) ;
#10935 = EDGE_CURVE ( 'NONE', #6165, #14559, #15656, .T. ) ;
#10936 = CARTESIAN_POINT ( 'NONE',  ( 22.24201797625671517, -7.474445146391827777, -15.38054711335415803 ) ) ;
#10937 = DIRECTION ( 'NONE',  ( -0.8090169943749474513, -2.183098979609982436E-16, -0.5877852522924731371 ) ) ;
#10938 = CARTESIAN_POINT ( 'NONE',  ( 137.2287565553230309, -10.00000000000000533, -20.83012701892220164 ) ) ;
#10939 = EDGE_CURVE ( 'NONE', #19094, #2770, #27457, .T. ) ;
#10940 = CARTESIAN_POINT ( 'NONE',  ( -3.660532965668825689, 7.124194613927628872, -4.999999999999999112 ) ) ;
#10941 = ADVANCED_FACE ( 'NONE', ( #13514 ), #22842, .T. ) ;
#10942 = CARTESIAN_POINT ( 'NONE',  ( 22.90368100322821121, -1.908636692139587199, -20.53213217155426662 ) ) ;
#10943 = B_SPLINE_CURVE_WITH_KNOTS ( 'NONE', 3,
 ( #12861, #23189, #153, #25629 ),
 .UNSPECIFIED., .F., .F.,
 ( 4, 4 ),
 ( 2.380737581964190397E-07, 0.002336974151641511756 ),
 .UNSPECIFIED. ) ;
#10944 = AXIS2_PLACEMENT_3D ( 'NONE', #12411, #14392, #5562 ) ;
#10945 = ORIENTED_EDGE ( 'NONE', *, *, #14949, .F. ) ;
#10946 = CARTESIAN_POINT ( 'NONE',  ( 134.7287565553230024, -4.999999999999981348, 0.8205080756888000204 ) ) ;
#10948 = ORIENTED_EDGE ( 'NONE', *, *, #7907, .T. ) ;
#10947 = DIRECTION ( 'NONE',  ( 1.000000000000000000, 0.000000000000000000, 0.000000000000000000 ) ) ;
#10949 = PLANE ( 'NONE',  #5399 ) ;
#10950 = DIRECTION ( 'NONE',  ( 0.000000000000000000, 0.000000000000000000, -1.000000000000000000 ) ) ;
#10951 = CARTESIAN_POINT ( 'NONE',  ( 13.10707286029108865, 8.563798077496334926, -15.92507172258792281 ) ) ;
#10952 = CARTESIAN_POINT ( 'NONE',  ( 33.69236230569678980, -11.08454582564024449, -17.09586691508924972 ) ) ;
#10953 = EDGE_LOOP ( 'NONE', ( #14667, #29360, #25200, #25604 ) ) ;
#10954 = CARTESIAN_POINT ( 'NONE',  ( 12.75200725638203281, 7.624046516185085665, -14.92932020320056452 ) ) ;
#10955 = CARTESIAN_POINT ( 'NONE',  ( 27.91615220763155847, -6.225400021157185826, -17.67258836524805332 ) ) ;
#10956 = CARTESIAN_POINT ( 'NONE',  ( 12.86830129319110405, 9.516055860257337073, -16.11539629037995169 ) ) ;
#10957 = DIRECTION ( 'NONE',  ( -2.698458740408365879E-16, 1.000000000000000000, 0.000000000000000000 ) ) ;
#10958 = EDGE_CURVE ( 'NONE', #13649, #28674, #7417, .T. ) ;
#10959 = ORIENTED_EDGE ( 'NONE', *, *, #9586, .T. ) ;
#10960 = EDGE_LOOP ( 'NONE', ( #13599, #1910, #8217, #9771 ) ) ;
#10961 = LINE ( 'NONE', #22731, #28587 ) ;
#10962 = VECTOR ( 'NONE', #25637, 1000.000000000000000 ) ;
#10963 = CARTESIAN_POINT ( 'NONE',  ( 12.50035968906703765, 8.570861208087439564, -15.12988832871674560 ) ) ;
#10964 = LINE ( 'NONE', #11124, #15968 ) ;
#10965 = FACE_OUTER_BOUND ( 'NONE', #18424, .T. ) ;
#10966 = ORIENTED_EDGE ( 'NONE', *, *, #10620, .T. ) ;
#10967 = CARTESIAN_POINT ( 'NONE',  ( 13.12404665403065707, 8.571044468271947991, -15.91156272984762765 ) ) ;
#10968 = ORIENTED_EDGE ( 'NONE', *, *, #4154, .F. ) ;
#10969 = CARTESIAN_POINT ( 'NONE',  ( 23.69691533927305116, -2.951365702903132604, -18.66995449711026822 ) ) ;
#10970 = CARTESIAN_POINT ( 'NONE',  ( 19.05076746314986025, 7.350425291474770084, -20.38782652337943446 ) ) ;
#10971 = VERTEX_POINT ( 'NONE', #28049 ) ;
#10972 = CARTESIAN_POINT ( 'NONE',  ( 11.39659457838139112, -5.000000000000014211, 35.07511151374514213 ) ) ;
#10973 = ORIENTED_EDGE ( 'NONE', *, *, #12594, .F. ) ;
#10974 = CARTESIAN_POINT ( 'NONE',  ( -5.355005115540915739, -6.145890662064674714, -0.08224679563972937812 ) ) ;
#10975 = ADVANCED_FACE ( 'NONE', ( #19297, #23745 ), #3150, .F. ) ;
#10976 = EDGE_LOOP ( 'NONE', ( #75, #21036, #11357, #21205 ) ) ;
#10977 = CARTESIAN_POINT ( 'NONE',  ( 19.12501085131992085, -2.578449613843157184, -15.80510918775627438 ) ) ;
#10978 = VERTEX_POINT ( 'NONE', #16860 ) ;
#10979 = CARTESIAN_POINT ( 'NONE',  ( 174.5152310637604387, -4.999999999999970690, -1.937508276747661892E-14 ) ) ;
#10980 = DIRECTION ( 'NONE',  ( 0.9510565162951536422, 2.566386769018988816E-16, 0.3090169943749472292 ) ) ;
#10981 = VERTEX_POINT ( 'NONE', #5270 ) ;
#10982 = LINE ( 'NONE', #20290, #18021 ) ;
#10983 = DIRECTION ( 'NONE',  ( 0.3090169943749472292, 8.338696094057992503E-17, -0.9510565162951536422 ) ) ;
#10984 = FACE_OUTER_BOUND ( 'NONE', #18485, .T. ) ;
#10985 = VERTEX_POINT ( 'NONE', #26038 ) ;
#10986 = DIRECTION ( 'NONE',  ( -2.698458740408365879E-16, 1.000000000000000000, -0.000000000000000000 ) ) ;
#10987 = EDGE_CURVE ( 'NONE', #22090, #7341, #7557, .T. ) ;
#10988 = CARTESIAN_POINT ( 'NONE',  ( 14.24706144987486667, 6.238427219560604087, -16.72753349211556184 ) ) ;
#10989 = CARTESIAN_POINT ( 'NONE',  ( 12.24683531348137144, 9.516853939945930208, -15.33195173648645593 ) ) ;
#10990 = CARTESIAN_POINT ( 'NONE',  ( 35.52583876341286384, -22.08228901593173177, -18.97221062538168113 ) ) ;
#10991 = EDGE_CURVE ( 'NONE', #12786, #5044, #26712, .T. ) ;
#10992 = ORIENTED_EDGE ( 'NONE', *, *, #23593, .T. ) ;
#10993 = CARTESIAN_POINT ( 'NONE',  ( -24.99999999999998934, 60.00000000000000711, 24.99999999999998934 ) ) ;
#10994 = EDGE_CURVE ( 'NONE', #8651, #22060, #12128, .T. ) ;
#10995 = AXIS2_PLACEMENT_3D ( 'NONE', #24687, #4077, #28998 ) ;
#10996 = CARTESIAN_POINT ( 'NONE',  ( 9.641350810849047548, 17.66889113945805789, -19.66666666666842644 ) ) ;
#10997 = DIRECTION ( 'NONE',  ( 0.3090169943749475623, 8.338696094058001131E-17, 0.9510565162951536422 ) ) ;
#10998 = DIRECTION ( 'NONE',  ( -0.000000000000000000, -0.000000000000000000, -1.000000000000000000 ) ) ;
#10999 = ORIENTED_EDGE ( 'NONE', *, *, #22916, .T. ) ;
#11000 = ORIENTED_EDGE ( 'NONE', *, *, #6567, .T. ) ;
#11001 = LINE ( 'NONE', #13297, #5216 ) ;
#11002 = VERTEX_POINT ( 'NONE', #7707 ) ;
#11003 = CARTESIAN_POINT ( 'NONE',  ( 10.35864924400752862, 16.97212476034085782, -17.91519562840587199 ) ) ;
#11005 = CARTESIAN_POINT ( 'NONE',  ( 32.11202735699620803, -10.19471129157119194, -14.63100864886716934 ) ) ;
#11004 = VECTOR ( 'NONE', #20232, 1000.000000000000000 ) ;
#11006 = CARTESIAN_POINT ( 'NONE',  ( 19.12501085131992085, -2.578449613843157184, -15.80510918775627438 ) ) ;
#11007 = EDGE_LOOP ( 'NONE', ( #5695, #30071, #29681, #25572 ) ) ;
#11008 = VERTEX_POINT ( 'NONE', #554 ) ;
#11009 = VECTOR ( 'NONE', #9977, 1000.000000000000000 ) ;
#11010 = DIRECTION ( 'NONE',  ( -0.9510565162951536422, 0.000000000000000000, -0.3090169943749472292 ) ) ;
#11011 = CARTESIAN_POINT ( 'NONE',  ( 0.000000000000000000, 0.000000000000000000, -23.00000000000000000 ) ) ;
#11012 = CARTESIAN_POINT ( 'NONE',  ( 0.000000000000000000, 0.000000000000000000, 18.00000000000000000 ) ) ;
#11013 = CARTESIAN_POINT ( 'NONE',  ( 29.02390443993225588, -5.138988301204332920, -16.36505798003706857 ) ) ;
#11014 = CARTESIAN_POINT ( 'NONE',  ( 23.76792026503975919, -8.198361753721227885, -14.67730844950409441 ) ) ;
#11015 = ORIENTED_EDGE ( 'NONE', *, *, #12550, .F. ) ;
#11016 = ORIENTED_EDGE ( 'NONE', *, *, #23730, .T. ) ;
#11017 = CARTESIAN_POINT ( 'NONE',  ( 130.7287565553229172, -10.00000000000000888, -19.55415080639416558 ) ) ;
#11018 = CARTESIAN_POINT ( 'NONE',  ( 162.2287565553228887, -1.999999999999973133, -3.509618943233403510 ) ) ;
#11019 = AXIS2_PLACEMENT_3D ( 'NONE', #3156, #19453, #12133 ) ;
#11020 = CARTESIAN_POINT ( 'NONE',  ( 158.6922820468853672, -4.999999999999975131, -17.92658477444275889 ) ) ;
#11021 = PLANE ( 'NONE',  #355 ) ;
#11022 = CARTESIAN_POINT ( 'NONE',  ( -31.74999999999995737, 0.000000000000000000, 0.000000000000000000 ) ) ;
#11023 = CONICAL_SURFACE ( 'NONE', #18830, 2.500000000000002665, 0.9599310885968781459 ) ;
#11024 = DIRECTION ( 'NONE',  ( 0.5877852522924731371, 1.586114251531760728E-16, -0.8090169943749474513 ) ) ;
#11025 = AXIS2_PLACEMENT_3D ( 'NONE', #22447, #4276, #13576 ) ;
#11026 = UNCERTAINTY_MEASURE_WITH_UNIT (LENGTH_MEASURE( 1.000000000000000082E-05 ), #26354, 'distance_accuracy_value', 'NONE');
#11027 = CARTESIAN_POINT ( 'NONE',  ( 13.31307029362551475, 7.598550302509940124, -15.76075481184169647 ) ) ;
#11028 = CARTESIAN_POINT ( 'NONE',  ( 12.13006862794127017, 8.527244997094612700, -15.41586291625151972 ) ) ;
#11029 = DIRECTION ( 'NONE',  ( -2.698458740408365879E-16, 1.000000000000000000, 0.000000000000000000 ) ) ;
#11030 = EDGE_CURVE ( 'NONE', #29780, #9765, #14404, .T. ) ;
#11031 = EDGE_CURVE ( 'NONE', #26001, #8714, #24051, .T. ) ;
#11032 = ORIENTED_EDGE ( 'NONE', *, *, #22103, .T. ) ;
#11033 = DIRECTION ( 'NONE',  ( 1.000000000000000000, -0.000000000000000000, -0.000000000000000000 ) ) ;
#11034 = DIRECTION ( 'NONE',  ( 0.3090169943749472292, 8.338696094057992503E-17, -0.9510565162951536422 ) ) ;
#11035 = EDGE_LOOP ( 'NONE', ( #13119, #17174, #17756, #5403 ) ) ;
#11036 = CARTESIAN_POINT ( 'NONE',  ( 9.745779815811758340, 17.18996641109745482, -16.82979807527155458 ) ) ;
#11037 = EDGE_CURVE ( 'NONE', #2878, #10747, #1251, .T. ) ;
#11038 = DIRECTION ( 'NONE',  ( -2.698458740408365879E-16, 1.000000000000000000, 0.000000000000000000 ) ) ;
#11039 = LINE ( 'NONE', #20053, #26858 ) ;
#11040 = DIRECTION ( 'NONE',  ( 0.000000000000000000, -1.000000000000000000, 1.287488025362403787E-15 ) ) ;
#11041 = EDGE_CURVE ( 'NONE', #29646, #10393, #12424, .T. ) ;
#11043 = ORIENTED_EDGE ( 'NONE', *, *, #30257, .T. ) ;
#11042 = CARTESIAN_POINT ( 'NONE',  ( 21.16681283796276603, -5.103637247178538061, -17.00692323485822754 ) ) ;
#11044 = ORIENTED_EDGE ( 'NONE', *, *, #4985, .F. ) ;
#11045 = LINE ( 'NONE', #15914, #12988 ) ;
#11046 = CARTESIAN_POINT ( 'NONE',  ( 11.05541531668977662, 17.68942339022145305, -17.92015940598198753 ) ) ;
#11047 = CARTESIAN_POINT ( 'NONE',  ( 35.09336438560361415, -20.13941072448723801, -20.22035334018532637 ) ) ;
#11048 = CARTESIAN_POINT ( 'NONE',  ( 132.0152310637605808, -4.999999999999981348, -6.958068083716893781 ) ) ;
#11049 = CIRCLE ( 'NONE', #12984, 0.8500000000000000888 ) ;
#11050 = CARTESIAN_POINT ( 'NONE',  ( 23.22413189157496305, -7.367447486509826504, -15.63851824576001981 ) ) ;
#11051 = CARTESIAN_POINT ( 'NONE',  ( 173.6922820468852819, -4.999999999999970690, -6.413161187712876909 ) ) ;
#11052 = CARTESIAN_POINT ( 'NONE',  ( 23.56326861202678202, -1.685860805813322427, -18.23406631578895798 ) ) ;
#11053 = ORIENTED_EDGE ( 'NONE', *, *, #8542, .T. ) ;
#11054 = DIRECTION ( 'NONE',  ( -0.8090169943749474513, -2.183098979609982436E-16, 0.5877852522924731371 ) ) ;
#11055 = CARTESIAN_POINT ( 'NONE',  ( 13.51621490077814691, 9.019785729699995258, -14.32023381125561556 ) ) ;
#11056 = AXIS2_PLACEMENT_3D ( 'NONE', #29508, #27641, #6707 ) ;
#11057 = CARTESIAN_POINT ( 'NONE',  ( 28.58746438791548528, -7.443717211345676432, -18.79719194573140584 ) ) ;
#11058 = MECHANICAL_DESIGN_GEOMETRIC_PRESENTATION_REPRESENTATION (  '', ( #7166 ), #26174 ) ;
#11059 = VERTEX_POINT ( 'NONE', #18702 ) ;
#11060 = PLANE ( 'NONE',  #14607 ) ;
#11061 = VECTOR ( 'NONE', #16847, 1000.000000000000000 ) ;
#11062 = DIRECTION ( 'NONE',  ( -0.8090169943749474513, -2.183098979609982436E-16, 0.5877852522924731371 ) ) ;
#11063 = DIRECTION ( 'NONE',  ( -0.5877852522924731371, -1.586114251531760728E-16, -0.8090169943749474513 ) ) ;
#11064 = CARTESIAN_POINT ( 'NONE',  ( 142.2287565553230024, -4.999999999999979572, -3.509618943233414168 ) ) ;
#11065 = DIRECTION ( 'NONE',  ( -1.110223024625156540E-16, 0.000000000000000000, -1.000000000000000000 ) ) ;
#11066 = VECTOR ( 'NONE', #11631, 1000.000000000000000 ) ;
#11067 = CARTESIAN_POINT ( 'NONE',  ( 9.641350810849047548, 17.66889113945805789, -17.92981046679734547 ) ) ;
#11068 = CARTESIAN_POINT ( 'NONE',  ( 24.17451698631213475, -5.926886182136407832, -14.25952201372300365 ) ) ;
#11069 = CARTESIAN_POINT ( 'NONE',  ( 17.20140313730510684, 4.016069822000726042, -19.84498366692964666 ) ) ;
#11070 = EDGE_CURVE ( 'NONE', #18037, #11863, #21285, .T. ) ;
#11071 = CARTESIAN_POINT ( 'NONE',  ( 35.92571694232586310, -20.38625956716168020, -21.41712135977877907 ) ) ;
#11072 = DIRECTION ( 'NONE',  ( 0.000000000000000000, -2.775557561562890735E-17, 1.000000000000000000 ) ) ;
#11073 = VECTOR ( 'NONE', #8458, 1000.000000000000000 ) ;
#11074 = CARTESIAN_POINT ( 'NONE',  ( 12.49742530276927610, 8.569573706352677789, -15.13222638044318735 ) ) ;
#11075 = EDGE_CURVE ( 'NONE', #11059, #26241, #19004, .T. ) ;
#11076 = CARTESIAN_POINT ( 'NONE',  ( 176.1922820468853388, -9.999999999999994671, -28.06379628232387802 ) ) ;
#11077 = DIRECTION ( 'NONE',  ( -0.000000000000000000, 0.000000000000000000, 1.000000000000000000 ) ) ;
#11078 = EDGE_CURVE ( 'NONE', #6062, #28182, #9523, .T. ) ;
#11079 = CARTESIAN_POINT ( 'NONE',  ( 9.669898452045105230, 16.21806703136846295, -17.88423646254436861 ) ) ;
#11080 = LINE ( 'NONE', #25127, #15600 ) ;
#11081 = DIRECTION ( 'NONE',  ( -0.8090169943749474513, -2.183098979609982436E-16, 0.5877852522924731371 ) ) ;
#11082 = CARTESIAN_POINT ( 'NONE',  ( 11.77869587587188249, 8.711114196793760200, -15.67004689359726299 ) ) ;
#11083 = VECTOR ( 'NONE', #4615, 1000.000000000000000 ) ;
#11084 = VERTEX_POINT ( 'NONE', #28207 ) ;
#11085 = LINE ( 'NONE', #11234, #20280 ) ;
#11086 = CARTESIAN_POINT ( 'NONE',  ( -4.250000000000000000, -1.366904252225139372E-15, -0.5251556536572770106 ) ) ;
#11087 = CARTESIAN_POINT ( 'NONE',  ( 144.5152310637605808, -10.00000000000000178, -21.71180489736091346 ) ) ;
#11088 = VERTEX_POINT ( 'NONE', #25728 ) ;
#11089 = CARTESIAN_POINT ( 'NONE',  ( 13.38265815842314943, 7.627299838292535661, -15.70544478996546900 ) ) ;
#11090 = CARTESIAN_POINT ( 'NONE',  ( 35.92571694232586310, -20.38625956716168020, -21.41712135977877907 ) ) ;
#11091 = CARTESIAN_POINT ( 'NONE',  ( 22.15888525254269581, 3.701285330253634154, -19.09944157575669621 ) ) ;
#11092 = CARTESIAN_POINT ( 'NONE',  ( 15.40919527484693319, 5.754234090002595003, -19.70842740302703078 ) ) ;
#11093 = VECTOR ( 'NONE', #9908, 1000.000000000000000 ) ;
#11094 = DIRECTION ( 'NONE',  ( -0.000000000000000000, -0.000000000000000000, 1.000000000000000000 ) ) ;
#11095 = CYLINDRICAL_SURFACE ( 'NONE', #25978, 5.000000000000006217 ) ;
#11096 = CARTESIAN_POINT ( 'NONE',  ( 23.73516035876120611, -6.831976609072074602, -19.85773546425274105 ) ) ;
#11097 = VECTOR ( 'NONE', #9464, 999.9999999999998863 ) ;
#11098 = ORIENTED_EDGE ( 'NONE', *, *, #957, .T. ) ;
#11099 = DIRECTION ( 'NONE',  ( -0.5877852522924731371, -1.586114251531760235E-16, 0.8090169943749474513 ) ) ;
#11101 = VERTEX_POINT ( 'NONE', #14103 ) ;
#11100 = FACE_OUTER_BOUND ( 'NONE', #10032, .T. ) ;
#11102 = CARTESIAN_POINT ( 'NONE',  ( 138.6922820468854525, -1.999999999999979572, -9.266330736598359152 ) ) ;
#11103 = CARTESIAN_POINT ( 'NONE',  ( 156.1922820468853956, -10.00000000000000000, -22.25671179336496053 ) ) ;
#11104 = PLANE ( 'NONE',  #8282 ) ;
#11105 = CARTESIAN_POINT ( 'NONE',  ( 35.37054299657279444, -20.38462739797860479, -19.24905200684423789 ) ) ;
#11106 = VERTEX_POINT ( 'NONE', #23437 ) ;
#11107 = CARTESIAN_POINT ( 'NONE',  ( 10.74080116101666427, 8.781381604732478863, -16.37623182050610993 ) ) ;
#11108 = ORIENTED_EDGE ( 'NONE', *, *, #9544, .T. ) ;
#11109 = EDGE_CURVE ( 'NONE', #16948, #5806, #28362, .T. ) ;
#11110 = EDGE_CURVE ( 'NONE', #5536, #28522, #7261, .T. ) ;
#11111 = CIRCLE ( 'NONE', #16972, 2.500000000000000888 ) ;
#11112 = CARTESIAN_POINT ( 'NONE',  ( 25.26806593431409453, -8.821542497490490575, -18.05414547114721557 ) ) ;
#11113 = CARTESIAN_POINT ( 'NONE',  ( 164.7287565553229172, -9.999999999999998224, -16.50000000000000355 ) ) ;
#11114 = EDGE_CURVE ( 'NONE', #26028, #21141, #25886, .T. ) ;
#11115 = CARTESIAN_POINT ( 'NONE',  ( 12.86946920628831670, 9.516571979449480523, -16.11446544321706398 ) ) ;
#11116 = FACE_OUTER_BOUND ( 'NONE', #17309, .T. ) ;
#11117 = EDGE_CURVE ( 'NONE', #12000, #23017, #28508, .T. ) ;
#11118 = EDGE_LOOP ( 'NONE', ( #1805, #19349, #29308, #8114 ) ) ;
#11119 = ORIENTED_EDGE ( 'NONE', *, *, #11341, .T. ) ;
#11120 = VECTOR ( 'NONE', #14789, 1000.000000000000000 ) ;
#11121 = CARTESIAN_POINT ( 'NONE',  ( 144.7287565553230024, -10.00000000000000355, -7.839745962155603820 ) ) ;
#11122 = ORIENTED_EDGE ( 'NONE', *, *, #9165, .F. ) ;
#11123 = CARTESIAN_POINT ( 'NONE',  ( 12.50268541164654756, 8.571888915454989544, -15.12803469218787811 ) ) ;
#11124 = CARTESIAN_POINT ( 'NONE',  ( 175.7287565553229456, -4.999999999999970690, -22.10610323145030520 ) ) ;
#11125 = EDGE_LOOP ( 'NONE', ( #27044, #22208, #21671, #4829 ) ) ;
#11126 = CARTESIAN_POINT ( 'NONE',  ( 152.2287565553230024, -10.00000000000000178, -20.83012701892220520 ) ) ;
#11127 = ORIENTED_EDGE ( 'NONE', *, *, #29831, .T. ) ;
#11128 = CARTESIAN_POINT ( 'NONE',  ( 13.12425544150138279, 8.571136816377206813, -15.91139631635614471 ) ) ;
#11129 = CARTESIAN_POINT ( 'NONE',  ( 24.91993355315554837, -1.627520125476753510, -17.55906114018776876 ) ) ;
#11130 = CARTESIAN_POINT ( 'NONE',  ( 17.51795708650258732, -0.4494001013054305660, -15.13702969726144509 ) ) ;
#11131 = CARTESIAN_POINT ( 'NONE',  ( 14.30110556002302680, 5.443193088601498530, -15.49285935407157666 ) ) ;
#11132 = FACE_OUTER_BOUND ( 'NONE', #7857, .T. ) ;
#11133 = LINE ( 'NONE', #27509, #7433 ) ;
#11134 = CONTEXT_DEPENDENT_SHAPE_REPRESENTATION ( #5604, #8120 ) ;
#11135 = CARTESIAN_POINT ( 'NONE',  ( 19.71807001554888217, -1.708786246101231532, -19.21472004699903380 ) ) ;
#11136 = CARTESIAN_POINT ( 'NONE',  ( 132.0152310637605524, -1.999999999999981348, -8.721423840594310306 ) ) ;
#11137 = CARTESIAN_POINT ( 'NONE',  ( 134.5152310637605808, -1.999999999999980460, -19.94844914048349338 ) ) ;
#11138 = CIRCLE ( 'NONE', #23839, 3.000000000000002665 ) ;
#11139 = VERTEX_POINT ( 'NONE', #7998 ) ;
#11140 = CARTESIAN_POINT ( 'NONE',  ( 10.35864918915110877, 16.97212501191939538, -17.91752729848689185 ) ) ;
#11141 = CARTESIAN_POINT ( 'NONE',  ( 32.48283477683061449, -11.02614750807341260, -17.91093295056291979 ) ) ;
#11142 = AXIS2_PLACEMENT_3D ( 'NONE', #9134, #4580, #2011 ) ;
#11143 = DIRECTION ( 'NONE',  ( -0.9510565162951536422, 0.000000000000000000, -0.3090169943749472292 ) ) ;
#11144 = ORIENTED_EDGE ( 'NONE', *, *, #24594, .F. ) ;
#11145 = ORIENTED_EDGE ( 'NONE', *, *, #27219, .F. ) ;
#11146 = CARTESIAN_POINT ( 'NONE',  ( 172.7287565553229456, -4.999999999999970690, 0.5000000000000029976 ) ) ;
#11147 = CARTESIAN_POINT ( 'NONE',  ( 14.93287775521291394, 9.378568215907955974, -14.88591063491414168 ) ) ;
#11148 = VECTOR ( 'NONE', #6926, 1000.000000000000000 ) ;
#11149 = CARTESIAN_POINT ( 'NONE',  ( 12.24516467974477152, 9.516115653471018732, -15.33328326133307762 ) ) ;
#11150 = CARTESIAN_POINT ( 'NONE',  ( 35.32886446602115171, -21.19738783794349857, -20.03221113960638178 ) ) ;
#11151 = EDGE_CURVE ( 'NONE', #17474, #9904, #13031, .T. ) ;
#11152 = EDGE_LOOP ( 'NONE', ( #18283, #26267, #4397, #12764, #28401, #15775 ) ) ;
#11153 = DIRECTION ( 'NONE',  ( -2.698458740408365879E-16, 1.000000000000000000, 0.000000000000000000 ) ) ;
#11154 = CARTESIAN_POINT ( 'NONE',  ( 12.75704675400704424, 7.626265983139092874, -14.92530421254393147 ) ) ;
#11155 = LINE ( 'NONE', #20606, #11241 ) ;
#11156 = EDGE_LOOP ( 'NONE', ( #16443, #3752, #345, #25322, #29750 ) ) ;
#11157 = CARTESIAN_POINT ( 'NONE',  ( 4.339467034331203621, 6.732211846623402884, -4.999999999999996447 ) ) ;
#11158 = ORIENTED_EDGE ( 'NONE', *, *, #8542, .F. ) ;
#11159 = CARTESIAN_POINT ( 'NONE',  ( 12.89562877257107054, 9.528132359803098694, -16.09361580714184825 ) ) ;
#11160 = VECTOR ( 'NONE', #18041, 1000.000000000000000 ) ;
#11161 = CARTESIAN_POINT ( 'NONE',  ( 34.49115424338278046, -12.94152926980570939, -19.96804914223585925 ) ) ;
#11162 = CARTESIAN_POINT ( 'NONE',  ( 22.39939798857497877, 2.694615832958070722, -14.02792042734668065 ) ) ;
#11163 = ORIENTED_EDGE ( 'NONE', *, *, #13650, .F. ) ;
#11164 = ORIENTED_EDGE ( 'NONE', *, *, #13444, .F. ) ;
#11165 = DIRECTION ( 'NONE',  ( 1.000000000000000000, 0.000000000000000000, 0.000000000000000000 ) ) ;
#11166 = AXIS2_PLACEMENT_3D ( 'NONE', #21641, #10191, #19960 ) ;
#11167 = CARTESIAN_POINT ( 'NONE',  ( 146.4575131106458912, -10.00000000000001599, -186.4312945166758482 ) ) ;
#11168 = CARTESIAN_POINT ( 'NONE',  ( 22.68884594494833706, -6.762261587817247843, -18.56982216542981234 ) ) ;
#11169 = CARTESIAN_POINT ( 'NONE',  ( 28.47173825316771101, -6.366402965996883268, -15.18523185298700007 ) ) ;
#11170 = ORIENTED_EDGE ( 'NONE', *, *, #8015, .T. ) ;
#11171 = ORIENTED_EDGE ( 'NONE', *, *, #10659, .T. ) ;
#11172 = ADVANCED_FACE ( 'NONE', ( #19594 ), #22189, .T. ) ;
#11173 = CARTESIAN_POINT ( 'NONE',  ( 0.000000000000000000, 0.000000000000000000, 18.00000000000000000 ) ) ;
#11174 = CARTESIAN_POINT ( 'NONE',  ( 129.5152310637605524, -1.999999999999982236, -4.391296821672111328 ) ) ;
#11175 = VECTOR ( 'NONE', #28239, 1000.000000000000000 ) ;
#11176 = DIRECTION ( 'NONE',  ( -0.5877852522924731371, 0.000000000000000000, 0.8090169943749474513 ) ) ;
#11177 = CARTESIAN_POINT ( 'NONE',  ( 166.1922820468853104, -9.999999999999998224, -2.083034168790677043 ) ) ;
#11178 = CARTESIAN_POINT ( 'NONE',  ( 12.50140887008201851, 8.571324787501421127, -15.12905211845398412 ) ) ;
#11179 = AXIS2_PLACEMENT_3D ( 'NONE', #18871, #4539, #13829 ) ;
#11180 = CARTESIAN_POINT ( 'NONE',  ( 27.87518295380144551, -11.54787579004265652, -18.81772651352153858 ) ) ;
#11181 = ORIENTED_EDGE ( 'NONE', *, *, #24109, .F. ) ;
#11182 = DIRECTION ( 'NONE',  ( -2.698458740408365879E-16, 1.000000000000000000, 0.000000000000000000 ) ) ;
#11183 = EDGE_LOOP ( 'NONE', ( #10672, #2647, #6691, #1009 ) ) ;
#11184 = FACE_OUTER_BOUND ( 'NONE', #26930, .T. ) ;
#11185 = CARTESIAN_POINT ( 'NONE',  ( 30.94061990612449264, -11.12808277128230294, -15.28946652318938959 ) ) ;
#11186 = CARTESIAN_POINT ( 'NONE',  ( 132.0152310637605808, -1.999999999999981348, -32.93883019725009120 ) ) ;
#11187 = DIRECTION ( 'NONE',  ( -1.110223024625156540E-16, 0.000000000000000000, -1.000000000000000000 ) ) ;
#11189 = ORIENTED_EDGE ( 'NONE', *, *, #24181, .T. ) ;
#11188 = CARTESIAN_POINT ( 'NONE',  ( 24.52797215547132836, -1.897736678990579184, -19.26084780660264073 ) ) ;
#11190 = ORIENTED_EDGE ( 'NONE', *, *, #15589, .F. ) ;
#11191 = CARTESIAN_POINT ( 'NONE',  ( 173.6922820468853104, -9.999999999999994671, -17.92658477444275889 ) ) ;
#11192 = CARTESIAN_POINT ( 'NONE',  ( 12.24619727527933222, 9.516571979449480523, -15.33246026419563890 ) ) ;
#11193 = CARTESIAN_POINT ( 'NONE',  ( 35.54859390953724585, -22.18451583373416014, -16.11276402859391865 ) ) ;
#11194 = FACE_OUTER_BOUND ( 'NONE', #15049, .T. ) ;
#11195 = CARTESIAN_POINT ( 'NONE',  ( 22.16846437878366061, -4.107540447007581363, -19.06500358040360865 ) ) ;
#11196 = FACE_OUTER_BOUND ( 'NONE', #19374, .T. ) ;
#11197 = CARTESIAN_POINT ( 'NONE',  ( 25.72346593501046996, -2.209713236584236018, -16.07608620281017053 ) ) ;
#11198 = ORIENTED_EDGE ( 'NONE', *, *, #16704, .T. ) ;
#11199 = PRODUCT_DEFINITION_FORMATION_WITH_SPECIFIED_SOURCE ( 'ANY', '', #18122, .NOT_KNOWN. ) ;
#11200 = LINE ( 'NONE', #8904, #14455 ) ;
#11201 = VECTOR ( 'NONE', #27459, 1000.000000000000000 ) ;
#11202 = CARTESIAN_POINT ( 'NONE',  ( 17.83091951040035283, 10.74857467630938501, -15.40187535130914753 ) ) ;
#11203 = CARTESIAN_POINT ( 'NONE',  ( 28.55476651072185845, -11.97999099613336504, -13.94805024529803994 ) ) ;
#11204 = VECTOR ( 'NONE', #6918, 1000.000000000000000 ) ;
#11205 = CIRCLE ( 'NONE', #18500, 13.00000000000000178 ) ;
#11206 = VECTOR ( 'NONE', #29286, 1000.000000000000000 ) ;
#11207 = ORIENTED_EDGE ( 'NONE', *, *, #1240, .T. ) ;
#11208 = EDGE_LOOP ( 'NONE', ( #1527, #27183, #8472, #29878 ) ) ;
#11209 = EDGE_CURVE ( 'NONE', #1955, #16958, #29109, .T. ) ;
#11210 = EDGE_CURVE ( 'NONE', #6687, #26171, #29427, .T. ) ;
#11211 = LINE ( 'NONE', #77, #21452 ) ;
#11212 = EDGE_CURVE ( 'NONE', #18633, #2363, #15464, .T. ) ;
#11213 = FACE_OUTER_BOUND ( 'NONE', #6134, .T. ) ;
#11214 = AXIS2_PLACEMENT_3D ( 'NONE', #6250, #15546, #22581 ) ;
#11215 = CYLINDRICAL_SURFACE ( 'NONE', #9230, 4.000000000000001776 ) ;
#11216 = AXIS2_PLACEMENT_3D ( 'NONE', #27109, #1451, #5876 ) ;
#11217 = DIRECTION ( 'NONE',  ( -0.5877852522924731371, -1.586114251531760728E-16, -0.8090169943749474513 ) ) ;
#11218 = DIRECTION ( 'NONE',  ( 0.5877852522924731371, 1.586114251531760728E-16, 0.8090169943749474513 ) ) ;
#11219 = LINE ( 'NONE', #11361, #10155 ) ;
#11220 = CARTESIAN_POINT ( 'NONE',  ( 23.84753192840887337, -5.516882280943989691, -18.03677479665242345 ) ) ;
#11221 = CARTESIAN_POINT ( 'NONE',  ( 20.05507840940144959, 2.642024363331392234, -19.51255487852252912 ) ) ;
#11223 = ORIENTED_EDGE ( 'NONE', *, *, #8321, .T. ) ;
#11222 = CARTESIAN_POINT ( 'NONE',  ( 34.47915806976548936, -13.88763681628941349, -21.00674453490027460 ) ) ;
#11225 = LINE ( 'NONE', #22221, #13914 ) ;
#11224 = VECTOR ( 'NONE', #17362, 1000.000000000000000 ) ;
#11226 = CARTESIAN_POINT ( 'NONE',  ( 12.50098444160134470, 8.571137227758441668, -15.12939039523150520 ) ) ;
#11227 = DIRECTION ( 'NONE',  ( 0.000000000000000000, 0.000000000000000000, -1.000000000000000000 ) ) ;
#11228 = CARTESIAN_POINT ( 'NONE',  ( 148.6922820468854525, -10.00000000000000178, -23.73366926340167637 ) ) ;
#11229 = CARTESIAN_POINT ( 'NONE',  ( 9.667771292961528928, 16.22782245407549340, -17.88511957776909966 ) ) ;
#11230 = FACE_OUTER_BOUND ( 'NONE', #23354, .T. ) ;
#11231 = DIRECTION ( 'NONE',  ( -1.000000000000000000, 0.000000000000000000, 0.000000000000000000 ) ) ;
#11232 = CARTESIAN_POINT ( 'NONE',  ( 11.82447321682112751, 8.672047275158794477, -15.63808403058127006 ) ) ;
#11233 = ORIENTED_EDGE ( 'NONE', *, *, #2925, .F. ) ;
#11234 = CARTESIAN_POINT ( 'NONE',  ( 88.21376772083030460, -4.999999999999993783, -64.09105380476975711 ) ) ;
#11235 = CARTESIAN_POINT ( 'NONE',  ( 129.5152310637605524, -10.00000000000000888, -30.37205893520530964 ) ) ;
#11236 = LINE ( 'NONE', #27317, #13204 ) ;
#11237 = ORIENTED_EDGE ( 'NONE', *, *, #15060, .T. ) ;
#11238 = CARTESIAN_POINT ( 'NONE',  ( 9.112830967032516938, 16.17999385759334885, -17.05460035006107589 ) ) ;
#11239 = CARTESIAN_POINT ( 'NONE',  ( 33.21739345078569272, -12.71166704379270129, -20.69560413545502797 ) ) ;
#11240 = CARTESIAN_POINT ( 'NONE',  ( 18.68528716101036480, 3.575476808761081760, -13.14399490972872186 ) ) ;
#11241 = VECTOR ( 'NONE', #20458, 1000.000000000000000 ) ;
#11242 = CARTESIAN_POINT ( 'NONE',  ( 31.69910715399011636, -11.01187737159756352, -14.44698884073069145 ) ) ;
#11243 = CARTESIAN_POINT ( 'NONE',  ( 158.6922820468853956, -1.999999999999973577, -26.58683881228715862 ) ) ;
#11244 = CARTESIAN_POINT ( 'NONE',  ( 18.48843674521961589, -1.244547778534776938, -16.48413177534300900 ) ) ;
#11245 = EDGE_CURVE ( 'NONE', #930, #4943, #12186, .T. ) ;
#11246 = PRESENTATION_LAYER_ASSIGNMENT (  '', '', ( #42 ) ) ;
#11247 = MANIFOLD_SOLID_BREP ( 'Hex', #1445 ) ;
#11248 = ADVANCED_FACE ( 'NONE', ( #5877 ), #15157, .T. ) ;
#11249 = ORIENTED_EDGE ( 'NONE', *, *, #13183, .F. ) ;
#11250 = EDGE_CURVE ( 'NONE', #19044, #15401, #3885, .T. ) ;
#11251 = DIRECTION ( 'NONE',  ( 0.3090169943749475623, 8.338696094058001131E-17, 0.9510565162951536422 ) ) ;
#11253 = VERTEX_POINT ( 'NONE', #26804 ) ;
#11252 = CARTESIAN_POINT ( 'NONE',  ( 147.0152310637605240, -1.999999999999977129, -8.721423840594312082 ) ) ;
#11254 = CARTESIAN_POINT ( 'NONE',  ( 2.000000000000026201, 3.464101615137736623, 8.673617379884035472E-16 ) ) ;
#11255 = VECTOR ( 'NONE', #26995, 1000.000000000000000 ) ;
#11256 = CARTESIAN_POINT ( 'NONE',  ( 13.55939796120610374, 8.763434079353437767, -15.56458004748339263 ) ) ;
#11257 = CARTESIAN_POINT ( 'NONE',  ( 35.54170021948790748, -21.15354613602950096, -18.58520066250327929 ) ) ;
#11258 = ORIENTED_EDGE ( 'NONE', *, *, #27588, .T. ) ;
#11259 = VECTOR ( 'NONE', #18854, 1000.000000000000000 ) ;
#11260 = CARTESIAN_POINT ( 'NONE',  ( 10.66464987567688993, 9.063154531648658363, -16.41286864359600983 ) ) ;
#11261 = ORIENTED_EDGE ( 'NONE', *, *, #29173, .T. ) ;
#11262 = CARTESIAN_POINT ( 'NONE',  ( 26.32595758385100382, -12.12905223104374386, -14.21117607008287642 ) ) ;
#11263 = FACE_OUTER_BOUND ( 'NONE', #20716, .T. ) ;
#11264 = CARTESIAN_POINT ( 'NONE',  ( 10.99070134719017311, 14.07345324724201063, -17.12031169937328201 ) ) ;
#11265 = CARTESIAN_POINT ( 'NONE',  ( 175.7287565553229456, -4.999999999999970690, 3.500000000000003109 ) ) ;
#11266 = CARTESIAN_POINT ( 'NONE',  ( 162.0152310637604955, -4.999999999999974243, -1.798730398669517955E-14 ) ) ;
#11267 = ORIENTED_EDGE ( 'NONE', *, *, #16565, .F. ) ;
#11268 = CARTESIAN_POINT ( 'NONE',  ( 157.0152310637604387, -4.999999999999975131, -1.743219247438259497E-14 ) ) ;
#11269 = CARTESIAN_POINT ( 'NONE',  ( 12.50162201464318557, 8.571418981294288031, -15.12888223836978341 ) ) ;
#11270 = VERTEX_POINT ( 'NONE', #19895 ) ;
#11271 = VERTEX_POINT ( 'NONE', #6171 ) ;
#11272 = DIRECTION ( 'NONE',  ( 0.9510565162951536422, 0.000000000000000000, -0.3090169943749475623 ) ) ;
#11273 = ORIENTED_EDGE ( 'NONE', *, *, #9024, .T. ) ;
#11274 = CARTESIAN_POINT ( 'NONE',  ( 13.12174330432777047, 8.570030634161971861, -15.91339823077023929 ) ) ;
#11275 = CARTESIAN_POINT ( 'NONE',  ( 24.98402180921622673, -1.135180495641346266, -16.01319527449767932 ) ) ;
#11276 = CARTESIAN_POINT ( 'NONE',  ( 25.05533511103952904, -1.369129923259265524, -16.98221401193426416 ) ) ;
#11277 = CARTESIAN_POINT ( 'NONE',  ( 19.14470263920462401, 1.819183656627200829, -19.33730474122706866 ) ) ;
#11278 = LINE ( 'NONE', #6259, #11608 ) ;
#11279 = DIRECTION ( 'NONE',  ( -0.9510565162951536422, -2.566386769018988323E-16, 0.3090169943749475623 ) ) ;
#11280 = ORIENTED_EDGE ( 'NONE', *, *, #24801, .F. ) ;
#11281 = CIRCLE ( 'NONE', #578, 5.000000000000000000 ) ;
#11282 = CARTESIAN_POINT ( 'NONE',  ( 20.14386580841007657, 1.771853782379294140, -13.30505882909219295 ) ) ;
#11283 = ADVANCED_FACE ( 'NONE', ( #29265 ), #21498, .T. ) ;
#11284 = ORIENTED_EDGE ( 'NONE', *, *, #5545, .T. ) ;
#11285 = EDGE_CURVE ( 'NONE', #9780, #209, #24638, .T. ) ;
#11286 = EDGE_CURVE ( 'NONE', #9036, #1194, #24492, .T. ) ;
#11287 = CARTESIAN_POINT ( 'NONE',  ( -1.310841663519413114, 0.000000000000000000, 0.000000000000000000 ) ) ;
#11288 = EDGE_CURVE ( 'NONE', #7265, #8429, #17752, .T. ) ;
#11289 = CARTESIAN_POINT ( 'NONE',  ( 172.0152310637604387, -9.999999999999996447, -6.958068083716895558 ) ) ;
#11290 = CARTESIAN_POINT ( 'NONE',  ( 10.35865266338826984, 16.97210907862488938, -17.91126819201198472 ) ) ;
#11291 = CARTESIAN_POINT ( 'NONE',  ( 159.7287565553229740, -4.999999999999974243, -25.16025403784441394 ) ) ;
#11292 = DIRECTION ( 'NONE',  ( 0.5877852522924731371, 1.586114251531760728E-16, -0.8090169943749474513 ) ) ;
#11293 = ORIENTED_EDGE ( 'NONE', *, *, #9443, .T. ) ;
#11294 = DIRECTION ( 'NONE',  ( 2.698458740408365879E-16, -1.000000000000000000, 0.000000000000000000 ) ) ;
#11295 = CARTESIAN_POINT ( 'NONE',  ( 18.47369133221681281, 7.987600538477567014, -15.27093437040897861 ) ) ;
#11296 = CARTESIAN_POINT ( 'NONE',  ( 11.43821061673542872, 15.93387534916056758, -16.71752457030684980 ) ) ;
#11297 = CARTESIAN_POINT ( 'NONE',  ( 33.68411698100747032, -13.80840863474736935, -19.79436191385186916 ) ) ;
#11298 = ORIENTED_EDGE ( 'NONE', *, *, #8956, .F. ) ;
#11299 =( BOUNDED_CURVE ( )  B_SPLINE_CURVE ( 3, ( #26588, #5672, #3385, #8397 ),
 .UNSPECIFIED., .F., .F. ) 
 B_SPLINE_CURVE_WITH_KNOTS ( ( 4, 4 ),
 ( 0.001563228649568139134, 0.003126104531729828346 ),
 .UNSPECIFIED. ) 
 CURVE ( )  GEOMETRIC_REPRESENTATION_ITEM ( )  RATIONAL_B_SPLINE_CURVE ( ( 1.000000000000001110, 0.3333333333333333703, 0.3333333333333322046, 1.000000000000000000 ) ) 
 REPRESENTATION_ITEM ( '' )  );
#11300 = ORIENTED_EDGE ( 'NONE', *, *, #22076, .T. ) ;
#11301 = CARTESIAN_POINT ( 'NONE',  ( 143.6922820468854241, -1.999999999999978462, -9.266330736598359152 ) ) ;
#11302 = CARTESIAN_POINT ( 'NONE',  ( 9.641384570184822422, 17.66873631484086715, -17.89388817125738385 ) ) ;
#11303 = CARTESIAN_POINT ( 'NONE',  ( 136.1922820468854241, -10.00000000000000533, -2.083034168790677043 ) ) ;
#11304 = DIRECTION ( 'NONE',  ( 1.110223024625156540E-16, 2.995891024602366092E-32, 1.000000000000000000 ) ) ;
#11305 = ORIENTED_EDGE ( 'NONE', *, *, #4950, .T. ) ;
#11306 = CARTESIAN_POINT ( 'NONE',  ( 141.1922820468854241, -1.999999999999979128, -4.936203717676158398 ) ) ;
#11307 = ORIENTED_EDGE ( 'NONE', *, *, #15650, .F. ) ;
#11308 = CARTESIAN_POINT ( 'NONE',  ( 12.86946920628831670, 9.516571979449480523, -16.11446544321706398 ) ) ;
#11309 = CARTESIAN_POINT ( 'NONE',  ( 35.06179249480944549, -15.50510465796065596, -20.14053939611612520 ) ) ;
#11310 = CARTESIAN_POINT ( 'NONE',  ( 25.77659985377941254, -6.250509680199615836, -13.67467641272277312 ) ) ;
#11311 = LINE ( 'NONE', #22778, #2367 ) ;
#11312 = DIRECTION ( 'NONE',  ( 0.000000000000000000, 0.000000000000000000, 1.000000000000000000 ) ) ;
#11313 = CARTESIAN_POINT ( 'NONE',  ( 28.50411217586706769, -6.135108760518566129, -18.55796808427148648 ) ) ;
#11314 = CARTESIAN_POINT ( 'NONE',  ( 28.03106068525412908, -6.431813172927290267, -14.41205174211060402 ) ) ;
#11315 = ADVANCED_FACE ( 'NONE', ( #29882 ), #15619, .T. ) ;
#11316 = VECTOR ( 'NONE', #11279, 999.9999999999998863 ) ;
#11317 = EDGE_CURVE ( 'NONE', #17166, #1955, #27273, .T. ) ;
#11319 = EDGE_LOOP ( 'NONE', ( #12935, #20895, #2403, #20897 ) ) ;
#11318 = EDGE_CURVE ( 'NONE', #9904, #5737, #20496, .T. ) ;
#11320 = CARTESIAN_POINT ( 'NONE',  ( -8.000000000000000000, 4.618802153517001408, -0.7145311798163294092 ) ) ;
#11321 = CARTESIAN_POINT ( 'NONE',  ( 173.6922820468853104, -1.999999999999970024, -17.92658477444275889 ) ) ;
#11322 = DIRECTION ( 'NONE',  ( -2.908569913943825554E-16, 1.000000000000000000, -0.000000000000000000 ) ) ;
#11323 = AXIS2_PLACEMENT_3D ( 'NONE', #12027, #23335, #2454 ) ;
#11324 = CARTESIAN_POINT ( 'NONE',  ( 157.0152310637605524, -1.999999999999973133, -34.70218595412750773 ) ) ;
#11325 = UNCERTAINTY_MEASURE_WITH_UNIT (LENGTH_MEASURE( 1.000000000000000082E-05 ), #15429, 'distance_accuracy_value', 'NONE');
#11326 = CARTESIAN_POINT ( 'NONE',  ( 12.49428694376680049, 8.568214790255201052, -15.13472557389765072 ) ) ;
#11327 = CARTESIAN_POINT ( 'NONE',  ( 31.69910715399011636, -11.01187737159756352, -14.44698884073069145 ) ) ;
#11328 = EDGE_LOOP ( 'NONE', ( #13836, #27685, #5544, #8761 ) ) ;
#11329 = CARTESIAN_POINT ( 'NONE',  ( 2.000000000000003553, -3.464101615137736623, 8.673617379884035472E-16 ) ) ;
#11330 = ORIENTED_EDGE ( 'NONE', *, *, #27690, .T. ) ;
#11331 = CARTESIAN_POINT ( 'NONE',  ( 9.641350810849047548, 17.66889113945805789, -17.92981046679734547 ) ) ;
#11332 = AXIS2_PLACEMENT_3D ( 'NONE', #9817, #25440, #2982 ) ;
#11333 = CARTESIAN_POINT ( 'NONE',  ( 15.19333023161420648, 6.044621996704095501, -18.15278115226310263 ) ) ;
#11334 = CARTESIAN_POINT ( 'NONE',  ( 134.5152310637605808, -10.00000000000000533, -19.94844914048349338 ) ) ;
#11335 = DIRECTION ( 'NONE',  ( 0.000000000000000000, -0.8660254037844390407, -0.4999999999999994449 ) ) ;
#11337 = VERTEX_POINT ( 'NONE', #13472 ) ;
#11336 = CARTESIAN_POINT ( 'NONE',  ( 24.18219217278060995, -6.970120066757704791, -14.18070892486464629 ) ) ;
#11338 = VERTEX_POINT ( 'NONE', #8890 ) ;
#11339 = CARTESIAN_POINT ( 'NONE',  ( 156.1922820468853672, -10.00000000000000000, -10.74328820663507678 ) ) ;
#11340 = CARTESIAN_POINT ( 'NONE',  ( 12.24537663854593816, 9.516207477791880365, -15.33311446707169701 ) ) ;
#11341 = EDGE_CURVE ( 'NONE', #29240, #17052, #11475, .T. ) ;
#11342 = ORIENTED_EDGE ( 'NONE', *, *, #27322, .T. ) ;
#11343 = CARTESIAN_POINT ( 'NONE',  ( 33.57712230886461668, -13.32773824946660923, -19.76201999124979736 ) ) ;
#11344 = CARTESIAN_POINT ( 'NONE',  ( 15.19603151210977821, 9.502094893032342782, -14.87270315361914896 ) ) ;
#11345 = CARTESIAN_POINT ( 'NONE',  ( 26.31132954256896639, -3.159408024760113509, -14.81636702655834803 ) ) ;
#11346 = CARTESIAN_POINT ( 'NONE',  ( 8.000000000000008882, 3.115336682267025203, -4.680606868608483850 ) ) ;
#11347 = CARTESIAN_POINT ( 'NONE',  ( 20.39818463913025681, -2.063888138892570723, -16.18016139629216354 ) ) ;
#11348 = ORIENTED_EDGE ( 'NONE', *, *, #5297, .T. ) ;
#11349 = CARTESIAN_POINT ( 'NONE',  ( 3.999999999999980904, -2.309401076758567317, -0.3572655899081716435 ) ) ;
#11350 = CARTESIAN_POINT ( 'NONE',  ( 17.10097030076851610, 6.697663726599960121, -13.82760435466811089 ) ) ;
#11351 = VECTOR ( 'NONE', #21640, 1000.000000000000000 ) ;
#11352 = CARTESIAN_POINT ( 'NONE',  ( 28.61171173311277016, -11.12923776720465874, -18.00325214586577971 ) ) ;
#11353 = ORIENTED_EDGE ( 'NONE', *, *, #26218, .T. ) ;
#11354 = CARTESIAN_POINT ( 'NONE',  ( 23.56128742750157201, -5.000000000000011546, -72.51418643027592736 ) ) ;
#11355 = CIRCLE ( 'NONE', #28466, 5.999999999999977796 ) ;
#11356 = DIRECTION ( 'NONE',  ( 1.000000000000000000, 0.000000000000000000, 0.000000000000000000 ) ) ;
#11357 = ORIENTED_EDGE ( 'NONE', *, *, #3151, .F. ) ;
#11358 = PLANE ( 'NONE',  #29801 ) ;
#11359 = DIRECTION ( 'NONE',  ( 0.9510565162951535312, 2.566386769018988816E-16, -0.3090169943749475623 ) ) ;
#11360 = CARTESIAN_POINT ( 'NONE',  ( 138.6922820468854525, -4.999999999999980460, -6.413161187712876909 ) ) ;
#11361 = CARTESIAN_POINT ( 'NONE',  ( 111.0562616426541069, -4.999999999999986677, 80.68709708467871167 ) ) ;
#11362 = CARTESIAN_POINT ( 'NONE',  ( 23.18557557936948044, -8.345241077663208884, -16.42592668061853800 ) ) ;
#11363 = CARTESIAN_POINT ( 'NONE',  ( 18.53947781130984751, 1.256531364521723537, -18.82393729036428098 ) ) ;
#11364 = AXIS2_PLACEMENT_3D ( 'NONE', #1110, #3538, #24146 ) ;
#11366 = VERTEX_POINT ( 'NONE', #15764 ) ;
#11365 = CARTESIAN_POINT ( 'NONE',  ( 34.13391181137448882, -12.33661648534566524, -20.90239171999057888 ) ) ;
#11367 = CARTESIAN_POINT ( 'NONE',  ( 0.000000000000000000, 0.000000000000000000, 18.00000000000000000 ) ) ;
#11368 = CARTESIAN_POINT ( 'NONE',  ( 11.47293561586387867, 9.269010148984008879, -15.86088772249501666 ) ) ;
#11369 = LINE ( 'NONE', #20674, #16644 ) ;
#11370 = CARTESIAN_POINT ( 'NONE',  ( 148.6922820468853956, -1.999999999999977129, -9.266330736598359152 ) ) ;
#11371 = CARTESIAN_POINT ( 'NONE',  ( 9.662070302079424522, 16.25396792496884046, -17.90822120357413638 ) ) ;
#11372 = DIRECTION ( 'NONE',  ( -0.9773680663943724589, -5.871577894680262505E-18, 0.2115458881484710285 ) ) ;
#11373 = EDGE_LOOP ( 'NONE', ( #25982, #342 ) ) ;
#11374 = CARTESIAN_POINT ( 'NONE',  ( 130.7287565553229172, -10.00000000000000888, -28.21440484423856532 ) ) ;
#11375 = CARTESIAN_POINT ( 'NONE',  ( 12.50098444160134470, 8.571137227758441668, -15.12939039523150520 ) ) ;
#11376 = EDGE_CURVE ( 'NONE', #10549, #2849, #13327, .T. ) ;
#11377 = ORIENTED_EDGE ( 'NONE', *, *, #18173, .F. ) ;
#11378 = LINE ( 'NONE', #20681, #5168 ) ;
#11379 = DIRECTION ( 'NONE',  ( -1.000000000000000000, 0.000000000000000000, -0.000000000000000000 ) ) ;
#11380 = FACE_OUTER_BOUND ( 'NONE', #29285, .T. ) ;
#11381 = AXIS2_PLACEMENT_3D ( 'NONE', #9055, #20968, #2378 ) ;
#11382 = ORIENTED_EDGE ( 'NONE', *, *, #6056, .F. ) ;
#11383 = CARTESIAN_POINT ( 'NONE',  ( 9.132840175088396961, 16.08822907886823472, -17.04632583937691592 ) ) ;
#11384 = CARTESIAN_POINT ( 'NONE',  ( 31.39893620166130717, -10.86152586746012183, -14.84747879817187943 ) ) ;
#11385 = CARTESIAN_POINT ( 'NONE',  ( 15.52843720209238931, 6.760224976758691717, -13.32525641785786696 ) ) ;
#11386 = CARTESIAN_POINT ( 'NONE',  ( 18.45234147263269620, 6.489596213788811241, -14.85506563039705519 ) ) ;
#11387 = CARTESIAN_POINT ( 'NONE',  ( -3.319543390096040270, 7.321065037175434220, -4.983111142572229646 ) ) ;
#11388 = CARTESIAN_POINT ( 'NONE',  ( 23.77355757633466382, -7.879698323813751237, -13.16654918938113283 ) ) ;
#11389 = ORIENTED_EDGE ( 'NONE', *, *, #24357, .F. ) ;
#11390 = LINE ( 'NONE', #6834, #8421 ) ;
#11391 = DIRECTION ( 'NONE',  ( -2.698458740408365879E-16, 1.000000000000000000, 0.000000000000000000 ) ) ;
#11392 = ORIENTED_EDGE ( 'NONE', *, *, #10002, .T. ) ;
#11393 = DIRECTION ( 'NONE',  ( -2.698458740408365879E-16, 1.000000000000000000, 0.000000000000000000 ) ) ;
#11394 = AXIS2_PLACEMENT_3D ( 'NONE', #16463, #28112, #14009 ) ;
#11395 = DIRECTION ( 'NONE',  ( -1.110223024625156540E-16, 0.000000000000000000, -1.000000000000000000 ) ) ;
#11396 = CARTESIAN_POINT ( 'NONE',  ( 35.39068211221506743, -20.47510177656754493, -19.23609803736608725 ) ) ;
#11397 = CARTESIAN_POINT ( 'NONE',  ( 11.11829553246053770, 8.091015213210848600, -16.14073874907621331 ) ) ;
#11398 = ORIENTED_EDGE ( 'NONE', *, *, #22076, .F. ) ;
#11399 = CARTESIAN_POINT ( 'NONE',  ( 27.78884322698630882, -6.380937659459246625, -17.89340433249687834 ) ) ;
#11400 = CARTESIAN_POINT ( 'NONE',  ( 149.5152310637605240, -4.999999999999976907, -13.05155085951651195 ) ) ;
#11401 = CARTESIAN_POINT ( 'NONE',  ( 10.50441255335269020, 16.30363564318377811, -17.32140922184415288 ) ) ;
#11402 = DIRECTION ( 'NONE',  ( 0.9510565162951535312, 2.566386769018988816E-16, -0.3090169943749475623 ) ) ;
#11403 = DIRECTION ( 'NONE',  ( -0.8090169943749474513, -2.183098979609982436E-16, -0.5877852522924731371 ) ) ;
#11404 = EDGE_CURVE ( 'NONE', #22598, #28447, #23100, .T. ) ;
#11405 = EDGE_CURVE ( 'NONE', #13495, #10404, #29732, .T. ) ;
#11406 = ORIENTED_EDGE ( 'NONE', *, *, #9800, .T. ) ;
#11407 = DIRECTION ( 'NONE',  ( 0.5877852522924731371, 1.586114251531760728E-16, 0.8090169943749474513 ) ) ;
#11408 = ORIENTED_EDGE ( 'NONE', *, *, #3408, .F. ) ;
#11409 = ADVANCED_FACE ( 'NONE', ( #22955 ), #24951, .T. ) ;
#11410 = CARTESIAN_POINT ( 'NONE',  ( 14.38576730248667701, 9.404056492746565965, -13.62718518646353161 ) ) ;
#11411 = ORIENTED_EDGE ( 'NONE', *, *, #19484, .T. ) ;
#11412 = EDGE_CURVE ( 'NONE', #2849, #4933, #8740, .T. ) ;
#11413 = LINE ( 'NONE', #28250, #15926 ) ;
#11414 = ORIENTED_EDGE ( 'NONE', *, *, #13691, .F. ) ;
#11415 = CARTESIAN_POINT ( 'NONE',  ( 9.664154528927689114, 16.24440939496457403, -17.89215119606715021 ) ) ;
#11416 = CARTESIAN_POINT ( 'NONE',  ( 21.88384027766407414, -2.187040905716116868, -14.00385029740408704 ) ) ;
#11417 = CARTESIAN_POINT ( 'NONE',  ( 24.36273546358933828, 1.710929640254579720, -17.54733717687237160 ) ) ;
#11418 = CARTESIAN_POINT ( 'NONE',  ( 21.26575470983302196, 3.903880982571942493, -18.68858533207590966 ) ) ;
#11419 = CARTESIAN_POINT ( 'NONE',  ( -20.00000000000017053, 34.64101615137744972, -10.00000000000000000 ) ) ;
#11420 = CIRCLE ( 'NONE', #24592, 2.000000000000000000 ) ;
#11421 = FACE_OUTER_BOUND ( 'NONE', #3041, .T. ) ;
#11422 = CARTESIAN_POINT ( 'NONE',  ( 22.29983652437130814, 0.6627547066652448304, -20.09853802436992964 ) ) ;
#11423 = APPLICATION_CONTEXT ( 'automotive_design' ) ;
#11424 = DIRECTION ( 'NONE',  ( 0.000000000000000000, 0.000000000000000000, -1.000000000000000000 ) ) ;
#11425 = CARTESIAN_POINT ( 'NONE',  ( 17.03854528076240271, -5.000000000000013323, -52.43925030801758425 ) ) ;
#11426 = EDGE_CURVE ( 'NONE', #28060, #3594, #25533, .T. ) ;
#11427 = CARTESIAN_POINT ( 'NONE',  ( 10.35865057885519214, 16.97211863855931924, -17.91295731025335414 ) ) ;
#11428 = CARTESIAN_POINT ( 'NONE',  ( 35.54859390953724585, -22.18451583373416014, -16.11276402859391865 ) ) ;
#11429 = FACE_OUTER_BOUND ( 'NONE', #20428, .T. ) ;
#11430 = ORIENTED_EDGE ( 'NONE', *, *, #22792, .T. ) ;
#11431 = EDGE_LOOP ( 'NONE', ( #28899, #14449, #29580, #20756, #22437 ) ) ;
#11432 = CARTESIAN_POINT ( 'NONE',  ( 12.58835545445038306, -5.000000000000014211, 38.74297434227223391 ) ) ;
#11433 = VECTOR ( 'NONE', #29563, 1000.000000000000000 ) ;
#11434 = CARTESIAN_POINT ( 'NONE',  ( 13.77718166750866224, 8.859676595473322536, -15.39100258941132715 ) ) ;
#11435 = CARTESIAN_POINT ( 'NONE',  ( 11.05584814685795081, 17.68743837589741830, -17.84564518929906285 ) ) ;
#11436 = CARTESIAN_POINT ( 'NONE',  ( 33.43446274600908907, -12.68684440242773448, -19.71889742777951327 ) ) ;
#11437 = EDGE_LOOP ( 'NONE', ( #23133, #23042, #8930, #10543 ) ) ;
#11438 = VERTEX_POINT ( 'NONE', #10883 ) ;
#11439 = CARTESIAN_POINT ( 'NONE',  ( 9.916118674515717046, 16.40877069192658055, -16.50468880802031890 ) ) ;
#11440 = EDGE_CURVE ( 'NONE', #21937, #19636, #15910, .T. ) ;
#11441 = CARTESIAN_POINT ( 'NONE',  ( 9.641350810849047548, 17.66889113945805789, -17.92279151347709032 ) ) ;
#11442 = DIRECTION ( 'NONE',  ( 0.000000000000000000, -2.775557561562890735E-17, 1.000000000000000000 ) ) ;
#11443 = LINE ( 'NONE', #15730, #19837 ) ;
#11444 = ADVANCED_FACE ( 'NONE', ( #25240 ), #18356, .T. ) ;
#11445 = EDGE_CURVE ( 'NONE', #26738, #25636, #22561, .T. ) ;
#11446 = ORIENTED_EDGE ( 'NONE', *, *, #18894, .F. ) ;
#11447 = CARTESIAN_POINT ( 'NONE',  ( 149.5152310637606092, -1.999999999999975353, -28.60870317832789667 ) ) ;
#11448 = VERTEX_POINT ( 'NONE', #4033 ) ;
#11449 = CARTESIAN_POINT ( 'NONE',  ( 10.46960557229346733, 16.46326489517938541, -17.33590790293451178 ) ) ;
#11450 = CARTESIAN_POINT ( 'NONE',  ( 34.06228043176686526, -11.34293828116054037, -19.64761387034043949 ) ) ;
#11451 = CARTESIAN_POINT ( 'NONE',  ( 24.95482030053459965, -6.624749414579512496, -13.76522253407564733 ) ) ;
#11452 = PLANE ( 'NONE',  #17921 ) ;
#11453 = LINE ( 'NONE', #20764, #26438 ) ;
#11454 = CARTESIAN_POINT ( 'NONE',  ( 16.51457045034215199, 5.649390745141357861, -14.67502403374339437 ) ) ;
#11455 = CARTESIAN_POINT ( 'NONE',  ( 23.58034929565730309, -2.629172400889816075, -20.70693660786654888 ) ) ;
#11456 = AXIS2_PLACEMENT_3D ( 'NONE', #16778, #14319, #7769 ) ;
#11457 = VERTEX_POINT ( 'NONE', #18057 ) ;
#11458 = CARTESIAN_POINT ( 'NONE',  ( 166.1922820468853388, -1.999999999999972244, -10.74328820663507678 ) ) ;
#11459 = DIRECTION ( 'NONE',  ( -2.698458740408365879E-16, 1.000000000000000000, 0.000000000000000000 ) ) ;
#11460 = SHAPE_REPRESENTATION ( 'socket head cap screw_iso_ISO 4762 M5 x 20 - 20N', ( #13190 ), #21991 ) ;
#11461 = DIRECTION ( 'NONE',  ( -1.000000000000000000, 0.000000000000000000, 0.000000000000000000 ) ) ;
#11462 = CARTESIAN_POINT ( 'NONE',  ( 154.5152310637605524, -1.999999999999974021, -30.37205893520531319 ) ) ;
#11463 = VECTOR ( 'NONE', #29310, 1000.000000000000000 ) ;
#11464 = CARTESIAN_POINT ( 'NONE',  ( 10.33812163068573575, 18.38616799828327686, -17.90626694547636433 ) ) ;
#11465 = DIRECTION ( 'NONE',  ( -1.000000000000000000, 0.000000000000000000, 0.000000000000000000 ) ) ;
#11466 = ORIENTED_EDGE ( 'NONE', *, *, #17853, .T. ) ;
#11467 = CARTESIAN_POINT ( 'NONE',  ( 0.6543471694412490436, 8.859816792613667502, -0.4964154566688076531 ) ) ;
#11468 = EDGE_LOOP ( 'NONE', ( #14925, #13135, #28504, #18878 ) ) ;
#11469 = CARTESIAN_POINT ( 'NONE',  ( 11.46877092736959014, 9.288109543210406827, -15.86260999805022820 ) ) ;
#11470 = EDGE_CURVE ( 'NONE', #13296, #8969, #9185, .T. ) ;
#11471 = EDGE_CURVE ( 'NONE', #5728, #23514, #27870, .T. ) ;
#11472 = AXIS2_PLACEMENT_3D ( 'NONE', #26335, #28649, #10280 ) ;
#11473 = CARTESIAN_POINT ( 'NONE',  ( 27.66237087416717699, -12.37519551434573017, -14.68082181149132204 ) ) ;
#11474 = LINE ( 'NONE', #11334, #24897 ) ;
#11475 = LINE ( 'NONE', #20792, #21042 ) ;
#11476 = EDGE_CURVE ( 'NONE', #23604, #21626, #16219, .T. ) ;
#11478 = ORIENTED_EDGE ( 'NONE', *, *, #27970, .T. ) ;
#11477 = CARTESIAN_POINT ( 'NONE',  ( 28.12266609392075267, -5.599633216697744942, -16.00068813756295327 ) ) ;
#11479 = ORIENTED_EDGE ( 'NONE', *, *, #20647, .T. ) ;
#11480 = CARTESIAN_POINT ( 'NONE',  ( 16.56108776669977090, -5.000000000000013323, -50.96978717728640618 ) ) ;
#11481 = EDGE_CURVE ( 'NONE', #12783, #18704, #22507, .T. ) ;
#11482 = CARTESIAN_POINT ( 'NONE',  ( 12.51736351114195500, 9.636405190433555035, -15.11633598780129439 ) ) ;
#11483 = ORIENTED_EDGE ( 'NONE', *, *, #11724, .F. ) ;
#11484 = CARTESIAN_POINT ( 'NONE',  ( 33.68411698100747032, -13.80840863474736935, -19.79436191385186916 ) ) ;
#11485 = FACE_OUTER_BOUND ( 'NONE', #25634, .T. ) ;
#11486 = DIRECTION ( 'NONE',  ( -0.8090169943749474513, -2.183098979609982436E-16, -0.5877852522924731371 ) ) ;
#11487 = CARTESIAN_POINT ( 'NONE',  ( 21.08246358516588259, -1.232126404925322438, -18.58940169363586037 ) ) ;
#11488 = ORIENTED_EDGE ( 'NONE', *, *, #7905, .F. ) ;
#11489 = CARTESIAN_POINT ( 'NONE',  ( 176.1922820468853104, -1.999999999999969358, -22.25671179336496053 ) ) ;
#11490 = ORIENTED_EDGE ( 'NONE', *, *, #24414, .F. ) ;
#11491 =( NAMED_UNIT ( * ) SI_UNIT ( $, .STERADIAN. ) SOLID_ANGLE_UNIT ( ) );
#11492 = CARTESIAN_POINT ( 'NONE',  ( 21.37428249720081297, 2.009508332918806151, -14.44682725892062614 ) ) ;
#11493 = CARTESIAN_POINT ( 'NONE',  ( 26.51887141003594195, -6.641914482010843557, -12.47546034222045819 ) ) ;
#11494 = VECTOR ( 'NONE', #26688, 1000.000000000000000 ) ;
#11495 = ORIENTED_EDGE ( 'NONE', *, *, #25327, .T. ) ;
#11496 = CARTESIAN_POINT ( 'NONE',  ( 166.1922820468853672, -9.999999999999996447, -28.06379628232387802 ) ) ;
#11497 = AXIS2_PLACEMENT_3D ( 'NONE', #24991, #2097, #16253 ) ;
#11498 = CARTESIAN_POINT ( 'NONE',  ( 20.00000000000017053, 34.64101615137744972, 14.00000000000000178 ) ) ;
#11499 = VERTEX_POINT ( 'NONE', #29577 ) ;
#11500 = LINE ( 'NONE', #20812, #17351 ) ;
#11501 = CARTESIAN_POINT ( 'NONE',  ( 74.18800000000001660, 7.511012776518211958E-16, -5.000000000000000888 ) ) ;
#11502 = CARTESIAN_POINT ( 'NONE',  ( 158.6922820468853388, -1.999999999999974021, -15.07341522555727664 ) ) ;
#11503 = CARTESIAN_POINT ( 'NONE',  ( 9.641350810849047548, 17.66889113945805789, -17.92015940598198753 ) ) ;
#11504 = CARTESIAN_POINT ( 'NONE',  ( 21.56333733550986409, -5.354713294276967517, -13.65854400988971484 ) ) ;
#11505 = CARTESIAN_POINT ( 'NONE',  ( 20.07445496384854877, 6.874260549971754841, -18.87959640166664954 ) ) ;
#11506 = CARTESIAN_POINT ( 'NONE',  ( 34.52807818452484412, -18.59987926346575549, -21.09179268733712576 ) ) ;
#11507 = CARTESIAN_POINT ( 'NONE',  ( 117.3538932196093185, -4.999999999999985789, -85.26259425104612433 ) ) ;
#11508 = CARTESIAN_POINT ( 'NONE',  ( 12.47535353872619446, 8.560407331872438519, -15.14977315560688176 ) ) ;
#11509 = AXIS2_PLACEMENT_3D ( 'NONE', #10858, #17868, #6295 ) ;
#11510 = LINE ( 'NONE', #4513, #24919 ) ;
#11511 = CARTESIAN_POINT ( 'NONE',  ( 137.0152310637606092, -1.999999999999979572, -24.27857615940569147 ) ) ;
#11512 = EDGE_CURVE ( 'NONE', #20403, #25256, #27196, .T. ) ;
#11513 = CARTESIAN_POINT ( 'NONE',  ( 14.93287775521291394, 9.378568215907955974, -14.88591063491414168 ) ) ;
#11514 = ORIENTED_EDGE ( 'NONE', *, *, #3483, .F. ) ;
#11515 = DIRECTION ( 'NONE',  ( -1.000000000000000000, 0.000000000000000000, 0.000000000000000000 ) ) ;
#11516 = EDGE_CURVE ( 'NONE', #13920, #26554, #23398, .T. ) ;
#11517 = CARTESIAN_POINT ( 'NONE',  ( 10.33811693838771717, 18.38618951776012267, -21.33333333332589632 ) ) ;
#11518 = VERTEX_POINT ( 'NONE', #2515 ) ;
#11519 = VECTOR ( 'NONE', #4182, 1000.000000000000000 ) ;
#11520 = DIRECTION ( 'NONE',  ( 0.000000000000000000, 0.000000000000000000, 1.000000000000000000 ) ) ;
#11521 = CARTESIAN_POINT ( 'NONE',  ( 131.1922820468854241, -10.00000000000000888, -4.936203717676158398 ) ) ;
#11522 = AXIS2_PLACEMENT_3D ( 'NONE', #1745, #13619, #20189 ) ;
#11523 = CARTESIAN_POINT ( 'NONE',  ( 18.21616227284554057, 4.699354889203569918, -13.86658597208997179 ) ) ;
#11524 = ORIENTED_EDGE ( 'NONE', *, *, #14811, .F. ) ;
#11525 = ORIENTED_EDGE ( 'NONE', *, *, #25146, .F. ) ;
#11526 = CARTESIAN_POINT ( 'NONE',  ( 9.274674406624409784, 15.43775921338471413, -16.98767239532306661 ) ) ;
#11527 = CARTESIAN_POINT ( 'NONE',  ( 32.52689891806821265, -10.77327725507678302, -19.81022979934233064 ) ) ;
#11528 = CARTESIAN_POINT ( 'NONE',  ( 17.45108151888110726, 3.014897074772306507, -13.47014999590450479 ) ) ;
#11529 = CARTESIAN_POINT ( 'NONE',  ( 13.40933447586352578, 7.914523597318124715, -14.40541938456405369 ) ) ;
#11530 = LINE ( 'NONE', #26170, #8393 ) ;
#11531 = CARTESIAN_POINT ( 'NONE',  ( 20.11894618883271946, -4.454955732405634805, -18.36807076737963129 ) ) ;
#11532 = ORIENTED_EDGE ( 'NONE', *, *, #28701, .T. ) ;
#11533 = DIRECTION ( 'NONE',  ( -0.000000000000000000, 0.000000000000000000, 1.000000000000000000 ) ) ;
#11534 = EDGE_CURVE ( 'NONE', #23150, #19629, #13504, .T. ) ;
#11536 = ORIENTED_EDGE ( 'NONE', *, *, #23889, .T. ) ;
#11535 = CARTESIAN_POINT ( 'NONE',  ( 4.000000000000019540, 6.928203230275512325, -5.000000000000000888 ) ) ;
#11537 = CIRCLE ( 'NONE', #27204, 3.000000000000002665 ) ;
#11538 = EDGE_LOOP ( 'NONE', ( #18059, #15180, #16182, #19808 ) ) ;
#11539 = CARTESIAN_POINT ( 'NONE',  ( 137.0152310637606092, -4.999999999999980460, -6.958068083716895558 ) ) ;
#11540 = CARTESIAN_POINT ( 'NONE',  ( 420.0000000000002274, 34.64101615137744972, 14.00000000000000178 ) ) ;
#11541 = CARTESIAN_POINT ( 'NONE',  ( 32.11202735699620803, -10.19471129157119194, -14.63100864886716934 ) ) ;
#11542 = CARTESIAN_POINT ( 'NONE',  ( 10.66915452275446619, 9.042499785519874322, -16.41100549784887619 ) ) ;
#11543 = ORIENTED_EDGE ( 'NONE', *, *, #17441, .T. ) ;
#11544 = CARTESIAN_POINT ( 'NONE',  ( 162.0152310637604387, -9.999999999999998224, 1.702185954127501066 ) ) ;
#11545 = CARTESIAN_POINT ( 'NONE',  ( 4.000000000000003553, 2.309401076758525573, -0.3572655899081716435 ) ) ;
#11546 = CARTESIAN_POINT ( 'NONE',  ( 10.35873811938078504, 16.97171716655003593, -17.89325570535168453 ) ) ;
#11547 = DIRECTION ( 'NONE',  ( 0.3090169943749475623, 8.338696094058001131E-17, 0.9510565162951536422 ) ) ;
#11548 = ORIENTED_EDGE ( 'NONE', *, *, #5896, .T. ) ;
#11549 = LINE ( 'NONE', #23164, #22210 ) ;
#11550 = VERTEX_POINT ( 'NONE', #19114 ) ;
#11551 = CARTESIAN_POINT ( 'NONE',  ( 154.5152310637604955, -10.00000000000000178, -2.627941064794695691 ) ) ;
#11552 = AXIS2_PLACEMENT_3D ( 'NONE', #6586, #10998, #30142 ) ;
#11553 = LINE ( 'NONE', #18281, #3498 ) ;
#11554 = ORIENTED_EDGE ( 'NONE', *, *, #14606, .T. ) ;
#11555 = FACE_OUTER_BOUND ( 'NONE', #25813, .T. ) ;
#11556 = EDGE_LOOP ( 'NONE', ( #23885, #25054, #13128, #26538 ) ) ;
#11557 = CARTESIAN_POINT ( 'NONE',  ( 9.797549260427590667, 15.63264415243319938, -17.83144836289601898 ) ) ;
#11558 = VECTOR ( 'NONE', #16291, 1000.000000000000000 ) ;
#11559 = CARTESIAN_POINT ( 'NONE',  ( 21.05341046998850629, -2.558799731849103587, -14.42238450910079806 ) ) ;
#11560 = CARTESIAN_POINT ( 'NONE',  ( 22.79055345825320344, -4.301464833599455417, -14.90020420563294046 ) ) ;
#11561 = ORIENTED_EDGE ( 'NONE', *, *, #24531, .F. ) ;
#11562 = CARTESIAN_POINT ( 'NONE',  ( 19.75232399841803854, 1.290101960903724754, -14.36573431580270999 ) ) ;
#11563 = DIRECTION ( 'NONE',  ( -0.9510565162951536422, -2.566386769018988323E-16, 0.3090169943749475623 ) ) ;
#11564 = DIRECTION ( 'NONE',  ( 0.9510565162951536422, 2.566386769018988816E-16, 0.3090169943749472292 ) ) ;
#11565 = CARTESIAN_POINT ( 'NONE',  ( 158.6922820468853956, -9.999999999999998224, -23.73366926340167637 ) ) ;
#11566 = CARTESIAN_POINT ( 'NONE',  ( 26.72610680620850232, -7.491537437428757329, -18.63066883040512067 ) ) ;
#11567 = LINE ( 'NONE', #28498, #9670 ) ;
#11568 = EDGE_CURVE ( 'NONE', #26251, #5568, #28322, .T. ) ;
#11569 = CARTESIAN_POINT ( 'NONE',  ( 158.6922820468853672, -10.00000000000000000, -17.92658477444275889 ) ) ;
#11570 = EDGE_CURVE ( 'NONE', #28726, #23960, #13917, .T. ) ;
#11571 = FACE_OUTER_BOUND ( 'NONE', #7785, .T. ) ;
#11572 = EDGE_CURVE ( 'NONE', #2975, #10405, #510, .T. ) ;
#11573 = VECTOR ( 'NONE', #21392, 1000.000000000000000 ) ;
#11574 = PLANE ( 'NONE',  #24885 ) ;
#11575 = DIRECTION ( 'NONE',  ( -0.8090169943749474513, -2.183098979609982436E-16, 0.5877852522924731371 ) ) ;
#11576 = EDGE_CURVE ( 'NONE', #29180, #14702, #9799, .T. ) ;
#11577 = CARTESIAN_POINT ( 'NONE',  ( 10.35864919943752405, 16.97212496474457311, -17.91550491156534974 ) ) ;
#11578 = CARTESIAN_POINT ( 'NONE',  ( 164.7287565553229456, -9.999999999999998224, -25.16025403784440329 ) ) ;
#11579 = DIRECTION ( 'NONE',  ( 0.3090169943749475623, 8.338696094058001131E-17, 0.9510565162951536422 ) ) ;
#11580 = VECTOR ( 'NONE', #17724, 1000.000000000000000 ) ;
#11581 = ORIENTED_EDGE ( 'NONE', *, *, #2182, .T. ) ;
#11582 = CARTESIAN_POINT ( 'NONE',  ( 11.22367979475099631, 9.092227732665495665, -17.24169321984975056 ) ) ;
#11583 = ORIENTED_EDGE ( 'NONE', *, *, #19774, .T. ) ;
#11584 = CARTESIAN_POINT ( 'NONE',  ( 164.5152310637604955, -4.999999999999973355, -19.94844914048349693 ) ) ;
#11585 = CARTESIAN_POINT ( 'NONE',  ( 21.42923412144385509, -1.598955984811285536, -13.33006947543598741 ) ) ;
#11586 = CARTESIAN_POINT ( 'NONE',  ( 11.27674754065650653, 16.67436559781366157, -16.78429523206404994 ) ) ;
#11587 = CARTESIAN_POINT ( 'NONE',  ( 35.09336438560361415, -20.13941072448723801, -20.22035334018532637 ) ) ;
#11588 = ORIENTED_EDGE ( 'NONE', *, *, #10104, .T. ) ;
#11589 = EDGE_LOOP ( 'NONE', ( #5098, #8227, #7156, #19467 ) ) ;
#11590 = EDGE_LOOP ( 'NONE', ( #29667, #28089, #11536, #10999, #24010, #116 ) ) ;
#11591 = CARTESIAN_POINT ( 'NONE',  ( 9.917015787971365626, 16.40465641526357743, -16.50431533440121257 ) ) ;
#11592 = LINE ( 'NONE', #22505, #12561 ) ;
#11593 = CARTESIAN_POINT ( 'NONE',  ( 9.641350810849047548, 17.66889113945805789, -17.91928203681695564 ) ) ;
#11594 = DIRECTION ( 'NONE',  ( -0.8090169943749474513, -2.183098979609982436E-16, -0.5877852522924731371 ) ) ;
#11595 = LINE ( 'NONE', #2477, #26229 ) ;
#11596 = EDGE_LOOP ( 'NONE', ( #28165, #20978, #20956, #21821, #2667 ) ) ;
#11597 = CARTESIAN_POINT ( 'NONE',  ( 0.000000000000000000, 0.000000000000000000, -0.5776712190230064436 ) ) ;
#11598 = VERTEX_POINT ( 'NONE', #14220 ) ;
#11599 = CARTESIAN_POINT ( 'NONE',  ( 10.47230989469697882, 16.45086252791593751, -17.33468480047602256 ) ) ;
#11600 = CARTESIAN_POINT ( 'NONE',  ( 34.16709027601721971, -12.48568152589075098, -20.91241392730897886 ) ) ;
#11601 = CARTESIAN_POINT ( 'NONE',  ( 24.60501232743784783, -9.531698448777172317, -16.22453333552994792 ) ) ;
#11602 = ORIENTED_EDGE ( 'NONE', *, *, #26601, .F. ) ;
#11603 = AXIS2_PLACEMENT_3D ( 'NONE', #19215, #19369, #2918 ) ;
#11604 = DIRECTION ( 'NONE',  ( -0.5877852522924731371, 0.000000000000000000, 0.8090169943749474513 ) ) ;
#11605 = CARTESIAN_POINT ( 'NONE',  ( 4.000000000000000000, 0.3904826640788077730, 4.917026258811211496E-16 ) ) ;
#11606 = ORIENTED_EDGE ( 'NONE', *, *, #30257, .F. ) ;
#11607 = CARTESIAN_POINT ( 'NONE',  ( 19.47111902912460124, 6.782054727477878409, -15.90798308235397407 ) ) ;
#11608 = VECTOR ( 'NONE', #20585, 1000.000000000000000 ) ;
#11609 = CARTESIAN_POINT ( 'NONE',  ( 27.54771222089439320, -11.35863810494041459, -14.08592588049474692 ) ) ;
#11610 = AXIS2_PLACEMENT_3D ( 'NONE', #9274, #16456, #23330 ) ;
#11611 = ORIENTED_EDGE ( 'NONE', *, *, #21000, .T. ) ;
#11612 = CARTESIAN_POINT ( 'NONE',  ( 157.0152310637605240, -9.999999999999998224, -26.04193191628311155 ) ) ;
#11613 = EDGE_CURVE ( 'NONE', #29774, #7167, #14520, .T. ) ;
#11614 = CIRCLE ( 'NONE', #3362, 5.000000000000000888 ) ;
#11615 = EDGE_CURVE ( 'NONE', #11457, #2772, #7517, .T. ) ;
#11616 = EDGE_CURVE ( 'NONE', #24955, #19224, #19254, .T. ) ;
#11617 = EDGE_CURVE ( 'NONE', #25465, #5840, #23863, .T. ) ;
#11618 = EDGE_LOOP ( 'NONE', ( #29498, #6490, #24341, #13022 ) ) ;
#11619 = DIRECTION ( 'NONE',  ( 0.3090169943749472292, 8.338696094057992503E-17, -0.9510565162951536422 ) ) ;
#11620 = FACE_OUTER_BOUND ( 'NONE', #5287, .T. ) ;
#11621 = DIRECTION ( 'NONE',  ( -2.698458740408365879E-16, 1.000000000000000000, 0.000000000000000000 ) ) ;
#11622 = UNCERTAINTY_MEASURE_WITH_UNIT (LENGTH_MEASURE( 1.000000000000000082E-05 ), #29747, 'distance_accuracy_value', 'NONE');
#11623 = CARTESIAN_POINT ( 'NONE',  ( 10.72074420406304895, 16.63141210374104872, -15.95421917676928025 ) ) ;
#11624 = CARTESIAN_POINT ( 'NONE',  ( 10.00000000000008527, 17.32050807568872486, -23.00000000000000000 ) ) ;
#11625 = VECTOR ( 'NONE', #731, 1000.000000000000000 ) ;
#11626 = FACE_OUTER_BOUND ( 'NONE', #29283, .T. ) ;
#11627 = ORIENTED_EDGE ( 'NONE', *, *, #892, .F. ) ;
#11628 = CARTESIAN_POINT ( 'NONE',  ( 10.82443827553465177, 12.24310121783546634, -16.12906421532448675 ) ) ;
#11629 = CARTESIAN_POINT ( 'NONE',  ( 17.11242430243909141, 7.828829022555451544, -19.39938683153768295 ) ) ;
#11630 = CARTESIAN_POINT ( 'NONE',  ( 12.03194932440650966, -5.000000000000014211, 37.03053235585281300 ) ) ;
#11631 = DIRECTION ( 'NONE',  ( -2.698458740408365879E-16, 1.000000000000000000, 0.000000000000000000 ) ) ;
#11633 = ORIENTED_EDGE ( 'NONE', *, *, #15559, .F. ) ;
#11632 = CARTESIAN_POINT ( 'NONE',  ( 28.06689949639850212, -8.111051215268487269, -13.49421662364394514 ) ) ;
#11634 = VECTOR ( 'NONE', #24473, 1000.000000000000000 ) ;
#11635 = ORIENTED_EDGE ( 'NONE', *, *, #6513, .F. ) ;
#11636 = DIRECTION ( 'NONE',  ( -0.9510565162951536422, -2.566386769018988816E-16, -0.3090169943749472292 ) ) ;
#11637 = CARTESIAN_POINT ( 'NONE',  ( 11.27564905058850719, 16.67940341329043363, -16.78475148866115774 ) ) ;
#11638 = ORIENTED_EDGE ( 'NONE', *, *, #7539, .T. ) ;
#11639 = CLOSED_SHELL ( 'NONE', ( #25218, #14053, #29257, #21600, #13443, #23039, #4910, #19517, #12682, #4813, #8110, #28452, #20239, #18982, #9167, #17821, #25490, #27932, #10174, #18521, #12410, #14776, #7708, #26671, #18336, #21424, #24444, #16583, #19775, #13037, #23458, #67, #1972 ) ) ;
#11640 = CARTESIAN_POINT ( 'NONE',  ( 35.49237112349044310, -21.93193663806729887, -19.32748734164077931 ) ) ;
#11641 = DIRECTION ( 'NONE',  ( 0.000000000000000000, 0.000000000000000000, -1.000000000000000000 ) ) ;
#11642 = DIRECTION ( 'NONE',  ( 1.000000000000000000, 2.698458740408365879E-16, -1.110223024625156540E-16 ) ) ;
#11643 = CARTESIAN_POINT ( 'NONE',  ( 31.14759003376246582, -7.259970019232452998, -15.53234487094253069 ) ) ;
#11644 = ORIENTED_EDGE ( 'NONE', *, *, #713, .F. ) ;
#11645 = CARTESIAN_POINT ( 'NONE',  ( 142.0152310637605808, -4.999999999999978684, -6.958068083716895558 ) ) ;
#11646 = CARTESIAN_POINT ( 'NONE',  ( 16.63724033897865340, 2.930722838386041751, -15.17604395537502526 ) ) ;
#11647 = CARTESIAN_POINT ( 'NONE',  ( 27.40270966038060152, -12.25096941946872953, -16.90735844088681006 ) ) ;
#11648 = ORIENTED_EDGE ( 'NONE', *, *, #5154, .T. ) ;
#11649 = FACE_OUTER_BOUND ( 'NONE', #16752, .T. ) ;
#11650 = AXIS2_PLACEMENT_3D ( 'NONE', #29206, #8246, #26909 ) ;
#11651 = EDGE_CURVE ( 'NONE', #20109, #16265, #27695, .T. ) ;
#11652 = EDGE_CURVE ( 'NONE', #8269, #10703, #20944, .T. ) ;
#11653 = ADVANCED_FACE ( 'NONE', ( #2653 ), #28169, .T. ) ;
#11654 = DIRECTION ( 'NONE',  ( 0.000000000000000000, 0.000000000000000000, 1.000000000000000000 ) ) ;
#11655 = CIRCLE ( 'NONE', #6824, 12.50000000000000000 ) ;
#11656 = EDGE_CURVE ( 'NONE', #319, #15181, #11928, .T. ) ;
#11657 = DIRECTION ( 'NONE',  ( -0.000000000000000000, -0.000000000000000000, 1.000000000000000000 ) ) ;
#11658 = CARTESIAN_POINT ( 'NONE',  ( 142.0152310637605524, -1.999999999999978462, -8.721423840594312082 ) ) ;
#11659 = FACE_OUTER_BOUND ( 'NONE', #2224, .T. ) ;
#11660 = CARTESIAN_POINT ( 'NONE',  ( 9.916551108984865692, 16.40678749232849398, -16.50450761325770443 ) ) ;
#11661 = CARTESIAN_POINT ( 'NONE',  ( 24.41106252871404436, -7.915231898853421377, -13.94454578273958667 ) ) ;
#11662 = CARTESIAN_POINT ( 'NONE',  ( 22.45293885382703536, -0.3771200753331621081, -14.01028023225368635 ) ) ;
#11664 = EDGE_LOOP ( 'NONE', ( #30136, #1644, #29797, #24089 ) ) ;
#11663 = CARTESIAN_POINT ( 'NONE',  ( 36.54859390954302967, -23.18451583373416014, -15.55638201429745848 ) ) ;
#11665 = FILL_AREA_STYLE ('',( #28045 ) ) ;
#11666 = CARTESIAN_POINT ( 'NONE',  ( 15.00000000000000000, 4.735455214955320607E-16, 5.000000000000000000 ) ) ;
#11667 = LINE ( 'NONE', #27902, #27405 ) ;
#11668 = CARTESIAN_POINT ( 'NONE',  ( 0.000000000000000000, 0.000000000000000000, 15.00000000000000000 ) ) ;
#11669 = CARTESIAN_POINT ( 'NONE',  ( 17.95327243003904982, 7.812726124483462264, -14.88485059575767266 ) ) ;
#11670 = VERTEX_POINT ( 'NONE', #7381 ) ;
#11671 = DIRECTION ( 'NONE',  ( 0.9510565162951536422, 0.000000000000000000, -0.3090169943749475623 ) ) ;
#11672 = CARTESIAN_POINT ( 'NONE',  ( 10.73702987185851931, 16.55672395529124330, -15.94748436097269817 ) ) ;
#11673 = VERTEX_POINT ( 'NONE', #362 ) ;
#11674 = CARTESIAN_POINT ( 'NONE',  ( 0.000000000000000000, 0.000000000000000000, 0.000000000000000000 ) ) ;
#11675 = DIRECTION ( 'NONE',  ( -2.698458740408365879E-16, 1.000000000000000000, 0.000000000000000000 ) ) ;
#11676 = CARTESIAN_POINT ( 'NONE',  ( 15.70491959545049987, 3.570626008024105680, -15.63470537622339229 ) ) ;
#11677 = ORIENTED_EDGE ( 'NONE', *, *, #23632, .F. ) ;
#11678 = VECTOR ( 'NONE', #8810, 1000.000000000000000 ) ;
#11679 = CARTESIAN_POINT ( 'NONE',  ( 25.18430082464795916, -12.47910854170484818, -17.34997305645471855 ) ) ;
#11680 = VECTOR ( 'NONE', #3758, 1000.000000000000000 ) ;
#11681 = VERTEX_POINT ( 'NONE', #16522 ) ;
#11682 = CARTESIAN_POINT ( 'NONE',  ( 33.74345058881453241, -15.07496310474945922, -20.85461858825047798 ) ) ;
#11683 = CARTESIAN_POINT ( 'NONE',  ( 22.42041779846375604, -0.009017426515379003624, -18.82878497401882001 ) ) ;
#11684 = CARTESIAN_POINT ( 'NONE',  ( 16.51457045034215199, 5.649390745141357861, -14.67502403374339437 ) ) ;
#11685 = CARTESIAN_POINT ( 'NONE',  ( 30.29779709953443501, -9.168887887504279632, -16.05354238668875055 ) ) ;
#11686 = MANIFOLD_SOLID_BREP ( 'TorqueElement', #11639 ) ;
#11687 = EDGE_CURVE ( 'NONE', #23514, #3855, #5533, .T. ) ;
#11688 = ORIENTED_EDGE ( 'NONE', *, *, #2346, .T. ) ;
#11689 = EDGE_CURVE ( 'NONE', #653, #5008, #3296, .T. ) ;
#11690 = CARTESIAN_POINT ( 'NONE',  ( 130.7287565553229456, -4.999999999999983125, 0.5000000000000052180 ) ) ;
#11691 = AXIS2_PLACEMENT_3D ( 'NONE', #9468, #19091, #2185 ) ;
#11692 = EDGE_CURVE ( 'NONE', #14061, #17928, #29155, .T. ) ;
#11693 = VECTOR ( 'NONE', #28776, 1000.000000000000000 ) ;
#11695 = ORIENTED_EDGE ( 'NONE', *, *, #25044, .F. ) ;
#11694 = DIRECTION ( 'NONE',  ( -2.698458740408365879E-16, 1.000000000000000000, 0.000000000000000000 ) ) ;
#11696 = EDGE_LOOP ( 'NONE', ( #2415, #29943, #8469, #4056, #24123 ) ) ;
#11697 = FACE_OUTER_BOUND ( 'NONE', #8382, .T. ) ;
#11698 = LINE ( 'NONE', #9400, #24863 ) ;
#11699 = CARTESIAN_POINT ( 'NONE',  ( 36.19723272591463115, -19.60603615691276858, -19.44143419077989421 ) ) ;
#11700 = CARTESIAN_POINT ( 'NONE',  ( 12.82404076521984670, 7.655871835264917102, -14.87190880308183871 ) ) ;
#11701 = VERTEX_POINT ( 'NONE', #1413 ) ;
#11702 = PLANE ( 'NONE',  #20488 ) ;
#11703 = PLANE ( 'NONE',  #12824 ) ;
#11704 = CARTESIAN_POINT ( 'NONE',  ( 10.41412541532089620, 16.71770396712979689, -17.42473314453425814 ) ) ;
#11705 = CARTESIAN_POINT ( 'NONE',  ( 172.7287565553229456, -4.999999999999970690, 0.5000000000000029976 ) ) ;
#11706 = DIRECTION ( 'NONE',  ( -0.9510565162951536422, 0.000000000000000000, -0.3090169943749472292 ) ) ;
#11707 = VECTOR ( 'NONE', #9566, 1000.000000000000000 ) ;
#11708 = VERTEX_POINT ( 'NONE', #20015 ) ;
#11709 = AXIS2_PLACEMENT_3D ( 'NONE', #22954, #20639, #16974 ) ;
#11710 = DIRECTION ( 'NONE',  ( -1.110223024625156540E-16, 0.000000000000000000, -1.000000000000000000 ) ) ;
#11711 = FACE_OUTER_BOUND ( 'NONE', #4052, .T. ) ;
#11712 = FACE_OUTER_BOUND ( 'NONE', #12981, .T. ) ;
#11713 = ORIENTED_EDGE ( 'NONE', *, *, #5368, .F. ) ;
#11714 = CARTESIAN_POINT ( 'NONE',  ( 9.667864356596815867, 16.22739565238121529, -17.88507765419223716 ) ) ;
#11715 = ADVANCED_FACE ( 'NONE', ( #961 ), #12533, .T. ) ;
#11716 = VECTOR ( 'NONE', #23188, 1000.000000000000000 ) ;
#11717 = CARTESIAN_POINT ( 'NONE',  ( 23.17017814088865535, -4.132587038751921682, -14.65442522582375240 ) ) ;
#11718 = CARTESIAN_POINT ( 'NONE',  ( 24.81022290780906658, -1.767900772465358372, -17.79475844156381470 ) ) ;
#11719 = CARTESIAN_POINT ( 'NONE',  ( 21.10828700581006601, 3.717818950362942854, -18.90958453460783417 ) ) ;
#11720 = CARTESIAN_POINT ( 'NONE',  ( 167.2287565553229740, -1.999999999999970468, -29.49038105676660493 ) ) ;
#11721 = CARTESIAN_POINT ( 'NONE',  ( 174.5152310637604671, -9.999999999999994671, -19.94844914048349693 ) ) ;
#11722 = CARTESIAN_POINT ( 'NONE',  ( 159.7287565553230024, -1.999999999999972244, -33.82050807568879947 ) ) ;
#11723 = CARTESIAN_POINT ( 'NONE',  ( 27.95388715220626707, -5.541385876428546631, -15.41148221666858831 ) ) ;
#11724 = EDGE_CURVE ( 'NONE', #6838, #6429, #24602, .T. ) ;
#11725 = FACE_OUTER_BOUND ( 'NONE', #3566, .T. ) ;
#11726 = CIRCLE ( 'NONE', #3012, 0.2000000000000000944 ) ;
#11727 = CARTESIAN_POINT ( 'NONE',  ( 144.5152310637605808, -4.999999999999978684, -21.71180489736091346 ) ) ;
#11728 = FACE_BOUND ( 'NONE', #24152, .T. ) ;
#11729 = VECTOR ( 'NONE', #19631, 1000.000000000000000 ) ;
#11730 = CARTESIAN_POINT ( 'NONE',  ( 15.68512135455575596, -5.000000000000013323, -48.27383977151229999 ) ) ;
#11731 = LINE ( 'NONE', #4870, #8949 ) ;
#11732 = CARTESIAN_POINT ( 'NONE',  ( 10.38089682401341385, 16.87009452252716102, -17.57504515238516873 ) ) ;
#11734 = VERTEX_POINT ( 'NONE', #19705 ) ;
#11733 = CARTESIAN_POINT ( 'NONE',  ( 35.54859390953724585, -22.18451583373416014, -18.06010107863414405 ) ) ;
#11735 = CARTESIAN_POINT ( 'NONE',  ( 32.89062095351589932, -11.25267498498577723, -18.96775996542842435 ) ) ;
#11736 = ORIENTED_EDGE ( 'NONE', *, *, #1203, .T. ) ;
#11737 = CARTESIAN_POINT ( 'NONE',  ( 8.944584694422324844, 16.95159271019519664, -17.91554756312530117 ) ) ;
#11738 = ORIENTED_EDGE ( 'NONE', *, *, #4234, .F. ) ;
#11739 = CARTESIAN_POINT ( 'NONE',  ( 142.0152310637605808, -10.00000000000000355, -34.70218595412750773 ) ) ;
#11740 = CARTESIAN_POINT ( 'NONE',  ( 23.36212950203212557, 2.915605996956767587, -15.34809340432955693 ) ) ;
#11741 = CARTESIAN_POINT ( 'NONE',  ( 11.20364811077027767, 17.00960890128215297, -16.86645280501126365 ) ) ;
#11742 = PLANE ( 'NONE',  #21428 ) ;
#11743 = EDGE_LOOP ( 'NONE', ( #26825, #1585, #15044, #26007 ) ) ;
#11744 = ORIENTED_EDGE ( 'NONE', *, *, #29533, .F. ) ;
#11745 = VERTEX_POINT ( 'NONE', #10706 ) ;
#11746 = CARTESIAN_POINT ( 'NONE',  ( 9.917965570771830386, 16.40030059027150600, -16.50392256580263606 ) ) ;
#11747 = DIRECTION ( 'NONE',  ( -2.698458740408365879E-16, 1.000000000000000000, 0.000000000000000000 ) ) ;
#11748 = CARTESIAN_POINT ( 'NONE',  ( 9.957223259857686415, 16.22025982393231303, -16.48768813039480818 ) ) ;
#11749 = CARTESIAN_POINT ( 'NONE',  ( 4.317446301598349301, -5.000000000000016875, 13.28773340506741896 ) ) ;
#11750 = DIRECTION ( 'NONE',  ( 0.9510565162951536422, 0.000000000000000000, -0.3090169943749475623 ) ) ;
#11751 = VERTEX_POINT ( 'NONE', #8409 ) ;
#11752 = CARTESIAN_POINT ( 'NONE',  ( 133.6922820468854241, -1.999999999999981348, -17.92658477444275533 ) ) ;
#11753 = VERTEX_POINT ( 'NONE', #17416 ) ;
#11754 = CARTESIAN_POINT ( 'NONE',  ( 10.53683180627515981, 16.15495681678771689, -17.30800272034635867 ) ) ;
#11755 = EDGE_CURVE ( 'NONE', #1753, #2498, #10547, .T. ) ;
#11756 = ORIENTED_EDGE ( 'NONE', *, *, #7531, .F. ) ;
#11758 = VECTOR ( 'NONE', #25893, 1000.000000000000000 ) ;
#11757 = CARTESIAN_POINT ( 'NONE',  ( 32.09732368354767118, -9.542663571685382706, -16.59113971387166941 ) ) ;
#11759 = CARTESIAN_POINT ( 'NONE',  ( 25.97256211245905533, -8.171536508395311316, -18.54953510021574559 ) ) ;
#11760 = ADVANCED_FACE ( 'NONE', ( #26300 ), #5833, .T. ) ;
#11761 = DIRECTION ( 'NONE',  ( -0.000000000000000000, -0.000000000000000000, -1.000000000000000000 ) ) ;
#11762 = CARTESIAN_POINT ( 'NONE',  ( 33.28625081342995884, -10.37305140221732991, -17.94975064729133862 ) ) ;
#11763 = DIRECTION ( 'NONE',  ( 0.000000000000000000, 0.000000000000000000, 1.000000000000000000 ) ) ;
#11764 = ORIENTED_EDGE ( 'NONE', *, *, #18000, .F. ) ;
#11765 = CARTESIAN_POINT ( 'NONE',  ( 27.62103240953636174, -12.62788667074165794, -13.46147607715242245 ) ) ;
#11766 = CARTESIAN_POINT ( 'NONE',  ( 29.25528888857379783, -9.059906918047152757, -17.02304095575280130 ) ) ;
#11767 = ORIENTED_EDGE ( 'NONE', *, *, #24908, .F. ) ;
#11768 = FACE_BOUND ( 'NONE', #3639, .T. ) ;
#11769 = VECTOR ( 'NONE', #11187, 1000.000000000000000 ) ;
#11770 = CARTESIAN_POINT ( 'NONE',  ( 169.5152310637604671, -1.999999999999970468, -21.71180489736091346 ) ) ;
#11771 = LINE ( 'NONE', #16963, #22393 ) ;
#11772 = CARTESIAN_POINT ( 'NONE',  ( 9.964222036193500998, -5.000000000000015099, 30.66672212155160793 ) ) ;
#11773 = CARTESIAN_POINT ( 'NONE',  ( 10.35008142444812052, 18.33131885956999696, -17.43324812465761653 ) ) ;
#11774 = LINE ( 'NONE', #7217, #10930 ) ;
#11775 = DIRECTION ( 'NONE',  ( 1.000000000000000000, 0.000000000000000000, 0.000000000000000000 ) ) ;
#11776 = ORIENTED_EDGE ( 'NONE', *, *, #29652, .F. ) ;
#11777 = CARTESIAN_POINT ( 'NONE',  ( 9.936961226781097167, 16.31318409042999917, -16.49606719383117337 ) ) ;
#11778 = EDGE_LOOP ( 'NONE', ( #4115, #25925, #15484, #19634 ) ) ;
#11779 = TOROIDAL_SURFACE ( 'NONE', #1100, 4.000000000000000000, 0.2500000000000000000 ) ;
#11780 = CARTESIAN_POINT ( 'NONE',  ( 16.16754939756797782, 8.873905313537072459, -14.69432754670026142 ) ) ;
#11781 = CARTESIAN_POINT ( 'NONE',  ( 13.46432186659439800, -5.000000000000014211, 41.43892174804634010 ) ) ;
#11782 = CARTESIAN_POINT ( 'NONE',  ( 13.13993655228012436, -5.000000000000014211, -40.44056640647991685 ) ) ;
#11783 = VERTEX_POINT ( 'NONE', #26452 ) ;
#11784 = CARTESIAN_POINT ( 'NONE',  ( 26.92971693216691165, -8.617903733377630715, -13.36642543767191427 ) ) ;
#11785 = ORIENTED_EDGE ( 'NONE', *, *, #12252, .T. ) ;
#11786 = DIRECTION ( 'NONE',  ( -0.5877852522924731371, 0.000000000000000000, 0.8090169943749474513 ) ) ;
#11787 = CARTESIAN_POINT ( 'NONE',  ( 11.27553273857261296, 16.67993683502164615, -16.78480078315762469 ) ) ;
#11788 = ORIENTED_EDGE ( 'NONE', *, *, #18593, .F. ) ;
#11789 = EDGE_CURVE ( 'NONE', #23642, #1088, #19855, .T. ) ;
#11790 = CARTESIAN_POINT ( 'NONE',  ( 33.30991885831043220, -11.83535627117299960, -18.22721479198959926 ) ) ;
#11791 = CARTESIAN_POINT ( 'NONE',  ( 16.53342136567307108, 10.04554801986687629, -15.32032680638607047 ) ) ;
#11792 = EDGE_CURVE ( 'NONE', #18131, #27161, #24452, .T. ) ;
#11793 = CARTESIAN_POINT ( 'NONE',  ( 130.7287565553229172, -4.999999999999983125, -22.10610323145025902 ) ) ;
#11794 = AXIS2_PLACEMENT_3D ( 'NONE', #14159, #5319, #2446 ) ;
#11795 = ADVANCED_FACE ( 'NONE', ( #3693 ), #26920, .T. ) ;
#11796 = CARTESIAN_POINT ( 'NONE',  ( 27.35338705259445646, -4.307586880325415812, -13.99634582963401996 ) ) ;
#11797 = ORIENTED_EDGE ( 'NONE', *, *, #20705, .F. ) ;
#11798 = FACE_OUTER_BOUND ( 'NONE', #25671, .T. ) ;
#11799 = CARTESIAN_POINT ( 'NONE',  ( 18.97628335640213493, 0.9430780577607489334, -14.77698032187241850 ) ) ;
#11800 = CARTESIAN_POINT ( 'NONE',  ( 15.31194320040279777, 8.488938064892046498, -14.62880434596509183 ) ) ;
#11801 = EDGE_LOOP ( 'NONE', ( #10398, #6919, #11233, #20175 ) ) ;
#11802 = ORIENTED_EDGE ( 'NONE', *, *, #29888, .F. ) ;
#11803 = CARTESIAN_POINT ( 'NONE',  ( 175.7287565553229456, -4.999999999999970690, 3.500000000000003109 ) ) ;
#11804 = VECTOR ( 'NONE', #1891, 1000.000000000000000 ) ;
#11805 = CARTESIAN_POINT ( 'NONE',  ( 167.2287565553228887, -9.999999999999998224, -3.509618943233403510 ) ) ;
#11806 = LINE ( 'NONE', #21123, #2261 ) ;
#11807 = CARTESIAN_POINT ( 'NONE',  ( 133.7287565553229456, -4.999999999999981348, 0.5000000000000029976 ) ) ;
#11808 = ORIENTED_EDGE ( 'NONE', *, *, #23802, .T. ) ;
#11809 = CARTESIAN_POINT ( 'NONE',  ( 25.00000000000000000, 2.055000000000001492, 0.000000000000000000 ) ) ;
#11810 = VECTOR ( 'NONE', #18258, 1000.000000000000000 ) ;
#11811 = CARTESIAN_POINT ( 'NONE',  ( 9.917965570771830386, 16.40030059027150600, -16.50392256580263606 ) ) ;
#11812 = CARTESIAN_POINT ( 'NONE',  ( 25.61803826562323394, -0.4625480611756047078, -19.10237625710802334 ) ) ;
#11813 = CARTESIAN_POINT ( 'NONE',  ( 22.84118038848623655, 1.850029439873439152, -18.07216660426987431 ) ) ;
#11814 = EDGE_CURVE ( 'NONE', #18644, #6532, #19558, .T. ) ;
#11816 = VERTEX_POINT ( 'NONE', #22011 ) ;
#11815 = CARTESIAN_POINT ( 'NONE',  ( 31.95629010954621663, -10.29636179124881679, -18.42443288805318247 ) ) ;
#11817 = CARTESIAN_POINT ( 'NONE',  ( 9.009307008068239142, -5.000000000000015099, 27.72779586008924468 ) ) ;
#11818 = DIRECTION ( 'NONE',  ( 0.9510565162951535312, 2.566386769018988816E-16, -0.3090169943749475623 ) ) ;
#11819 = LINE ( 'NONE', #19003, #2534 ) ;
#11820 = DIRECTION ( 'NONE',  ( -2.698458740408365879E-16, 1.000000000000000000, 0.000000000000000000 ) ) ;
#11821 = CARTESIAN_POINT ( 'NONE',  ( 17.66155849027303049, 7.702290371990539342, -14.74052880078125760 ) ) ;
#11822 = ORIENTED_EDGE ( 'NONE', *, *, #13011, .F. ) ;
#11823 = PLANE ( 'NONE',  #20758 ) ;
#11824 = CARTESIAN_POINT ( 'NONE',  ( 10.52543090623380451, 17.52714378424053265, -16.25779133722369707 ) ) ;
#11825 = VERTEX_POINT ( 'NONE', #19406 ) ;
#11826 = CARTESIAN_POINT ( 'NONE',  ( 144.5152310637605808, -4.999999999999978684, -1.604441369360116507E-14 ) ) ;
#11827 = DIRECTION ( 'NONE',  ( -0.9510565162951536422, 0.000000000000000000, -0.3090169943749472292 ) ) ;
#11828 = EDGE_CURVE ( 'NONE', #13853, #8269, #14967, .T. ) ;
#11829 = CARTESIAN_POINT ( 'NONE',  ( 21.64656857049893901, 5.639188926465734220, -17.17864421186117951 ) ) ;
#11830 = EDGE_CURVE ( 'NONE', #28906, #11448, #803, .T. ) ;
#11831 = EDGE_CURVE ( 'NONE', #26232, #13323, #7818, .T. ) ;
#11832 = CARTESIAN_POINT ( 'NONE',  ( 29.95565488329840775, -10.73317148848732039, -11.80569981112315325 ) ) ;
#11833 = VERTEX_POINT ( 'NONE', #22469 ) ;
#11834 = EDGE_CURVE ( 'NONE', #25350, #11270, #2023, .T. ) ;
#11835 = CARTESIAN_POINT ( 'NONE',  ( 35.53993026725221682, -23.14559467820676275, -18.82474504553469075 ) ) ;
#11836 = CARTESIAN_POINT ( 'NONE',  ( 22.40466763571637543, -1.191653471825661059, -14.65485681160645548 ) ) ;
#11837 = CARTESIAN_POINT ( 'NONE',  ( 17.95893182911733277, 3.791778598950861667, -15.25628287466289024 ) ) ;
#11838 = AXIS2_PLACEMENT_3D ( 'NONE', #21800, #19501, #28871 ) ;
#11839 = CARTESIAN_POINT ( 'NONE',  ( 26.13670795350922660, -6.813068953109826076, -12.41955265015470999 ) ) ;
#11840 = MANIFOLD_SOLID_BREP ( 'Fillet1', #24820 ) ;
#11841 = ORIENTED_EDGE ( 'NONE', *, *, #5635, .F. ) ;
#11842 = CARTESIAN_POINT ( 'NONE',  ( -8.000000000000001776, -4.336808689942017736E-15, -5.000000000000000888 ) ) ;
#11843 = ORIENTED_EDGE ( 'NONE', *, *, #18758, .T. ) ;
#11844 = CARTESIAN_POINT ( 'NONE',  ( 133.6922820468854241, -1.999999999999981348, -26.58683881228715506 ) ) ;
#11845 = DIRECTION ( 'NONE',  ( 1.110223024625156540E-16, 2.995891024602366092E-32, 1.000000000000000000 ) ) ;
#11846 = DIRECTION ( 'NONE',  ( 0.000000000000000000, 0.000000000000000000, 1.000000000000000000 ) ) ;
#11847 = CARTESIAN_POINT ( 'NONE',  ( 36.54816482920796972, -21.18258820310476409, -18.41547799146826847 ) ) ;
#11848 = CARTESIAN_POINT ( 'NONE',  ( 12.79001206111077948, 7.640833942120977440, -14.89903028090515136 ) ) ;
#11849 = ORIENTED_EDGE ( 'NONE', *, *, #15593, .T. ) ;
#11850 = AXIS2_PLACEMENT_3D ( 'NONE', #18080, #4204, #27441 ) ;
#11851 = CARTESIAN_POINT ( 'NONE',  ( 172.7287565553229456, -1.999999999999970468, 6.499999999999977796 ) ) ;
#11852 = CARTESIAN_POINT ( 'NONE',  ( 149.5152310637605240, -1.999999999999976685, -2.627941064794695691 ) ) ;
#11853 = CARTESIAN_POINT ( 'NONE',  ( 10.47139596700049147, 16.45505391683073526, -17.33506929010674114 ) ) ;
#11854 = DIRECTION ( 'NONE',  ( 0.5877852522924731371, 1.586114251531760728E-16, -0.8090169943749474513 ) ) ;
#11855 = ORIENTED_EDGE ( 'NONE', *, *, #26747, .F. ) ;
#11856 = DIRECTION ( 'NONE',  ( 1.000000000000000000, 0.000000000000000000, 0.000000000000000000 ) ) ;
#11857 = VERTEX_POINT ( 'NONE', #25206 ) ;
#11858 = CARTESIAN_POINT ( 'NONE',  ( 0.000000000000000000, 0.000000000000000000, -5.000000000000000888 ) ) ;
#11859 = ADVANCED_FACE ( 'NONE', ( #9000 ), #8856, .T. ) ;
#11860 = DIRECTION ( 'NONE',  ( -0.8090169943749474513, -2.183098979609982436E-16, 0.5877852522924731371 ) ) ;
#11861 = EDGE_CURVE ( 'NONE', #12653, #15277, #13140, .T. ) ;
#11862 = CARTESIAN_POINT ( 'NONE',  ( 173.6922820468852819, -1.999999999999970024, -15.07341522555727664 ) ) ;
#11863 = VERTEX_POINT ( 'NONE', #22614 ) ;
#11864 = EDGE_CURVE ( 'NONE', #23355, #18808, #16030, .T. ) ;
#11865 = CARTESIAN_POINT ( 'NONE',  ( 9.667069921042207525, 16.23103903510144619, -17.88562738470040969 ) ) ;
#11866 = CARTESIAN_POINT ( 'NONE',  ( 25.35799213500633442, -5.391047399292974163, -13.97031313328441726 ) ) ;
#11867 = CARTESIAN_POINT ( 'NONE',  ( 20.97044927184332508, -4.289323992320570156, -15.06659861376252429 ) ) ;
#11868 = LINE ( 'NONE', #11720, #12568 ) ;
#11869 = LINE ( 'NONE', #1726, #29235 ) ;
#11870 = CARTESIAN_POINT ( 'NONE',  ( 158.6922820468853104, -10.00000000000000000, 2.247092850131519715 ) ) ;
#11871 = CARTESIAN_POINT ( 'NONE',  ( 21.43917814492346707, -4.799604530101110988, -17.97822123721208243 ) ) ;
#11872 = VECTOR ( 'NONE', #25788, 1000.000000000000000 ) ;
#11873 = ORIENTED_EDGE ( 'NONE', *, *, #20443, .T. ) ;
#11874 = CARTESIAN_POINT ( 'NONE',  ( 169.7287565553228603, -4.999999999999971578, 0.8205080756888000204 ) ) ;
#11875 = CARTESIAN_POINT ( 'NONE',  ( 131.1922820468854241, -10.00000000000000888, -10.74328820663507322 ) ) ;
#11876 = FACE_OUTER_BOUND ( 'NONE', #4187, .T. ) ;
#11877 = PLANE ( 'NONE',  #28990 ) ;
#11878 = CARTESIAN_POINT ( 'NONE',  ( 10.60167031212029443, 15.85759916399494607, -17.28118971735050735 ) ) ;
#11879 = EDGE_CURVE ( 'NONE', #28015, #17495, #11443, .T. ) ;
#11880 = LINE ( 'NONE', #7174, #29713 ) ;
#11881 = CARTESIAN_POINT ( 'NONE',  ( 33.96943610671532809, -15.09019632882451134, -19.88060704079178720 ) ) ;
#11882 = ORIENTED_EDGE ( 'NONE', *, *, #11616, .T. ) ;
#11883 = CARTESIAN_POINT ( 'NONE',  ( 13.38265815842314943, 7.627299838292535661, -15.70544478996546900 ) ) ;
#11884 = EDGE_LOOP ( 'NONE', ( #2803, #19577, #18428, #25733 ) ) ;
#11885 = FACE_OUTER_BOUND ( 'NONE', #25961, .T. ) ;
#11886 = CARTESIAN_POINT ( 'NONE',  ( 22.39939798857497877, 2.694615832958070722, -14.02792042734668065 ) ) ;
#11887 = CARTESIAN_POINT ( 'NONE',  ( 11.27624053946810889, 16.67669076989127674, -16.78450489582619554 ) ) ;
#11888 = FACE_BOUND ( 'NONE', #25094, .T. ) ;
#11889 = ORIENTED_EDGE ( 'NONE', *, *, #12215, .F. ) ;
#11890 = CARTESIAN_POINT ( 'NONE',  ( 9.641359250860388030, 17.66885243249017634, -17.90483003768722625 ) ) ;
#11891 = PLANE ( 'NONE',  #27242 ) ;
#11892 = VECTOR ( 'NONE', #3760, 1000.000000000000000 ) ;
#11893 = CARTESIAN_POINT ( 'NONE',  ( 9.905109554012803130, 16.45925992188944420, -16.51025697316969953 ) ) ;
#11894 = DIRECTION ( 'NONE',  ( -0.9510565162951536422, -2.566386769018988816E-16, -0.3090169943749472292 ) ) ;
#11895 = PLANE ( 'NONE',  #24260 ) ;
#11896 = ORIENTED_EDGE ( 'NONE', *, *, #11830, .F. ) ;
#11897 = DIRECTION ( 'NONE',  ( 1.000000000000000000, 2.698458740408365879E-16, -1.110223024625156540E-16 ) ) ;
#11898 = VERTEX_POINT ( 'NONE', #25354 ) ;
#11899 = EDGE_CURVE ( 'NONE', #28625, #1424, #23761, .T. ) ;
#11900 = CARTESIAN_POINT ( 'NONE',  ( 10.47139596700049147, 16.45505391683073526, -17.33506929010674114 ) ) ;
#11901 = ORIENTED_EDGE ( 'NONE', *, *, #776, .T. ) ;
#11902 = CARTESIAN_POINT ( 'NONE',  ( 32.39840662109286029, -9.588391805189495187, -17.44209920064860597 ) ) ;
#11903 = CARTESIAN_POINT ( 'NONE',  ( 16.30094628073386076, 10.97451324635404291, -15.74372407192620216 ) ) ;
#11904 = CARTESIAN_POINT ( 'NONE',  ( 27.44219139316946965, -6.774709612358828181, -18.29578255718776703 ) ) ;
#11905 = ORIENTED_EDGE ( 'NONE', *, *, #15553, .F. ) ;
#11906 = DIRECTION ( 'NONE',  ( -0.9510565162951536422, 0.000000000000000000, -0.3090169943749472292 ) ) ;
#11907 = LINE ( 'NONE', #12063, #5472 ) ;
#11908 = CARTESIAN_POINT ( 'NONE',  ( 15.13914318552241056, 5.040073780016904870, -15.86576734333453764 ) ) ;
#11909 = CARTESIAN_POINT ( 'NONE',  ( 25.65469514739125856, -9.762610920096198797, -17.09127189072687614 ) ) ;
#11910 = ORIENTED_EDGE ( 'NONE', *, *, #10141, .T. ) ;
#11911 = DIRECTION ( 'NONE',  ( -2.698458740408366372E-16, 1.000000000000000000, 0.000000000000000000 ) ) ;
#11912 = VECTOR ( 'NONE', #11955, 1000.000000000000000 ) ;
#11913 = EDGE_LOOP ( 'NONE', ( #1234, #15250, #7742, #17267, #2622 ) ) ;
#11914 = EDGE_CURVE ( 'NONE', #11708, #8986, #27233, .T. ) ;
#11915 = FACE_OUTER_BOUND ( 'NONE', #14099, .T. ) ;
#11916 = CARTESIAN_POINT ( 'NONE',  ( 173.6922820468852819, -9.999999999999996447, -9.266330736598359152 ) ) ;
#11917 = PRODUCT_DEFINITION ( 'UNKNOWN', '', #21444, #24752 ) ;
#11918 = DIRECTION ( 'NONE',  ( -2.698458740408365879E-16, 1.000000000000000000, 0.000000000000000000 ) ) ;
#11919 = UNCERTAINTY_MEASURE_WITH_UNIT (LENGTH_MEASURE( 1.000000000000000082E-05 ), #25221, 'distance_accuracy_value', 'NONE');
#11920 = CARTESIAN_POINT ( 'NONE',  ( 10.65690970294255280, 16.92416526288626955, -16.00322527524160066 ) ) ;
#11921 = DIRECTION ( 'NONE',  ( 1.000000000000000000, 2.698458740408365879E-16, -1.110223024625156540E-16 ) ) ;
#11922 = CARTESIAN_POINT ( 'NONE',  ( 137.0152310637605808, -10.00000000000000533, -26.04193191628310800 ) ) ;
#11923 = ORIENTED_EDGE ( 'NONE', *, *, #6710, .F. ) ;
#11924 = CARTESIAN_POINT ( 'NONE',  ( 11.47293561586387867, 9.269010148984008879, -15.86088772249501666 ) ) ;
#11925 = CARTESIAN_POINT ( 'NONE',  ( 9.666872068725954392, 16.23194641104447911, -17.88584179299332533 ) ) ;
#11926 = CARTESIAN_POINT ( 'NONE',  ( 17.50199379865806293, 2.211901401554522639, -18.92990045904890550 ) ) ;
#11927 = DIRECTION ( 'NONE',  ( 0.000000000000000000, 1.224646799147353207E-16, 1.000000000000000000 ) ) ;
#11928 = LINE ( 'NONE', #658, #13968 ) ;
#11929 = CARTESIAN_POINT ( 'NONE',  ( 28.67486520862709654, -7.888541471525570614, -13.83454100519475105 ) ) ;
#11930 = ORIENTED_EDGE ( 'NONE', *, *, #16100, .T. ) ;
#11931 = CARTESIAN_POINT ( 'NONE',  ( 163.6922820468853956, -9.999999999999998224, -32.39392330124607611 ) ) ;
#11932 = CARTESIAN_POINT ( 'NONE',  ( 11.23925813788225447, 16.84629677772421275, -16.81283633444384407 ) ) ;
#11933 = ORIENTED_EDGE ( 'NONE', *, *, #11692, .T. ) ;
#11934 = CARTESIAN_POINT ( 'NONE',  ( 35.54859390953724585, -21.18451583373416014, -17.78191007148576119 ) ) ;
#11935 = FACE_OUTER_BOUND ( 'NONE', #25106, .T. ) ;
#11936 = EDGE_LOOP ( 'NONE', ( #7749, #21398, #29369, #17713 ) ) ;
#11937 = ORIENTED_EDGE ( 'NONE', *, *, #8038, .T. ) ;
#11938 = AXIS2_PLACEMENT_3D ( 'NONE', #11739, #7619, #21198 ) ;
#11939 = DIRECTION ( 'NONE',  ( 0.9510565162951535312, 2.566386769018988816E-16, -0.3090169943749475623 ) ) ;
#11940 = CARTESIAN_POINT ( 'NONE',  ( 24.62608015258945215, -5.401662417846991637, -13.04198456947205820 ) ) ;
#11941 = ORIENTED_EDGE ( 'NONE', *, *, #7572, .T. ) ;
#11942 = CARTESIAN_POINT ( 'NONE',  ( 0.000000000000000000, 0.000000000000000000, 0.000000000000000000 ) ) ;
#11943 = CARTESIAN_POINT ( 'NONE',  ( 19.36978511310259421, 2.022953856625822944, -19.43459320487130171 ) ) ;
#11944 = CARTESIAN_POINT ( 'NONE',  ( 18.67591552545227174, 7.243412299697878254, -16.30691131850022657 ) ) ;
#11945 = ORIENTED_EDGE ( 'NONE', *, *, #29078, .T. ) ;
#11946 = ORIENTED_EDGE ( 'NONE', *, *, #12929, .F. ) ;
#11947 = DIRECTION ( 'NONE',  ( 0.9510565162951536422, 2.566386769018988816E-16, 0.3090169943749472292 ) ) ;
#11948 = FACE_OUTER_BOUND ( 'NONE', #3580, .T. ) ;
#11949 = EDGE_CURVE ( 'NONE', #600, #26457, #13295, .T. ) ;
#11950 = EDGE_CURVE ( 'NONE', #25602, #29938, #4447, .T. ) ;
#11951 = CARTESIAN_POINT ( 'NONE',  ( 154.7287565553229172, -4.999999999999975131, 0.8205080756888000204 ) ) ;
#11952 = DIRECTION ( 'NONE',  ( 0.7071067811865474617, 1.962615573354718650E-17, -0.7071067811865475727 ) ) ;
#11953 = VECTOR ( 'NONE', #24532, 1000.000000000000000 ) ;
#11954 = EDGE_CURVE ( 'NONE', #12367, #29073, #9111, .T. ) ;
#11955 = DIRECTION ( 'NONE',  ( -0.5877852522924731371, -1.586114251531760728E-16, -0.8090169943749474513 ) ) ;
#11956 = VERTEX_POINT ( 'NONE', #13742 ) ;
#11957 = VECTOR ( 'NONE', #27453, 1000.000000000000000 ) ;
#11958 = EDGE_CURVE ( 'NONE', #24955, #6624, #2832, .T. ) ;
#11959 = CARTESIAN_POINT ( 'NONE',  ( 9.776119957569173735, 17.05082265352876547, -16.72288386497739765 ) ) ;
#11960 = CARTESIAN_POINT ( 'NONE',  ( 23.87837110222071502, -4.315358902625421322, -12.52832693522684693 ) ) ;
#11961 = CARTESIAN_POINT ( 'NONE',  ( 24.68325608809179528, -0.07379305852225118145, -17.41420097001153167 ) ) ;
#11963 = VERTEX_POINT ( 'NONE', #8706 ) ;
#11962 = CARTESIAN_POINT ( 'NONE',  ( 36.54742519285235858, -23.17926540875556896, -18.54852884019370762 ) ) ;
#11964 = CARTESIAN_POINT ( 'NONE',  ( 0.000000000000000000, 0.000000000000000000, -0.5776712190230064436 ) ) ;
#11965 = CARTESIAN_POINT ( 'NONE',  ( 146.1922820468854241, -10.00000000000000355, -13.59645775552055902 ) ) ;
#11966 = CARTESIAN_POINT ( 'NONE',  ( 162.2287565553229456, -1.999999999999972244, -20.83012701892220520 ) ) ;
#11967 = CARTESIAN_POINT ( 'NONE',  ( 15.19603151210977821, 9.502094893032342782, -14.87270315361914896 ) ) ;
#11968 = VERTEX_POINT ( 'NONE', #17716 ) ;
#11969 = FACE_BOUND ( 'NONE', #16123, .T. ) ;
#11970 = CARTESIAN_POINT ( 'NONE',  ( 10.71880336532874445, 16.64031303757595026, -15.95504377300109944 ) ) ;
#11971 = VECTOR ( 'NONE', #6962, 1000.000000000000000 ) ;
#11972 = ORIENTED_EDGE ( 'NONE', *, *, #6479, .F. ) ;
#11973 = CARTESIAN_POINT ( 'NONE',  ( 159.5152310637605240, -9.999999999999998224, -30.37205893520531319 ) ) ;
#11974 = CARTESIAN_POINT ( 'NONE',  ( -4.000000000000010658, -2.309401076758525573, -2.092734410091829034 ) ) ;
#11975 = VECTOR ( 'NONE', #14446, 1000.000000000000000 ) ;
#11976 = CARTESIAN_POINT ( 'NONE',  ( 21.58242789233717573, 5.264303332692052528, -18.32037006577847293 ) ) ;
#11977 = VERTEX_POINT ( 'NONE', #15875 ) ;
#11978 = CARTESIAN_POINT ( 'NONE',  ( 32.00807787192805876, -10.01600718589171990, -13.21854031764240389 ) ) ;
#11979 = ORIENTED_EDGE ( 'NONE', *, *, #18265, .T. ) ;
#11980 = CARTESIAN_POINT ( 'NONE',  ( 33.35202879388211983, -12.33251541790028760, -19.68467382345759376 ) ) ;
#11981 = CARTESIAN_POINT ( 'NONE',  ( 20.36893440901172170, -1.919154233093003814, -17.42624063329192552 ) ) ;
#11982 = VECTOR ( 'NONE', #2688, 1000.000000000000000 ) ;
#11983 = CARTESIAN_POINT ( 'NONE',  ( 17.24163842130223046, 3.474294283696999219, -15.80253352452890425 ) ) ;
#11984 = AXIS2_PLACEMENT_3D ( 'NONE', #27266, #22183, #1293 ) ;
#11985 = CARTESIAN_POINT ( 'NONE',  ( 29.20193236150002392, -6.731655735042891386, -17.98962132073140552 ) ) ;
#11986 = AXIS2_PLACEMENT_3D ( 'NONE', #25870, #14242, #14389 ) ;
#11987 = VERTEX_POINT ( 'NONE', #4297 ) ;
#11988 = CARTESIAN_POINT ( 'NONE',  ( 2.500000000000000444, 2.357898499370430834, -3.469446951953614189E-15 ) ) ;
#11989 = ADVANCED_FACE ( 'NONE', ( #27074 ), #6132, .T. ) ;
#11991 = ORIENTED_EDGE ( 'NONE', *, *, #29045, .F. ) ;
#11990 = CARTESIAN_POINT ( 'NONE',  ( 166.1922820468853104, -1.999999999999972244, -2.083034168790677043 ) ) ;
#11992 = EDGE_CURVE ( 'NONE', #28209, #28125, #9610, .T. ) ;
#11993 = FACE_OUTER_BOUND ( 'NONE', #19039, .T. ) ;
#11994 = CIRCLE ( 'NONE', #8576, 4.756499999999999062 ) ;
#11995 = EDGE_CURVE ( 'NONE', #24401, #16811, #14032, .T. ) ;
#11996 = CARTESIAN_POINT ( 'NONE',  ( -4.000000000000003553, 0.3904826640788011671, -2.449999999999998401 ) ) ;
#11997 = CARTESIAN_POINT ( 'NONE',  ( 34.93112910557051976, -13.91810326443952306, -19.05872143998290014 ) ) ;
#11998 = VECTOR ( 'NONE', #14969, 1000.000000000000000 ) ;
#11999 = CARTESIAN_POINT ( 'NONE',  ( 9.641350810849047548, 17.66889113945805789, -17.92279151347709032 ) ) ;
#12000 = VERTEX_POINT ( 'NONE', #16787 ) ;
#12001 = APPLICATION_CONTEXT ( 'automotive_design' ) ;
#12002 = AXIS2_PLACEMENT_3D ( 'NONE', #8733, #30016, #29570 ) ;
#12003 = CARTESIAN_POINT ( 'NONE',  ( 167.0152310637604671, -9.999999999999996447, -17.38167787843871182 ) ) ;
#12004 = DIRECTION ( 'NONE',  ( -0.9510565162951536422, -2.566386769018988816E-16, -0.3090169943749472292 ) ) ;
#12005 = CARTESIAN_POINT ( 'NONE',  ( 13.09018272752966716, 8.557097568986355540, -15.93847522207377310 ) ) ;
#12006 = LINE ( 'NONE', #21319, #21948 ) ;
#12007 = LINE ( 'NONE', #23473, #25203 ) ;
#12008 = ORIENTED_EDGE ( 'NONE', *, *, #231, .F. ) ;
#12009 = PLANE ( 'NONE',  #21720 ) ;
#12010 = VERTEX_POINT ( 'NONE', #25648 ) ;
#12011 = LINE ( 'NONE', #23946, #27369 ) ;
#12012 = ORIENTED_EDGE ( 'NONE', *, *, #28646, .F. ) ;
#12013 = CARTESIAN_POINT ( 'NONE',  ( 13.00000000000001243, 55.00000000000000711, -18.00000000000000000 ) ) ;
#12014 = EDGE_LOOP ( 'NONE', ( #15233, #11043, #9860, #16172 ) ) ;
#12015 = CARTESIAN_POINT ( 'NONE',  ( 9.700291501659986437, 16.07868063162199945, -17.87166786738998780 ) ) ;
#12016 = CARTESIAN_POINT ( 'NONE',  ( 27.00779440489029071, -4.779404007149373079, -14.88408750732950914 ) ) ;
#12017 = CARTESIAN_POINT ( 'NONE',  ( 20.59283418570449697, -4.290598171560842111, -16.90930062131523215 ) ) ;
#12018 = VECTOR ( 'NONE', #5891, 1000.000000000000000 ) ;
#12019 = CARTESIAN_POINT ( 'NONE',  ( 141.1922820468854241, -4.999999999999979572, -4.936203717676158398 ) ) ;
#12020 = PLANE ( 'NONE',  #22350 ) ;
#12021 = LINE ( 'NONE', #9731, #28448 ) ;
#12022 = VECTOR ( 'NONE', #27389, 1000.000000000000000 ) ;
#12023 = CARTESIAN_POINT ( 'NONE',  ( 25.04068920418659161, -5.475481712173364990, -18.92835678451453774 ) ) ;
#12024 = AXIS2_PLACEMENT_3D ( 'NONE', #2877, #19485, #721 ) ;
#12025 = ORIENTED_EDGE ( 'NONE', *, *, #12331, .F. ) ;
#12026 = LINE ( 'NONE', #29973, #15901 ) ;
#12027 = CARTESIAN_POINT ( 'NONE',  ( -1.310841663519413114, 0.000000000000000000, 0.000000000000000000 ) ) ;
#12028 = VECTOR ( 'NONE', #29870, 1000.000000000000000 ) ;
#12029 = CARTESIAN_POINT ( 'NONE',  ( 2.500000000000000444, 2.357898499370430834, -3.469446951953614189E-15 ) ) ;
#12030 = ADVANCED_FACE ( 'NONE', ( #9148 ), #16483, .T. ) ;
#12031 = EDGE_CURVE ( 'NONE', #3628, #9641, #20, .T. ) ;
#12032 = FACE_OUTER_BOUND ( 'NONE', #17908, .T. ) ;
#12033 = CARTESIAN_POINT ( 'NONE',  ( 107.3608926408196140, -4.999999999999988454, 78.00225434817323844 ) ) ;
#12034 = ADVANCED_FACE ( 'NONE', ( #472 ), #326, .T. ) ;
#12035 = EDGE_CURVE ( 'NONE', #5806, #12653, #18632, .T. ) ;
#12036 = CARTESIAN_POINT ( 'NONE',  ( 11.50940939395034768, 11.69459202490242689, -16.90580767540677343 ) ) ;
#12037 = CARTESIAN_POINT ( 'NONE',  ( 8.000000000000001776, 4.336808689942017736E-15, 0.000000000000000000 ) ) ;
#12038 = CARTESIAN_POINT ( 'NONE',  ( 33.37634376253905089, -12.42895282922877342, -19.69946502924221932 ) ) ;
#12039 = ORIENTED_EDGE ( 'NONE', *, *, #16797, .T. ) ;
#12040 = CARTESIAN_POINT ( 'NONE',  ( 13.43370121458407418, 7.649856678006609734, -15.66476257323406784 ) ) ;
#12041 = VERTEX_POINT ( 'NONE', #9760 ) ;
#12042 = DIRECTION ( 'NONE',  ( -0.000000000000000000, -0.000000000000000000, -1.000000000000000000 ) ) ;
#12043 = VECTOR ( 'NONE', #3546, 1000.000000000000000 ) ;
#12044 = CARTESIAN_POINT ( 'NONE',  ( 19.71807001554888217, -1.708786246101231532, -19.21472004699903380 ) ) ;
#12045 = CARTESIAN_POINT ( 'NONE',  ( 12.83198842527593087, 9.541832653742346793, -16.14114841745374562 ) ) ;
#12046 = CARTESIAN_POINT ( 'NONE',  ( 171.1922820468853104, -4.999999999999971578, -10.74328820663507678 ) ) ;
#12047 = ORIENTED_EDGE ( 'NONE', *, *, #25373, .F. ) ;
#12048 = VECTOR ( 'NONE', #3895, 1000.000000000000000 ) ;
#12049 = CARTESIAN_POINT ( 'NONE',  ( 9.913797604922770290, 16.41941541294738727, -16.50570979788118464 ) ) ;
#12050 = FACE_BOUND ( 'NONE', #5691, .T. ) ;
#12051 = CARTESIAN_POINT ( 'NONE',  ( 9.916551108984865692, 16.40678749232849398, -16.50450761325770443 ) ) ;
#12052 = CARTESIAN_POINT ( 'NONE',  ( 163.6922820468853956, -1.999999999999971356, -32.39392330124607611 ) ) ;
#12053 = ORIENTED_EDGE ( 'NONE', *, *, #3821, .T. ) ;
#12054 = CARTESIAN_POINT ( 'NONE',  ( 8.000000000000003553, 4.618802153517037823, -4.285468820183664818 ) ) ;
#12055 = ORIENTED_EDGE ( 'NONE', *, *, #18862, .F. ) ;
#12056 = CARTESIAN_POINT ( 'NONE',  ( 10.35870477237433818, 16.97187010017241349, -17.89775757279876700 ) ) ;
#12057 = CIRCLE ( 'NONE', #27701, 2.041999999999999815 ) ;
#12058 = CARTESIAN_POINT ( 'NONE',  ( 33.01522398464379648, -9.800858501837518943, -19.11635465682842394 ) ) ;
#12059 = CARTESIAN_POINT ( 'NONE',  ( 29.76939623719675510, -8.219725197086590995, -17.35520659559267287 ) ) ;
#12060 = CARTESIAN_POINT ( 'NONE',  ( 15.44177808481316383, 7.494736869644298416, -14.00399691429678306 ) ) ;
#12061 = CARTESIAN_POINT ( 'NONE',  ( 152.2287565553230024, -10.00000000000000178, -20.83012701892220520 ) ) ;
#12062 = ORIENTED_EDGE ( 'NONE', *, *, #8284, .F. ) ;
#12063 = CARTESIAN_POINT ( 'NONE',  ( 108.2718491523516207, -4.999999999999987566, -78.66410299496463665 ) ) ;
#12064 = DIRECTION ( 'NONE',  ( 1.000000000000000000, 0.000000000000000000, 0.000000000000000000 ) ) ;
#12065 = CARTESIAN_POINT ( 'NONE',  ( 27.03191753302054323, -12.88672130028117735, -14.08881772908025454 ) ) ;
#12066 = CARTESIAN_POINT ( 'NONE',  ( 28.63694740700460173, -9.765300015774602826, -17.75617681614052046 ) ) ;
#12067 = VECTOR ( 'NONE', #22582, 1000.000000000000000 ) ;
#12068 = ORIENTED_EDGE ( 'NONE', *, *, #23765, .F. ) ;
#12069 = FACE_BOUND ( 'NONE', #29356, .T. ) ;
#12070 = CIRCLE ( 'NONE', #15490, 0.8500000000000000888 ) ;
#12071 = EDGE_CURVE ( 'NONE', #20011, #18400, #4740, .T. ) ;
#12072 = EDGE_CURVE ( 'NONE', #12263, #23543, #21211, .T. ) ;
#12073 = ORIENTED_EDGE ( 'NONE', *, *, #10557, .T. ) ;
#12074 = EDGE_CURVE ( 'NONE', #19491, #19224, #2920, .T. ) ;
#12075 = CARTESIAN_POINT ( 'NONE',  ( 169.7287565553229740, -9.999999999999996447, -33.82050807568879947 ) ) ;
#12076 = CARTESIAN_POINT ( 'NONE',  ( 36.04859390953723874, -22.18451583373416014, -15.00000000000000000 ) ) ;
#12077 = FACE_OUTER_BOUND ( 'NONE', #19187, .T. ) ;
#12078 = CARTESIAN_POINT ( 'NONE',  ( 153.6922820468853672, -1.999999999999975353, -6.413161187712876909 ) ) ;
#12079 = CARTESIAN_POINT ( 'NONE',  ( 10.72107673987424015, 16.62988705212242735, -15.95408154060974404 ) ) ;
#12080 = LINE ( 'NONE', #20784, #11204 ) ;
#12081 = DIRECTION ( 'NONE',  ( 0.000000000000000000, 0.000000000000000000, 1.000000000000000000 ) ) ;
#12082 = ORIENTED_EDGE ( 'NONE', *, *, #1936, .T. ) ;
#12083 = CARTESIAN_POINT ( 'NONE',  ( 10.17605321708455257, 15.21667774575863419, -16.39719424528293246 ) ) ;
#12084 = ORIENTED_EDGE ( 'NONE', *, *, #13312, .F. ) ;
#12085 = VECTOR ( 'NONE', #11747, 1000.000000000000000 ) ;
#12086 = CARTESIAN_POINT ( 'NONE',  ( 21.72387110042699376, 1.401658020055618792, -20.45241765577301152 ) ) ;
#12087 = CARTESIAN_POINT ( 'NONE',  ( 158.6922820468853956, -9.999999999999998224, -26.58683881228715862 ) ) ;
#12088 = DIRECTION ( 'NONE',  ( 0.000000000000000000, -2.775557561562890735E-17, 1.000000000000000000 ) ) ;
#12089 = ORIENTED_EDGE ( 'NONE', *, *, #12547, .F. ) ;
#12090 = CARTESIAN_POINT ( 'NONE',  ( 30.24922550192677306, -10.40856591028444278, -13.02298783260255988 ) ) ;
#12091 = ORIENTED_EDGE ( 'NONE', *, *, #9890, .F. ) ;
#12092 = CARTESIAN_POINT ( 'NONE',  ( 174.5152310637604387, -9.999999999999994671, -11.28819510263909542 ) ) ;
#12093 = CARTESIAN_POINT ( 'NONE',  ( 11.27588265011317326, 16.67833209609329259, -16.78465339804365541 ) ) ;
#12094 = VERTEX_POINT ( 'NONE', #7340 ) ;
#12095 = VECTOR ( 'NONE', #12778, 1000.000000000000000 ) ;
#12096 = CARTESIAN_POINT ( 'NONE',  ( 34.98004922032874475, -18.63034571161586683, -19.14376959241974774 ) ) ;
#12097 = CARTESIAN_POINT ( 'NONE',  ( 14.24706144987486667, 6.238427219560604087, -16.72753349211556184 ) ) ;
#12098 = CARTESIAN_POINT ( 'NONE',  ( 92.33196323856196841, -4.999999999999992006, -67.08309798704286209 ) ) ;
#12099 = CARTESIAN_POINT ( 'NONE',  ( 8.977559110355956662, 16.80036783546273327, -17.41076197725142194 ) ) ;
#12100 = CARTESIAN_POINT ( 'NONE',  ( 22.80194228990702143, -6.214338098008789224, -14.16187805771452801 ) ) ;
#12101 = ORIENTED_EDGE ( 'NONE', *, *, #19067, .F. ) ;
#12102 = VECTOR ( 'NONE', #10334, 1000.000000000000000 ) ;
#12103 = FACE_OUTER_BOUND ( 'NONE', #18746, .T. ) ;
#12104 = ADVANCED_FACE ( 'NONE', ( #7040 ), #11895, .T. ) ;
#12105 = SURFACE_SIDE_STYLE ('',( #7530 ) ) ;
#12106 = CARTESIAN_POINT ( 'NONE',  ( 21.65198393244800812, 4.573788442230395823, -17.29480057625502454 ) ) ;
#12107 = CARTESIAN_POINT ( 'NONE',  ( 17.00905032053054811, 4.985101812230166907, -18.82491780458422781 ) ) ;
#12108 = CARTESIAN_POINT ( 'NONE',  ( 134.7287565553230024, -10.00000000000000711, -33.82050807568879947 ) ) ;
#12109 = VERTEX_POINT ( 'NONE', #16331 ) ;
#12110 = LINE ( 'NONE', #12405, #6840 ) ;
#12111 = EDGE_CURVE ( 'NONE', #24640, #26897, #11595, .T. ) ;
#12112 = DIRECTION ( 'NONE',  ( -2.698458740408365879E-16, 1.000000000000000000, 0.000000000000000000 ) ) ;
#12113 = DIRECTION ( 'NONE',  ( -1.000000000000000000, -4.440892098500622217E-16, 0.000000000000000000 ) ) ;
#12114 = VECTOR ( 'NONE', #12471, 1000.000000000000000 ) ;
#12115 = CARTESIAN_POINT ( 'NONE',  ( 3.150000000000000799, 1.398881011027696413E-15, 2.550000000000000266 ) ) ;
#12116 = CARTESIAN_POINT ( 'NONE',  ( 2.500000000000000444, 2.357898499370430834, -3.469446951953614189E-15 ) ) ;
#12117 = EDGE_LOOP ( 'NONE', ( #2728, #14679, #9872, #12082 ) ) ;
#12118 = CARTESIAN_POINT ( 'NONE',  ( 9.641350829061996919, 17.66889105593114806, -17.91548090047172437 ) ) ;
#12119 = VECTOR ( 'NONE', #8046, 1000.000000000000000 ) ;
#12120 = CARTESIAN_POINT ( 'NONE',  ( 26.19520757255249066, -7.109971961106261951, -13.37903969216112898 ) ) ;
#12121 = CARTESIAN_POINT ( 'NONE',  ( 21.56383972367567736, -3.323709001909281202, -18.92284382192250192 ) ) ;
#12123 = ORIENTED_EDGE ( 'NONE', *, *, #11117, .T. ) ;
#12122 = CARTESIAN_POINT ( 'NONE',  ( 34.79556486487921774, -19.80155522666461465, -21.17264749384332134 ) ) ;
#12124 = VECTOR ( 'NONE', #2392, 1000.000000000000000 ) ;
#12125 = CARTESIAN_POINT ( 'NONE',  ( 142.0152310637605808, -4.999999999999979572, -17.38167787843871182 ) ) ;
#12126 = CARTESIAN_POINT ( 'NONE',  ( 14.38576730248667701, 9.404056492746565965, -13.62718518646353161 ) ) ;
#12127 = CARTESIAN_POINT ( 'NONE',  ( 173.6922820468853672, -1.999999999999970024, -32.39392330124607611 ) ) ;
#12128 = LINE ( 'NONE', #21136, #16351 ) ;
#12129 = CARTESIAN_POINT ( 'NONE',  ( 15.93484470893836935, 6.939319753835953009, -14.67888072223970752 ) ) ;
#12130 = VERTEX_POINT ( 'NONE', #173 ) ;
#12131 = DIRECTION ( 'NONE',  ( -2.698458740408365879E-16, 1.000000000000000000, 0.000000000000000000 ) ) ;
#12132 = CARTESIAN_POINT ( 'NONE',  ( 10.70792791965113544, 16.69018921775036546, -15.96040338026158523 ) ) ;
#12133 = DIRECTION ( 'NONE',  ( 0.5877852522924731371, 0.000000000000000000, 0.8090169943749474513 ) ) ;
#12134 = CARTESIAN_POINT ( 'NONE',  ( 90.57535369523569102, -4.999999999999992895, 65.80684644871624300 ) ) ;
#12135 = ORIENTED_EDGE ( 'NONE', *, *, #13650, .T. ) ;
#12136 = CARTESIAN_POINT ( 'NONE',  ( 14.39533340154967433, 6.572929804808670617, -18.54476805420031837 ) ) ;
#12137 = CARTESIAN_POINT ( 'NONE',  ( 26.67611703245768950, -12.21101477627283849, -12.48819288018415108 ) ) ;
#12138 = VERTEX_POINT ( 'NONE', #16639 ) ;
#12139 = CARTESIAN_POINT ( 'NONE',  ( 32.74314609665832165, -11.10724048739539782, -18.62249297335446840 ) ) ;
#12140 = EDGE_CURVE ( 'NONE', #26865, #4487, #17272, .T. ) ;
#12141 = AXIS2_PLACEMENT_3D ( 'NONE', #13613, #22943, #16049 ) ;
#12142 = CARTESIAN_POINT ( 'NONE',  ( 22.92155253933561809, -3.178009374129639131, -14.34666800710537693 ) ) ;
#12143 = ORIENTED_EDGE ( 'NONE', *, *, #25072, .F. ) ;
#12144 = EDGE_CURVE ( 'NONE', #4293, #11898, #14184, .T. ) ;
#12145 = CARTESIAN_POINT ( 'NONE',  ( 22.41093758190154972, 3.143874582428516806, -16.84310506638757943 ) ) ;
#12146 = VECTOR ( 'NONE', #24779, 1000.000000000000000 ) ;
#12147 = CARTESIAN_POINT ( 'NONE',  ( 25.09247252535503492, -10.89683230441130135, -15.98339435310939827 ) ) ;
#12148 = VERTEX_POINT ( 'NONE', #5190 ) ;
#12149 = DIRECTION ( 'NONE',  ( -1.000000000000000000, -0.000000000000000000, 0.000000000000000000 ) ) ;
#12151 = EDGE_LOOP ( 'NONE', ( #25845, #6515 ) ) ;
#12150 = CARTESIAN_POINT ( 'NONE',  ( 6.938893903907228378E-15, 55.00000000000000711, -1.040834085586084257E-14 ) ) ;
#12152 = DIRECTION ( 'NONE',  ( -0.5877852522924731371, 0.000000000000000000, 0.8090169943749474513 ) ) ;
#12153 = DIRECTION ( 'NONE',  ( -0.5877852522924731371, -1.586114251531760235E-16, 0.8090169943749474513 ) ) ;
#12154 = CARTESIAN_POINT ( 'NONE',  ( 34.53678113438137842, -12.15940631226206925, -18.93201839848989465 ) ) ;
#12155 = CIRCLE ( 'NONE', #14110, 5.000000000000000000 ) ;
#12156 = CARTESIAN_POINT ( 'NONE',  ( 9.641364314812712166, 17.66882920855936590, -17.90209449470656722 ) ) ;
#12157 = CARTESIAN_POINT ( 'NONE',  ( 143.6922820468853956, -10.00000000000000533, 2.247092850131519715 ) ) ;
#12158 = LINE ( 'NONE', #19478, #27094 ) ;
#12159 = CARTESIAN_POINT ( 'NONE',  ( 12.72883512080982804, 8.524354266104470668, -16.21679389071614352 ) ) ;
#12160 = DIRECTION ( 'NONE',  ( 2.908569913943825554E-16, -1.000000000000000000, 0.000000000000000000 ) ) ;
#12161 = VECTOR ( 'NONE', #15368, 1000.000000000000000 ) ;
#12162 = CARTESIAN_POINT ( 'NONE',  ( 10.00000000000008527, 17.32050807568872486, -17.99999999999999645 ) ) ;
#12163 = ORIENTED_EDGE ( 'NONE', *, *, #21933, .F. ) ;
#12164 = LINE ( 'NONE', #3333, #19768 ) ;
#12165 = CYLINDRICAL_SURFACE ( 'NONE', #13173, 5.000000000000000000 ) ;
#12166 = VERTEX_POINT ( 'NONE', #6896 ) ;
#12167 = LINE ( 'NONE', #28972, #12048 ) ;
#12168 = ORIENTED_EDGE ( 'NONE', *, *, #950, .T. ) ;
#12169 = CARTESIAN_POINT ( 'NONE',  ( 11.22637516657937162, 9.079975409179585455, -17.24057027585384105 ) ) ;
#12170 = EDGE_CURVE ( 'NONE', #134, #5625, #2769, .T. ) ;
#12171 = CARTESIAN_POINT ( 'NONE',  ( 24.01829950071418907, -5.359185124211399476, -18.14381017295562160 ) ) ;
#12172 = EDGE_CURVE ( 'NONE', #3548, #17432, #25505, .T. ) ;
#12173 = CARTESIAN_POINT ( 'NONE',  ( 24.68325608809179528, -0.07379305852225118145, -17.41420097001153167 ) ) ;
#12174 = CARTESIAN_POINT ( 'NONE',  ( 2.500000000000000444, -1.178949249685215417, -2.041999999999998483 ) ) ;
#12175 = DIRECTION ( 'NONE',  ( 0.5877852522924731371, 1.586114251531760728E-16, 0.8090169943749474513 ) ) ;
#12176 = ADVANCED_FACE ( 'NONE', ( #29185 ), #3217, .T. ) ;
#12177 = CARTESIAN_POINT ( 'NONE',  ( 25.00000000000000000, 0.000000000000000000, 0.000000000000000000 ) ) ;
#12178 = VECTOR ( 'NONE', #21014, 999.9999999999998863 ) ;
#12179 = CARTESIAN_POINT ( 'NONE',  ( 164.7287565553228887, -9.999999999999998224, 0.8205080756887930260 ) ) ;
#12180 = DIRECTION ( 'NONE',  ( 0.3090169943749472292, 8.338696094057992503E-17, -0.9510565162951536422 ) ) ;
#12181 = DIRECTION ( 'NONE',  ( 1.000000000000000000, 2.698458740408365879E-16, -1.110223024625156540E-16 ) ) ;
#12182 = PLANE ( 'NONE',  #25372 ) ;
#12183 = LINE ( 'NONE', #17516, #13344 ) ;
#12184 = AXIS2_PLACEMENT_3D ( 'NONE', #8253, #6127, #27230 ) ;
#12185 = CARTESIAN_POINT ( 'NONE',  ( 10.55304143273637330, 16.08061740358965253, -17.30129946959702281 ) ) ;
#12186 = CIRCLE ( 'NONE', #3428, 139.8897274573438096 ) ;
#12187 = DIRECTION ( 'NONE',  ( -1.000000000000000000, -2.698458740408366372E-16, 8.163404592832029035E-16 ) ) ;
#12188 = CARTESIAN_POINT ( 'NONE',  ( 49.00000000000000000, -1.252609127533332839E-16, 4.513000000000000789 ) ) ;
#12189 = ORIENTED_EDGE ( 'NONE', *, *, #19817, .T. ) ;
#12190 = VECTOR ( 'NONE', #25239, 1000.000000000000000 ) ;
#12191 = CARTESIAN_POINT ( 'NONE',  ( 13.37957753592864663, 7.625938299336016968, -15.70790011242621453 ) ) ;
#12192 = CARTESIAN_POINT ( 'NONE',  ( 0.2500000000000002220, 0.000000000000000000, 0.000000000000000000 ) ) ;
#12193 = CARTESIAN_POINT ( 'NONE',  ( 20.14386580841007657, 1.771853782379294140, -13.30505882909219295 ) ) ;
#12194 = CARTESIAN_POINT ( 'NONE',  ( 12.57288446902313872, 10.73011642529405307, -16.24829701787703939 ) ) ;
#12195 = FACE_BOUND ( 'NONE', #50, .T. ) ;
#12196 = EDGE_LOOP ( 'NONE', ( #24533, #466, #24539, #16450 ) ) ;
#12197 = AXIS2_PLACEMENT_3D ( 'NONE', #19505, #10193, #3500 ) ;
#12198 = VERTEX_POINT ( 'NONE', #7779 ) ;
#12199 = CARTESIAN_POINT ( 'NONE',  ( 10.82443827553465177, 12.24310121783546634, -16.12906421532448675 ) ) ;
#12200 = DIRECTION ( 'NONE',  ( -0.5877852522924731371, -1.586114251531760235E-16, 0.8090169943749474513 ) ) ;
#12201 = CARTESIAN_POINT ( 'NONE',  ( 11.43229926783177497, 9.455373222906182207, -15.87769231223556332 ) ) ;
#12202 = DIRECTION ( 'NONE',  ( -0.9510565162951536422, 0.000000000000000000, -0.3090169943749472292 ) ) ;
#12203 = ORIENTED_EDGE ( 'NONE', *, *, #8452, .F. ) ;
#12204 = DIRECTION ( 'NONE',  ( -0.5877852522924731371, -1.586114251531760235E-16, 0.8090169943749474513 ) ) ;
#12205 = EDGE_LOOP ( 'NONE', ( #22510, #12537, #7828, #28589, #7782 ) ) ;
#12206 = CARTESIAN_POINT ( 'NONE',  ( 12.35422140817580683, 8.720385185214494683, -16.48779044034850116 ) ) ;
#12207 = ORIENTED_EDGE ( 'NONE', *, *, #24184, .F. ) ;
#12208 = CARTESIAN_POINT ( 'NONE',  ( 36.44920892064849482, -21.73803172434679354, -19.68085951391205057 ) ) ;
#12209 = CARTESIAN_POINT ( 'NONE',  ( 17.15446488409023829, 10.64262399902749578, -18.76211774343175520 ) ) ;
#12210 = CARTESIAN_POINT ( 'NONE',  ( 25.90632082398269276, -12.28056132945115841, -15.12647891527467969 ) ) ;
#12211 = VERTEX_POINT ( 'NONE', #8070 ) ;
#12212 = EDGE_CURVE ( 'NONE', #1890, #26875, #8222, .T. ) ;
#12213 = CARTESIAN_POINT ( 'NONE',  ( 16.16257886861838955, -5.000000000000013323, -49.74330290224348516 ) ) ;
#12214 = ADVANCED_FACE ( 'NONE', ( #21660 ), #17090, .F. ) ;
#12215 = EDGE_CURVE ( 'NONE', #23323, #29393, #19820, .T. ) ;
#12216 = EDGE_CURVE ( 'NONE', #2560, #4171, #17380, .T. ) ;
#12217 = CARTESIAN_POINT ( 'NONE',  ( 32.20428705557502269, -10.20872362009771095, -14.89176492545819919 ) ) ;
#12218 = CIRCLE ( 'NONE', #8318, 49.99999999999998579 ) ;
#12219 = SHAPE_DEFINITION_REPRESENTATION ( #24973, #22819 ) ;
#12220 = CARTESIAN_POINT ( 'NONE',  ( 21.74214448781610542, 1.960522507982400020, -19.23370281053773923 ) ) ;
#12221 = AXIS2_PLACEMENT_3D ( 'NONE', #22306, #19854, #3545 ) ;
#12222 = CARTESIAN_POINT ( 'NONE',  ( 29.36168402625536444, -8.616725751243539122, -15.73432514746931155 ) ) ;
#12223 = CARTESIAN_POINT ( 'NONE',  ( 146.1922820468854525, -4.999999999999978684, -30.91696583120935671 ) ) ;
#12224 = FACE_BOUND ( 'NONE', #2482, .T. ) ;
#12225 =( GEOMETRIC_REPRESENTATION_CONTEXT ( 3 ) GLOBAL_UNCERTAINTY_ASSIGNED_CONTEXT ( ( #15902 ) ) GLOBAL_UNIT_ASSIGNED_CONTEXT ( ( #4940, #20959, #528 ) ) REPRESENTATION_CONTEXT ( 'NONE', 'WORKASPACE' ) );
#12226 = CARTESIAN_POINT ( 'NONE',  ( 6.938893903907228378E-15, 60.00000000000000711, -12.50000000000001066 ) ) ;
#12227 = CARTESIAN_POINT ( 'NONE',  ( 166.1922820468853388, -1.999999999999971800, -10.74328820663507678 ) ) ;
#12228 = CARTESIAN_POINT ( 'NONE',  ( 129.5152310637605808, -10.00000000000000888, -2.627941064794695691 ) ) ;
#12229 = CARTESIAN_POINT ( 'NONE',  ( 74.18800000000001660, 7.511012776518211958E-16, -5.000000000000000888 ) ) ;
#12230 = CARTESIAN_POINT ( 'NONE',  ( 12.19589625337134997, 9.866176767462979669, -15.34419179356244634 ) ) ;
#12232 = AXIS2_PLACEMENT_3D ( 'NONE', #11965, #4656, #2239 ) ;
#12231 = DIRECTION ( 'NONE',  ( 1.110223024625156540E-16, 2.995891024602366092E-32, 1.000000000000000000 ) ) ;
#12233 = CARTESIAN_POINT ( 'NONE',  ( 152.0152310637606092, -1.999999999999974465, -32.93883019725009120 ) ) ;
#12234 = VERTEX_POINT ( 'NONE', #15079 ) ;
#12235 = VECTOR ( 'NONE', #3740, 1000.000000000000000 ) ;
#12236 = CARTESIAN_POINT ( 'NONE',  ( 12.49742530276927610, 8.569573706352677789, -15.13222638044318735 ) ) ;
#12237 = ORIENTED_EDGE ( 'NONE', *, *, #28491, .T. ) ;
#12238 = CARTESIAN_POINT ( 'NONE',  ( 22.35455276305805938, 2.055732105393538678, -20.05127887597516434 ) ) ;
#12239 = CARTESIAN_POINT ( 'NONE',  ( 120.0000000000000000, 20.00000000000000355, -186.4312945166758482 ) ) ;
#12240 = CARTESIAN_POINT ( 'NONE',  ( 164.5152310637604671, -9.999999999999998224, -2.627941064794695691 ) ) ;
#12241 = DIRECTION ( 'NONE',  ( -0.8090169943749474513, -2.183098979609982436E-16, 0.5877852522924731371 ) ) ;
#12242 = ORIENTED_EDGE ( 'NONE', *, *, #10477, .F. ) ;
#12243 = FACE_OUTER_BOUND ( 'NONE', #12352, .T. ) ;
#12244 = CARTESIAN_POINT ( 'NONE',  ( 11.26867954870061439, 16.71136643735313143, -16.78814161468471156 ) ) ;
#12245 = VERTEX_POINT ( 'NONE', #17530 ) ;
#12246 = CARTESIAN_POINT ( 'NONE',  ( 33.55945865873172096, -12.30028340163019607, -18.68418013052470883 ) ) ;
#12247 = CARTESIAN_POINT ( 'NONE',  ( 17.32695330507268494, 5.471673316493076200, -20.08600194542987794 ) ) ;
#12248 = ADVANCED_FACE ( 'NONE', ( #12495 ), #760, .T. ) ;
#12249 = DIRECTION ( 'NONE',  ( -0.8090169943749474513, -2.183098979609982436E-16, -0.5877852522924731371 ) ) ;
#12250 = CARTESIAN_POINT ( 'NONE',  ( 26.73315660230872837, -4.509142541826837380, -13.49646658189591619 ) ) ;
#12251 = VERTEX_POINT ( 'NONE', #14932 ) ;
#12252 = EDGE_CURVE ( 'NONE', #10971, #3997, #24120, .T. ) ;
#12253 = LINE ( 'NONE', #28483, #18844 ) ;
#12254 = SURFACE_STYLE_FILL_AREA ( #2977 ) ;
#12255 = CARTESIAN_POINT ( 'NONE',  ( 25.47985489653468605, -2.350970512090694520, -13.88367939857760014 ) ) ;
#12256 = CARTESIAN_POINT ( 'NONE',  ( 15.10317701704014226, 5.923596928851710075, -17.67988701311836053 ) ) ;
#12257 = ORIENTED_EDGE ( 'NONE', *, *, #4534, .T. ) ;
#12258 = CARTESIAN_POINT ( 'NONE',  ( 130.7287565553229172, -4.999999999999983125, -28.21440484423857242 ) ) ;
#12259 = ORIENTED_EDGE ( 'NONE', *, *, #10581, .F. ) ;
#12260 = DIRECTION ( 'NONE',  ( 0.5877852522924731371, 0.000000000000000000, 0.8090169943749474513 ) ) ;
#12261 = VECTOR ( 'NONE', #1296, 1000.000000000000000 ) ;
#12262 = PLANE ( 'NONE',  #6992 ) ;
#12263 = VERTEX_POINT ( 'NONE', #24268 ) ;
#12264 = CARTESIAN_POINT ( 'NONE',  ( 144.5152310637605240, -4.999999999999978684, -1.604441369360115876E-14 ) ) ;
#12265 = DIRECTION ( 'NONE',  ( -1.000000000000000000, 0.000000000000000000, 0.000000000000000000 ) ) ;
#12266 = FACE_OUTER_BOUND ( 'NONE', #17765, .T. ) ;
#12267 = CARTESIAN_POINT ( 'NONE',  ( 11.46471852075427478, 9.306694396509932687, -15.86428581073749378 ) ) ;
#12268 = CARTESIAN_POINT ( 'NONE',  ( 27.49606495187617128, -9.167791027049197794, -14.03786016821673677 ) ) ;
#12269 = CARTESIAN_POINT ( 'NONE',  ( 21.55249387529322647, -4.041031698679099726, -14.19001464829599435 ) ) ;
#12270 = EDGE_CURVE ( 'NONE', #24297, #25495, #918, .T. ) ;
#12272 = ORIENTED_EDGE ( 'NONE', *, *, #15257, .F. ) ;
#12271 = CARTESIAN_POINT ( 'NONE',  ( 32.67186286342521839, -11.06527230177895227, -18.43913201350460440 ) ) ;
#12273 = DIRECTION ( 'NONE',  ( -1.000000000000000000, 0.000000000000000000, 0.000000000000000000 ) ) ;
#12274 = CARTESIAN_POINT ( 'NONE',  ( -1.660531772554310725, 3.660093687634845772, 4.223306275009939913E-15 ) ) ;
#12275 = DIRECTION ( 'NONE',  ( -1.734723475976807587E-16, 0.000000000000000000, -1.000000000000000000 ) ) ;
#12276 = AXIS2_PLACEMENT_3D ( 'NONE', #21982, #14943, #7795 ) ;
#12277 = PLANE ( 'NONE',  #17552 ) ;
#12278 = CARTESIAN_POINT ( 'NONE',  ( 3.344563996438202569, 2.687817229851458212, -2.291324518471520300 ) ) ;
#12279 = CARTESIAN_POINT ( 'NONE',  ( 21.19279910686179846, 4.720633506281588510, -19.26595127233560234 ) ) ;
#12280 = ORIENTED_EDGE ( 'NONE', *, *, #30125, .T. ) ;
#12281 = DIRECTION ( 'NONE',  ( -2.698458740408365879E-16, 1.000000000000000000, 0.000000000000000000 ) ) ;
#12282 = CARTESIAN_POINT ( 'NONE',  ( 10.71275814632708823, 16.66803718250374899, -15.95787532639072914 ) ) ;
#12283 = CARTESIAN_POINT ( 'NONE',  ( 142.0152310637605808, -10.00000000000000355, -34.70218595412750773 ) ) ;
#12284 = CARTESIAN_POINT ( 'NONE',  ( 0.000000000000000000, 0.000000000000000000, 0.000000000000000000 ) ) ;
#12285 = CARTESIAN_POINT ( 'NONE',  ( 21.79935899731381710, -1.430375723040585356, -13.25318265510616733 ) ) ;
#12286 = CARTESIAN_POINT ( 'NONE',  ( 25.97279949409942290, -11.71600155862194015, -18.85018042282848683 ) ) ;
#12287 = EDGE_LOOP ( 'NONE', ( #24966, #25393, #2583, #24815, #23035, #16542 ) ) ;
#12288 = CARTESIAN_POINT ( 'NONE',  ( 32.36240160181304759, -11.00785621467150044, -17.57054915585148436 ) ) ;
#12289 = CARTESIAN_POINT ( 'NONE',  ( 22.60637541839240683, -1.101515789306901194, -14.68923631892221948 ) ) ;
#12290 = VECTOR ( 'NONE', #18335, 1000.000000000000000 ) ;
#12291 = CARTESIAN_POINT ( 'NONE',  ( 19.31105547890425100, 3.022890346832332042, -18.89353813576326857 ) ) ;
#12292 = VERTEX_POINT ( 'NONE', #12347 ) ;
#12293 = CARTESIAN_POINT ( 'NONE',  ( 27.51083730600015897, -9.905735641176994122, -13.30399992039142099 ) ) ;
#12294 = ORIENTED_EDGE ( 'NONE', *, *, #27363, .F. ) ;
#12295 = AXIS2_PLACEMENT_3D ( 'NONE', #8048, #24095, #3197 ) ;
#12296 = ORIENTED_EDGE ( 'NONE', *, *, #24912, .T. ) ;
#12297 = CARTESIAN_POINT ( 'NONE',  ( 172.7287565553229456, -1.999999999999970468, -33.50000000000000000 ) ) ;
#12298 = LINE ( 'NONE', #1781, #11892 ) ;
#12299 = DIRECTION ( 'NONE',  ( 0.3090169943749475623, 8.338696094058001131E-17, 0.9510565162951536422 ) ) ;
#12300 = EDGE_CURVE ( 'NONE', #18617, #18267, #10507, .T. ) ;
#12301 = CARTESIAN_POINT ( 'NONE',  ( 34.38415957124060895, -12.46085888452578594, -19.93570721963346060 ) ) ;
#12302 = CARTESIAN_POINT ( 'NONE',  ( 9.641350810849047548, 17.66889113945805789, -17.92981046679734547 ) ) ;
#12303 = PRODUCT_RELATED_PRODUCT_CATEGORY ( 'part', '', ( #28886 ) ) ;
#12304 = VECTOR ( 'NONE', #4907, 1000.000000000000000 ) ;
#12305 = DIRECTION ( 'NONE',  ( 0.5877852522924731371, 0.000000000000000000, 0.8090169943749474513 ) ) ;
#12306 = CARTESIAN_POINT ( 'NONE',  ( 152.0152310637605808, -1.999999999999974465, -34.70218595412750773 ) ) ;
#12307 = CARTESIAN_POINT ( 'NONE',  ( 13.11043623405165448, 8.565188957795726310, -15.92239833454181230 ) ) ;
#12308 = CARTESIAN_POINT ( 'NONE',  ( 157.0152310637604955, -1.999999999999974021, -17.38167787843871182 ) ) ;
#12309 = LINE ( 'NONE', #19330, #28593 ) ;
#12310 = ORIENTED_EDGE ( 'NONE', *, *, #4611, .T. ) ;
#12311 = ORIENTED_EDGE ( 'NONE', *, *, #26083, .T. ) ;
#12312 = DIRECTION ( 'NONE',  ( -0.8090169943749474513, -2.183098979609982436E-16, -0.5877852522924731371 ) ) ;
#12313 = ORIENTED_EDGE ( 'NONE', *, *, #4123, .T. ) ;
#12314 = ORIENTED_EDGE ( 'NONE', *, *, #12592, .F. ) ;
#12315 = CARTESIAN_POINT ( 'NONE',  ( 11.96143972814086531, 7.837808674300617007, -16.77422427047595477 ) ) ;
#12316 = CARTESIAN_POINT ( 'NONE',  ( 23.79992313191835507, -8.927985498448517632, -17.01055530912027791 ) ) ;
#12317 = CARTESIAN_POINT ( 'NONE',  ( 20.53420570626898822, -0.4664991210283321310, -19.04361528682417415 ) ) ;
#12318 = CARTESIAN_POINT ( 'NONE',  ( 171.1922820468852819, -1.999999999999971356, -4.936203717676158398 ) ) ;
#12319 = CARTESIAN_POINT ( 'NONE',  ( -11.85189716074913058, -5.341585316273319783, 4.999999999999998224 ) ) ;
#12320 = DIRECTION ( 'NONE',  ( -0.9510565162951536422, -2.566386769018988816E-16, -0.3090169943749472292 ) ) ;
#12321 = VERTEX_POINT ( 'NONE', #3513 ) ;
#12322 = ORIENTED_EDGE ( 'NONE', *, *, #3151, .T. ) ;
#12323 = LINE ( 'NONE', #21638, #3576 ) ;
#12324 = CARTESIAN_POINT ( 'NONE',  ( 157.2287565553229740, -10.00000000000000000, -20.83012701892220520 ) ) ;
#12325 = PLANE ( 'NONE',  #19965 ) ;
#12326 = DIRECTION ( 'NONE',  ( -0.8090169943749474513, -2.183098979609982436E-16, -0.5877852522924731371 ) ) ;
#12327 = DIRECTION ( 'NONE',  ( -0.000000000000000000, -0.000000000000000000, -1.000000000000000000 ) ) ;
#12328 = AXIS2_PLACEMENT_3D ( 'NONE', #7985, #26630, #3718 ) ;
#12329 = CARTESIAN_POINT ( 'NONE',  ( 10.48009811366078381, 16.41514476298091907, -17.33146409796769660 ) ) ;
#12330 = EDGE_CURVE ( 'NONE', #9369, #19861, #26566, .T. ) ;
#12331 = EDGE_CURVE ( 'NONE', #21151, #14407, #15237, .T. ) ;
#12332 = PLANE ( 'NONE',  #23844 ) ;
#12333 = CARTESIAN_POINT ( 'NONE',  ( 35.37764311538968087, -21.41652447078215005, -19.89511094362359955 ) ) ;
#12334 = ORIENTED_EDGE ( 'NONE', *, *, #10309, .F. ) ;
#12335 = CARTESIAN_POINT ( 'NONE',  ( 13.41328399211976397, 7.640833942120977440, -15.68103545992656578 ) ) ;
#12336 = EDGE_CURVE ( 'NONE', #1843, #15349, #12652, .T. ) ;
#12337 = CARTESIAN_POINT ( 'NONE',  ( 136.1922820468854241, -10.00000000000000533, -22.25671179336495697 ) ) ;
#12338 = EDGE_CURVE ( 'NONE', #5003, #280, #3660, .T. ) ;
#12339 = CARTESIAN_POINT ( 'NONE',  ( 23.56138260001205964, -6.829566487537672259, -18.05074380722902916 ) ) ;
#12340 = CARTESIAN_POINT ( 'NONE',  ( 12.85916040382217318, 9.514151651470600157, -16.12251888295402580 ) ) ;
#12341 = DIRECTION ( 'NONE',  ( -1.110223024625156540E-16, 0.000000000000000000, -1.000000000000000000 ) ) ;
#12342 = ORIENTED_EDGE ( 'NONE', *, *, #20669, .F. ) ;
#12343 = ORIENTED_EDGE ( 'NONE', *, *, #16658, .T. ) ;
#12344 = CARTESIAN_POINT ( 'NONE',  ( 11.47219014545126647, 9.272428573238919114, -15.86119603109536058 ) ) ;
#12345 = CARTESIAN_POINT ( 'NONE',  ( 151.1922820468853956, -1.999999999999976241, -13.59645775552055902 ) ) ;
#12346 = CARTESIAN_POINT ( 'NONE',  ( 9.915538251416846194, 16.41143258624473233, -16.50493629029764264 ) ) ;
#12347 = CARTESIAN_POINT ( 'NONE',  ( 130.7287565553229456, -10.00000000000000888, -2.233642730705364343 ) ) ;
#12348 = ORIENTED_EDGE ( 'NONE', *, *, #16347, .F. ) ;
#12349 = CARTESIAN_POINT ( 'NONE',  ( 149.5152310637605240, -10.00000000000000178, -2.627941064794695691 ) ) ;
#12350 = ORIENTED_EDGE ( 'NONE', *, *, #13852, .F. ) ;
#12351 = CARTESIAN_POINT ( 'NONE',  ( 12.03842576178837298, 9.272001309349649389, -16.68677036593512497 ) ) ;
#12352 = EDGE_LOOP ( 'NONE', ( #8825, #29900, #27229, #19278 ) ) ;
#12353 = CARTESIAN_POINT ( 'NONE',  ( 36.52535953212831998, -23.08013608362457703, -19.17046861472280028 ) ) ;
#12354 = CARTESIAN_POINT ( 'NONE',  ( 24.78692427941192733, -9.284778175067517125, -17.23615439686343720 ) ) ;
#12355 = CARTESIAN_POINT ( 'NONE',  ( 14.78952226657687063, 10.37904477376192069, -15.12939866669752575 ) ) ;
#12356 = ORIENTED_EDGE ( 'NONE', *, *, #15375, .T. ) ;
#12357 = ORIENTED_EDGE ( 'NONE', *, *, #10828, .T. ) ;
#12358 = DIRECTION ( 'NONE',  ( -1.734723475976807587E-16, 0.000000000000000000, -1.000000000000000000 ) ) ;
#12359 = VECTOR ( 'NONE', #26871, 1000.000000000000000 ) ;
#12360 = ORIENTED_EDGE ( 'NONE', *, *, #2557, .F. ) ;
#12361 = CARTESIAN_POINT ( 'NONE',  ( 33.30032953382602301, -10.37518355935928938, -17.98954529685971337 ) ) ;
#12362 = CONTEXT_DEPENDENT_SHAPE_REPRESENTATION ( #9865, #29902 ) ;
#12363 = CARTESIAN_POINT ( 'NONE',  ( 17.95893182911733277, 3.791778598950861667, -15.25628287466289024 ) ) ;
#12364 = CARTESIAN_POINT ( 'NONE',  ( 18.55171814111300321, 6.637122934506423988, -19.73184648383247364 ) ) ;
#12365 = LINE ( 'NONE', #3238, #14420 ) ;
#12366 = FACE_BOUND ( 'NONE', #27036, .T. ) ;
#12367 = VERTEX_POINT ( 'NONE', #623 ) ;
#12368 = DIRECTION ( 'NONE',  ( 0.9510565162951536422, 2.566386769018988816E-16, 0.3090169943749472292 ) ) ;
#12369 = DIRECTION ( 'NONE',  ( 0.000000000000000000, 0.000000000000000000, -1.000000000000000000 ) ) ;
#12370 = DIRECTION ( 'NONE',  ( -0.5877852522924731371, 0.000000000000000000, 0.8090169943749474513 ) ) ;
#12371 = EDGE_CURVE ( 'NONE', #21981, #3855, #19218, .T. ) ;
#12372 = CARTESIAN_POINT ( 'NONE',  ( 174.5152310637604387, -1.999999999999969580, -11.28819510263909542 ) ) ;
#12373 = VECTOR ( 'NONE', #11218, 1000.000000000000000 ) ;
#12374 = EDGE_CURVE ( 'NONE', #9954, #24408, #23981, .T. ) ;
#12375 = ADVANCED_FACE ( 'NONE', ( #19523 ), #28894, .T. ) ;
#12376 = ADVANCED_BREP_SHAPE_REPRESENTATION ( '', ( #1835, #13190 ), #496 ) ;
#12377 = CARTESIAN_POINT ( 'NONE',  ( 12.27584558688950978, 9.498490731067679604, -15.31120835137462244 ) ) ;
#12378 = DIRECTION ( 'NONE',  ( 1.000000000000000000, 4.440892098500622217E-16, 0.000000000000000000 ) ) ;
#12379 = ORIENTED_EDGE ( 'NONE', *, *, #7439, .T. ) ;
#12380 = CARTESIAN_POINT ( 'NONE',  ( 144.5152310637605808, -10.00000000000000355, -11.28819510263909542 ) ) ;
#12381 = VERTEX_POINT ( 'NONE', #29815 ) ;
#12382 = CARTESIAN_POINT ( 'NONE',  ( 12.50076791318051761, 8.571041463825640250, -15.12956297801270900 ) ) ;
#12383 = VERTEX_POINT ( 'NONE', #3813 ) ;
#12384 = CARTESIAN_POINT ( 'NONE',  ( 20.14260469057294500, 4.737385465944226048, -19.07682320266127718 ) ) ;
#12385 = LINE ( 'NONE', #10091, #15615 ) ;
#12386 = CARTESIAN_POINT ( 'NONE',  ( 154.5152310637605524, -10.00000000000000000, -30.37205893520531319 ) ) ;
#12387 = CARTESIAN_POINT ( 'NONE',  ( 151.1922820468854525, -4.999999999999976907, -30.91696583120936026 ) ) ;
#12388 = ORIENTED_EDGE ( 'NONE', *, *, #103, .F. ) ;
#12389 = FACE_OUTER_BOUND ( 'NONE', #17554, .T. ) ;
#12390 = CARTESIAN_POINT ( 'NONE',  ( 11.53546837550287130, 15.48783886997274450, -16.67730506581143501 ) ) ;
#12391 = ORIENTED_EDGE ( 'NONE', *, *, #12414, .F. ) ;
#12392 = CARTESIAN_POINT ( 'NONE',  ( 35.40392844931823646, -20.53461055239511879, -19.22110946685632271 ) ) ;
#12393 = CARTESIAN_POINT ( 'NONE',  ( 15.39489021548154568, 6.697694061803245447, -14.95590323207311734 ) ) ;
#12394 = ORIENTED_EDGE ( 'NONE', *, *, #6602, .F. ) ;
#12395 = FACE_OUTER_BOUND ( 'NONE', #5769, .T. ) ;
#12396 = CARTESIAN_POINT ( 'NONE',  ( 18.55888777153046121, 10.80885496093247689, -16.87139299526244685 ) ) ;
#12397 = ORIENTED_EDGE ( 'NONE', *, *, #26650, .T. ) ;
#12398 = DIRECTION ( 'NONE',  ( -1.000000000000000000, 0.000000000000000000, 0.000000000000000000 ) ) ;
#12399 = CARTESIAN_POINT ( 'NONE',  ( 20.97149233804390533, -0.06858483505933390956, -19.21322127741759189 ) ) ;
#12400 = CARTESIAN_POINT ( 'NONE',  ( 18.06018518654990856, -2.098401534709970928, -17.02619504079518364 ) ) ;
#12401 = VECTOR ( 'NONE', #7547, 1000.000000000000000 ) ;
#12402 = LINE ( 'NONE', #23883, #7451 ) ;
#12403 = EDGE_LOOP ( 'NONE', ( #5916, #15109, #7349, #21329 ) ) ;
#12404 = ORIENTED_EDGE ( 'NONE', *, *, #1892, .F. ) ;
#12405 = CARTESIAN_POINT ( 'NONE',  ( 8.000000000000000000, 9.797174393178825657E-16, 18.00000000000000000 ) ) ;
#12406 = CARTESIAN_POINT ( 'NONE',  ( 163.6922820468853388, -4.999999999999973355, -17.92658477444275889 ) ) ;
#12407 = LINE ( 'NONE', #5560, #29605 ) ;
#12408 = DIRECTION ( 'NONE',  ( -2.698458740408365879E-16, 1.000000000000000000, 0.000000000000000000 ) ) ;
#12409 = EDGE_CURVE ( 'NONE', #10981, #28540, #13106, .T. ) ;
#12410 = ADVANCED_FACE ( 'NONE', ( #24879 ), #20339, .T. ) ;
#12411 = CARTESIAN_POINT ( 'NONE',  ( 0.000000000000000000, 0.000000000000000000, 0.000000000000000000 ) ) ;
#12412 = ADVANCED_FACE ( 'NONE', ( #1990 ), #24726, .T. ) ;
#12413 = CARTESIAN_POINT ( 'NONE',  ( 11.31072706937237982, 10.01291882189198112, -15.92796669285280764 ) ) ;
#12414 = EDGE_CURVE ( 'NONE', #18724, #11499, #6550, .T. ) ;
#12415 = CARTESIAN_POINT ( 'NONE',  ( 28.13717792526295014, -10.23527491042630011, -17.83415580063453376 ) ) ;
#12416 = CARTESIAN_POINT ( 'NONE',  ( 26.09074415779471323, -5.786596670875995940, -12.76770422508296932 ) ) ;
#12418 = VERTEX_POINT ( 'NONE', #25027 ) ;
#12417 = CARTESIAN_POINT ( 'NONE',  ( 33.38708106686501509, -12.47399286361455850, -19.70456970583452616 ) ) ;
#12419 = CARTESIAN_POINT ( 'NONE',  ( 169.7287565553229740, -1.999999999999969580, -33.82050807568879947 ) ) ;
#12420 = CARTESIAN_POINT ( 'NONE',  ( 0.000000000000000000, 0.000000000000000000, -18.00000000000000000 ) ) ;
#12421 = CARTESIAN_POINT ( 'NONE',  ( 149.5152310637605808, -10.00000000000000178, -19.94844914048349693 ) ) ;
#12422 = CARTESIAN_POINT ( 'NONE',  ( 166.1922820468853104, -4.999999999999973355, -4.936203717676158398 ) ) ;
#12423 = CARTESIAN_POINT ( 'NONE',  ( 157.0152310637604955, -10.00000000000000000, -17.38167787843871182 ) ) ;
#12424 = LINE ( 'NONE', #2684, #20252 ) ;
#12425 = CARTESIAN_POINT ( 'NONE',  ( 21.10023079691774228, -0.4353598523292347422, -20.14113737667230097 ) ) ;
#12426 = ORIENTED_EDGE ( 'NONE', *, *, #5742, .F. ) ;
#12427 = PLANE ( 'NONE',  #13912 ) ;
#12428 = CARTESIAN_POINT ( 'NONE',  ( 12.26149629667000340, 9.515828874666294013, -15.32083899563621898 ) ) ;
#12429 = CARTESIAN_POINT ( 'NONE',  ( 4.250000000000003553, 1.887379141862766119E-15, -0.5251556536572770106 ) ) ;
#12430 = CARTESIAN_POINT ( 'NONE',  ( 139.5152310637606092, -4.999999999999980460, -19.94844914048349338 ) ) ;
#12431 = CARTESIAN_POINT ( 'NONE',  ( 21.19279910686179846, 4.720633506281588510, -19.26595127233560234 ) ) ;
#12432 = CARTESIAN_POINT ( 'NONE',  ( 18.99162967131814028, 0.6168208955672017657, -19.54819510397825510 ) ) ;
#12433 = ORIENTED_EDGE ( 'NONE', *, *, #19276, .F. ) ;
#12434 = CARTESIAN_POINT ( 'NONE',  ( 35.45944968151609800, -21.78403803824750185, -19.54251958818673174 ) ) ;
#12435 = CARTESIAN_POINT ( 'NONE',  ( 27.61464345320196045, -4.235915813641956795, -14.29244051139929894 ) ) ;
#12436 = CARTESIAN_POINT ( 'NONE',  ( 20.92249676953290916, 2.861121271339598593, -14.71414025844469720 ) ) ;
#12437 = VECTOR ( 'NONE', #10840, 1000.000000000000000 ) ;
#12438 = ADVANCED_FACE ( 'NONE', ( #22432 ), #1535, .F. ) ;
#12439 = LINE ( 'NONE', #3756, #15253 ) ;
#12440 = ORIENTED_EDGE ( 'NONE', *, *, #25211, .F. ) ;
#12441 = FACE_OUTER_BOUND ( 'NONE', #29387, .T. ) ;
#12442 = CARTESIAN_POINT ( 'NONE',  ( 134.7287565553230024, -10.00000000000000711, -25.16025403784439973 ) ) ;
#12443 = CARTESIAN_POINT ( 'NONE',  ( 173.6922820468852535, -1.999999999999970912, -0.6060766987539614181 ) ) ;
#12444 = EDGE_CURVE ( 'NONE', #17847, #21366, #29660, .T. ) ;
#12445 = EDGE_CURVE ( 'NONE', #5191, #3131, #20127, .T. ) ;
#12446 = CARTESIAN_POINT ( 'NONE',  ( 18.55888777153046121, 10.80885496093247689, -16.87139299526244685 ) ) ;
#12447 = AXIS2_PLACEMENT_3D ( 'NONE', #27749, #27903, #30210 ) ;
#12448 = CARTESIAN_POINT ( 'NONE',  ( 36.54859390953724585, -22.18451583373416014, -18.06010107863414405 ) ) ;
#12449 = CARTESIAN_POINT ( 'NONE',  ( 9.745779815811758340, 17.18996641109745482, -16.82979807527155458 ) ) ;
#12450 = VECTOR ( 'NONE', #19779, 1000.000000000000000 ) ;
#12451 = CARTESIAN_POINT ( 'NONE',  ( 164.7287565553229740, -9.999999999999998224, -33.82050807568879947 ) ) ;
#12452 = CARTESIAN_POINT ( 'NONE',  ( 172.0152310637605240, -4.999999999999971578, -32.93883019725009120 ) ) ;
#12453 = CARTESIAN_POINT ( 'NONE',  ( 12.05017172662707381, 9.228765020691243492, -16.68110209197688221 ) ) ;
#12454 = CARTESIAN_POINT ( 'NONE',  ( 174.7287565553228603, -1.999999999999969580, -7.839745962155603820 ) ) ;
#12455 = CARTESIAN_POINT ( 'NONE',  ( 162.2287565553229172, -1.999999999999972689, -12.16987298107780369 ) ) ;
#12456 = ORIENTED_EDGE ( 'NONE', *, *, #25339, .F. ) ;
#12457 = EDGE_LOOP ( 'NONE', ( #22622, #21655, #3735, #16470 ) ) ;
#12458 = VECTOR ( 'NONE', #2845, 1000.000000000000000 ) ;
#12459 = PLANE ( 'NONE',  #18295 ) ;
#12460 = CARTESIAN_POINT ( 'NONE',  ( 152.0152310637604955, -1.999999999999976241, 1.702185954127501066 ) ) ;
#12461 = CIRCLE ( 'NONE', #26133, 13.00000000000000178 ) ;
#12462 = CARTESIAN_POINT ( 'NONE',  ( 172.2287565553228603, -9.999999999999996447, -3.509618943233403510 ) ) ;
#12463 = ORIENTED_EDGE ( 'NONE', *, *, #18173, .T. ) ;
#12464 = VERTEX_POINT ( 'NONE', #17829 ) ;
#12465 = ORIENTED_EDGE ( 'NONE', *, *, #9203, .F. ) ;
#12466 = VERTEX_POINT ( 'NONE', #3967 ) ;
#12467 = CARTESIAN_POINT ( 'NONE',  ( 11.46306169112780537, 8.437560028716553973, -17.10890052424691632 ) ) ;
#12468 = VECTOR ( 'NONE', #28037, 1000.000000000000000 ) ;
#12469 = CARTESIAN_POINT ( 'NONE',  ( 26.67611703245768950, -12.21101477627283849, -12.48819288018415108 ) ) ;
#12470 = CARTESIAN_POINT ( 'NONE',  ( 25.46127020808262387, -4.208148299910691392, -19.59612275642668777 ) ) ;
#12471 = DIRECTION ( 'NONE',  ( 0.9510565162951535312, 2.566386769018988816E-16, -0.3090169943749475623 ) ) ;
#12472 = CARTESIAN_POINT ( 'NONE',  ( -13.00000000000000178, -2.870178842070716726E-15, 18.00000000000000000 ) ) ;
#12473 = PLANE ( 'NONE',  #614 ) ;
#12474 = ADVANCED_FACE ( 'NONE', ( #13559 ), #18136, .T. ) ;
#12475 = VECTOR ( 'NONE', #6817, 1000.000000000000000 ) ;
#12476 = PLANE ( 'NONE',  #11838 ) ;
#12477 = FACE_OUTER_BOUND ( 'NONE', #24459, .T. ) ;
#12478 = PLANE ( 'NONE',  #21430 ) ;
#12479 = CIRCLE ( 'NONE', #13937, 2.000000000000000000 ) ;
#12480 = CARTESIAN_POINT ( 'NONE',  ( 0.000000000000000000, 0.000000000000000000, -23.00000000000000000 ) ) ;
#12482 = CARTESIAN_POINT ( 'NONE',  ( 139.5152310637605524, -10.00000000000000533, -4.391296821672111328 ) ) ;
#12481 = CIRCLE ( 'NONE', #29627, 8.000000000000007105 ) ;
#12483 = CARTESIAN_POINT ( 'NONE',  ( 10.47193650065820592, 16.45257496057443802, -17.33483926051624735 ) ) ;
#12484 = CARTESIAN_POINT ( 'NONE',  ( 32.91905456285188336, -11.74221475484424104, -17.14214516703887980 ) ) ;
#12485 = ORIENTED_EDGE ( 'NONE', *, *, #27938, .T. ) ;
#12486 = CARTESIAN_POINT ( 'NONE',  ( 9.193626274318058123, 15.80945627937554576, -17.02118864906812234 ) ) ;
#12487 = PRODUCT_DEFINITION_SHAPE ( 'NONE', 'NONE',  #26898 ) ;
#12488 = CARTESIAN_POINT ( 'NONE',  ( 25.23810427664335165, -6.496417100615061280, -13.69959235629456629 ) ) ;
#12489 = CARTESIAN_POINT ( 'NONE',  ( 12.83296646064745339, 9.537815246119466295, -16.14070827264395547 ) ) ;
#12490 = FACE_BOUND ( 'NONE', #1521, .T. ) ;
#12491 = VERTEX_POINT ( 'NONE', #19978 ) ;
#12492 = PLANE ( 'NONE',  #2377 ) ;
#12493 = CIRCLE ( 'NONE', #24703, 8.000000000000000000 ) ;
#12494 = CARTESIAN_POINT ( 'NONE',  ( 12.46899830068120352, 8.557956911948249257, -15.15481108270911825 ) ) ;
#12495 = FACE_OUTER_BOUND ( 'NONE', #15933, .T. ) ;
#12496 = VERTEX_POINT ( 'NONE', #10671 ) ;
#12497 = PLANE ( 'NONE',  #9579 ) ;
#12498 = ORIENTED_EDGE ( 'NONE', *, *, #28580, .T. ) ;
#12499 = CARTESIAN_POINT ( 'NONE',  ( 12.56022695423237145, 8.580358410770909217, -16.34122335808152826 ) ) ;
#12500 = ORIENTED_EDGE ( 'NONE', *, *, #1587, .F. ) ;
#12502 = CARTESIAN_POINT ( 'NONE',  ( 34.26516872548082659, -12.92629604573065549, -20.94206068969455004 ) ) ;
#12501 = VECTOR ( 'NONE', #17685, 1000.000000000000000 ) ;
#12503 = CARTESIAN_POINT ( 'NONE',  ( 26.48263329513011755, -12.06126822337667903, -13.95730679897583038 ) ) ;
#12504 = CARTESIAN_POINT ( 'NONE',  ( 26.38113052396219516, -11.59678093645141672, -17.84452879788985769 ) ) ;
#12505 = VECTOR ( 'NONE', #16669, 1000.000000000000000 ) ;
#12506 = CARTESIAN_POINT ( 'NONE',  ( 177.2287565553228603, -9.999999999999994671, -12.16987298107780369 ) ) ;
#12507 = ORIENTED_EDGE ( 'NONE', *, *, #21765, .T. ) ;
#12508 = CARTESIAN_POINT ( 'NONE',  ( 156.1922820468853956, -10.00000000000000000, -19.40354224447947828 ) ) ;
#12509 = ITEM_DEFINED_TRANSFORMATION ( 'NONE', 'NONE', #9730,  #13190 ) ;
#12510 = EDGE_CURVE ( 'NONE', #590, #13010, #13265, .T. ) ;
#12511 = EDGE_CURVE ( 'NONE', #13196, #12109, #10964, .T. ) ;
#12512 = CARTESIAN_POINT ( 'NONE',  ( 20.49785840140504689, 4.750029832917431527, -16.36601636927073145 ) ) ;
#12513 = ADVANCED_FACE ( 'NONE', ( #6409 ), #15698, .T. ) ;
#12514 = CARTESIAN_POINT ( 'NONE',  ( 19.11618317516819587, 7.271703427217982352, -19.10559232466456692 ) ) ;
#12515 = VERTEX_POINT ( 'NONE', #20424 ) ;
#12516 = CARTESIAN_POINT ( 'NONE',  ( 2.500000000000002665, 1.416384724411995397E-15, -2.424599999999998978 ) ) ;
#12517 = FACE_BOUND ( 'NONE', #25462, .T. ) ;
#12518 = VECTOR ( 'NONE', #7072, 1000.000000000000000 ) ;
#12519 = CARTESIAN_POINT ( 'NONE',  ( 134.7287565553230024, -1.999999999999980460, -16.50000000000000000 ) ) ;
#12520 = LINE ( 'NONE', #21393, #19904 ) ;
#12521 = DIRECTION ( 'NONE',  ( 0.000000000000000000, 0.000000000000000000, 1.000000000000000000 ) ) ;
#12522 = VECTOR ( 'NONE', #18522, 1000.000000000000000 ) ;
#12523 = CARTESIAN_POINT ( 'NONE',  ( 139.7287565553230309, -10.00000000000000533, -16.50000000000000000 ) ) ;
#12524 = CARTESIAN_POINT ( 'NONE',  ( 12.26149629667000340, 9.515828874666294013, -15.32083899563621898 ) ) ;
#12525 = DIRECTION ( 'NONE',  ( -0.9510565162951536422, 0.000000000000000000, -0.3090169943749472292 ) ) ;
#12526 = VECTOR ( 'NONE', #27096, 1000.000000000000000 ) ;
#12527 = CARTESIAN_POINT ( 'NONE',  ( 137.0152310637606092, -10.00000000000000533, -6.958068083716895558 ) ) ;
#12528 = ORIENTED_EDGE ( 'NONE', *, *, #22032, .T. ) ;
#12529 = CARTESIAN_POINT ( 'NONE',  ( 12.50098444160134470, 8.571137227758441668, -15.12939039523150520 ) ) ;
#12530 = EDGE_LOOP ( 'NONE', ( #26914, #26459, #16262, #7295 ) ) ;
#12531 = CARTESIAN_POINT ( 'NONE',  ( 11.68234546060339163, 7.643720436761259229, -15.74430661255668262 ) ) ;
#12532 = CARTESIAN_POINT ( 'NONE',  ( 163.6922820468853104, -1.999999999999973133, -6.413161187712876909 ) ) ;
#12533 = PLANE ( 'NONE',  #23257 ) ;
#12534 = LINE ( 'NONE', #10397, #3917 ) ;
#12535 = ORIENTED_EDGE ( 'NONE', *, *, #21229, .F. ) ;
#12536 = CARTESIAN_POINT ( 'NONE',  ( 130.7287565553229172, -4.999999999999983125, -33.50000000000000000 ) ) ;
#12537 = ORIENTED_EDGE ( 'NONE', *, *, #20651, .T. ) ;
#12538 = CARTESIAN_POINT ( 'NONE',  ( 12.85536779349230052, 9.514564043964993445, -16.12538237964846388 ) ) ;
#12539 = ORIENTED_EDGE ( 'NONE', *, *, #22246, .F. ) ;
#12540 = CARTESIAN_POINT ( 'NONE',  ( 34.07550722110926955, -11.19626532300822674, -18.14763417942564061 ) ) ;
#12541 = CARTESIAN_POINT ( 'NONE',  ( 17.85084670134855145, 5.929878015568476712, -20.08862479909851828 ) ) ;
#12542 = ORIENTED_EDGE ( 'NONE', *, *, #22205, .T. ) ;
#12543 = VECTOR ( 'NONE', #26368, 999.9999999999998863 ) ;
#12544 = LINE ( 'NONE', #21863, #19872 ) ;
#12545 = CARTESIAN_POINT ( 'NONE',  ( 17.10097030076851610, 6.697663726599960121, -13.82760435466811089 ) ) ;
#12546 = CARTESIAN_POINT ( 'NONE',  ( 3.999999999999980904, -2.309401076758567317, -0.3572655899081716435 ) ) ;
#12547 = EDGE_CURVE ( 'NONE', #17432, #12041, #27498, .T. ) ;
#12548 = CARTESIAN_POINT ( 'NONE',  ( 26.02348467347448491, -3.622150272347476108, -19.21400332953221124 ) ) ;
#12549 = VECTOR ( 'NONE', #2334, 1000.000000000000000 ) ;
#12550 = EDGE_CURVE ( 'NONE', #2172, #29884, #12900, .T. ) ;
#12551 = CARTESIAN_POINT ( 'NONE',  ( 18.39947282702827991, 3.040288584705510999, -19.58888106367123427 ) ) ;
#12552 = EDGE_CURVE ( 'NONE', #6921, #15438, #19619, .T. ) ;
#12553 = ORIENTED_EDGE ( 'NONE', *, *, #3952, .T. ) ;
#12554 = EDGE_CURVE ( 'NONE', #3882, #14836, #28679, .T. ) ;
#12555 = VERTEX_POINT ( 'NONE', #1323 ) ;
#12556 = DIRECTION ( 'NONE',  ( -2.698458740408365879E-16, 1.000000000000000000, 0.000000000000000000 ) ) ;
#12557 = CARTESIAN_POINT ( 'NONE',  ( 130.7287565553229456, -4.999999999999983125, 3.500000000000003109 ) ) ;
#12558 = DIRECTION ( 'NONE',  ( 1.110223024625156540E-16, 2.995891024602366092E-32, 1.000000000000000000 ) ) ;
#12559 = LINE ( 'NONE', #21877, #27780 ) ;
#12560 = DIRECTION ( 'NONE',  ( -0.9510565162951536422, -2.566386769018988323E-16, 0.3090169943749475623 ) ) ;
#12561 = VECTOR ( 'NONE', #20905, 1000.000000000000000 ) ;
#12562 = CARTESIAN_POINT ( 'NONE',  ( 11.40798482813988635, 9.566882342703072695, -15.88774718835883348 ) ) ;
#12563 = CARTESIAN_POINT ( 'NONE',  ( 26.47302276827314671, -6.985584592454325836, -13.42065591321591711 ) ) ;
#12564 = CARTESIAN_POINT ( 'NONE',  ( 25.66600519952783799, -8.909200411882650883, -19.30012332941604924 ) ) ;
#12566 = VERTEX_POINT ( 'NONE', #26831 ) ;
#12565 = CARTESIAN_POINT ( 'NONE',  ( 31.39893620166130717, -10.86152586746012183, -14.84747879817187943 ) ) ;
#12567 = CARTESIAN_POINT ( 'NONE',  ( 103.6655236389851069, -4.999999999999989342, 75.31741161166775100 ) ) ;
#12568 = VECTOR ( 'NONE', #21038, 1000.000000000000000 ) ;
#12569 = LINE ( 'NONE', #5419, #2879 ) ;
#12570 = CARTESIAN_POINT ( 'NONE',  ( 157.2287565553229172, -10.00000000000000178, -3.509618943233403510 ) ) ;
#12571 = CARTESIAN_POINT ( 'NONE',  ( -8.000000000000003553, -4.618802153517037823, -4.285468820183664818 ) ) ;
#12572 = LINE ( 'NONE', #21891, #26362 ) ;
#12573 = CARTESIAN_POINT ( 'NONE',  ( 134.7287565553230024, -1.999999999999980460, -7.839745962155602044 ) ) ;
#12574 = CARTESIAN_POINT ( 'NONE',  ( 19.83745040964868522, -2.306422872736943575, -14.39351019504378293 ) ) ;
#12575 = ORIENTED_EDGE ( 'NONE', *, *, #27973, .T. ) ;
#12576 = LINE ( 'NONE', #29112, #7610 ) ;
#12577 = CARTESIAN_POINT ( 'NONE',  ( 12.23642031952448406, 9.680328234467932447, -15.32743366668982432 ) ) ;
#12578 = CONICAL_SURFACE ( 'NONE', #8679, 8.000000000000007105, 1.047197551196596077 ) ;
#12579 = CARTESIAN_POINT ( 'NONE',  ( 0.000000000000000000, 0.000000000000000000, 0.000000000000000000 ) ) ;
#12580 = CARTESIAN_POINT ( 'NONE',  ( 141.1922820468853956, -1.999999999999979128, -2.083034168790675267 ) ) ;
#12581 = ORIENTED_EDGE ( 'NONE', *, *, #1373, .T. ) ;
#12582 = ORIENTED_EDGE ( 'NONE', *, *, #16268, .F. ) ;
#12583 = CARTESIAN_POINT ( 'NONE',  ( 16.89369580670022941, 0.5033910033923695293, -17.32063897790030893 ) ) ;
#12584 = CARTESIAN_POINT ( 'NONE',  ( 18.25722813608836859, -0.08152059447761372812, -18.39925177747023710 ) ) ;
#12585 = ORIENTED_EDGE ( 'NONE', *, *, #2713, .F. ) ;
#12586 = CARTESIAN_POINT ( 'NONE',  ( 35.07504771885155037, -20.05712364337910714, -20.21480690768607857 ) ) ;
#12587 =( LENGTH_UNIT ( ) NAMED_UNIT ( * ) SI_UNIT ( .MILLI., .METRE. ) );
#12588 = CARTESIAN_POINT ( 'NONE',  ( 25.85951265464835203, -2.375871015539448461, -16.96122936427994787 ) ) ;
#12589 = CARTESIAN_POINT ( 'NONE',  ( 22.33422182767193576, -8.475443503041637072, -15.36134680393336538 ) ) ;
#12590 = ADVANCED_FACE ( 'NONE', ( #13053 ), #871, .T. ) ;
#12591 = VECTOR ( 'NONE', #13403, 1000.000000000000000 ) ;
#12592 = EDGE_CURVE ( 'NONE', #1878, #6853, #19318, .T. ) ;
#12593 = ADVANCED_FACE ( 'NONE', ( #24070 ), #10615, .T. ) ;
#12594 = EDGE_CURVE ( 'NONE', #18794, #4418, #17329, .T. ) ;
#12595 = CARTESIAN_POINT ( 'NONE',  ( 21.94319337455657859, -4.318501116253552041, -18.82930321547734920 ) ) ;
#12596 = VECTOR ( 'NONE', #10797, 1000.000000000000000 ) ;
#12597 = CARTESIAN_POINT ( 'NONE',  ( 4.873852431642221816, -5.000000000000015987, 15.00017539148683454 ) ) ;
#12598 = VECTOR ( 'NONE', #12175, 1000.000000000000000 ) ;
#12599 = CIRCLE ( 'NONE', #22861, 5.000000000000000000 ) ;
#12600 =( NAMED_UNIT ( * ) SI_UNIT ( $, .STERADIAN. ) SOLID_ANGLE_UNIT ( ) );
#12601 = PLANE ( 'NONE',  #4773 ) ;
#12602 = CARTESIAN_POINT ( 'NONE',  ( 154.5152310637605808, -10.00000000000000000, -28.60870317832789667 ) ) ;
#12603 = CARTESIAN_POINT ( 'NONE',  ( 16.06097560829885040, 7.604535090956617616, -20.76572858943923094 ) ) ;
#12604 = CARTESIAN_POINT ( 'NONE',  ( 36.48591233058812833, -21.90292070287360460, -19.44112467175505898 ) ) ;
#12605 = CARTESIAN_POINT ( 'NONE',  ( 9.916953853453376766, 16.40494045485788632, -16.50434094533541085 ) ) ;
#12606 = DIRECTION ( 'NONE',  ( 0.5877852522924731371, 0.000000000000000000, 0.8090169943749474513 ) ) ;
#12607 = PLANE ( 'NONE',  #26119 ) ;
#12608 = CARTESIAN_POINT ( 'NONE',  ( 12.04525852301462585, 9.245982119944198274, -16.68353927915122981 ) ) ;
#12609 = FACE_OUTER_BOUND ( 'NONE', #11538, .T. ) ;
#12610 = ORIENTED_EDGE ( 'NONE', *, *, #20161, .T. ) ;
#12611 = CYLINDRICAL_SURFACE ( 'NONE', #26681, 2.100000000000000977 ) ;
#12612 = VERTEX_POINT ( 'NONE', #7728 ) ;
#12613 = ORIENTED_EDGE ( 'NONE', *, *, #28003, .T. ) ;
#12614 = VECTOR ( 'NONE', #11952, 1000.000000000000000 ) ;
#12615 = CARTESIAN_POINT ( 'NONE',  ( 173.6922820468853388, -4.999999999999969802, -23.73366926340167637 ) ) ;
#12616 = DIRECTION ( 'NONE',  ( -2.698458740408365879E-16, 1.000000000000000000, 0.000000000000000000 ) ) ;
#12617 = PLANE ( 'NONE',  #27858 ) ;
#12618 = CIRCLE ( 'NONE', #19434, 2.041999999999999815 ) ;
#12619 = ORIENTED_EDGE ( 'NONE', *, *, #6123, .T. ) ;
#12620 = CARTESIAN_POINT ( 'NONE',  ( 12.94178543664954972, 7.512178771719595360, -16.05074886939826939 ) ) ;
#12621 = ORIENTED_EDGE ( 'NONE', *, *, #29485, .T. ) ;
#12622 = CARTESIAN_POINT ( 'NONE',  ( 28.02170931380428698, -7.325026966936788675, -12.85224998211816860 ) ) ;
#12623 = EDGE_CURVE ( 'NONE', #8261, #26148, #14876, .T. ) ;
#12624 = CARTESIAN_POINT ( 'NONE',  ( 27.71186802668094273, -7.007055141436442369, -19.33373627201896383 ) ) ;
#12625 = LINE ( 'NONE', #17656, #21876 ) ;
#12626 = PLANE ( 'NONE',  #25296 ) ;
#12627 = EDGE_CURVE ( 'NONE', #14866, #13813, #3173, .T. ) ;
#12628 = CARTESIAN_POINT ( 'NONE',  ( 149.7287565553230024, -1.999999999999975797, -16.50000000000000355 ) ) ;
#12629 = EDGE_CURVE ( 'NONE', #15955, #15809, #16953, .T. ) ;
#12630 = ORIENTED_EDGE ( 'NONE', *, *, #17914, .T. ) ;
#12631 = DIRECTION ( 'NONE',  ( 0.3090169943749472292, 8.338696094057992503E-17, -0.9510565162951536422 ) ) ;
#12632 = CARTESIAN_POINT ( 'NONE',  ( 152.0152310637605240, -1.999999999999975797, -6.958068083716895558 ) ) ;
#12633 = VECTOR ( 'NONE', #1557, 999.9999999999998863 ) ;
#12634 =( BOUNDED_CURVE ( )  B_SPLINE_CURVE ( 3, ( #15500, #27145, #29141, #26996 ),
 .UNSPECIFIED., .F., .F. ) 
 B_SPLINE_CURVE_WITH_KNOTS ( ( 4, 4 ),
 ( 1.734723475976807094E-18, 0.001563228649568139134 ),
 .UNSPECIFIED. ) 
 CURVE ( )  GEOMETRIC_REPRESENTATION_ITEM ( )  RATIONAL_B_SPLINE_CURVE ( ( 1.000000000000000000, 0.3333333333333345361, 0.3333333333333333703, 0.9999999999999987788 ) ) 
 REPRESENTATION_ITEM ( '' )  );
#12635 = DIRECTION ( 'NONE',  ( 0.9510565162951536422, 0.000000000000000000, -0.3090169943749475623 ) ) ;
#12636 = EDGE_LOOP ( 'NONE', ( #28657, #25704, #11882, #18494 ) ) ;
#12637 = DIRECTION ( 'NONE',  ( 1.000000000000000000, 4.440892098500622217E-16, 0.000000000000000000 ) ) ;
#12638 = CARTESIAN_POINT ( 'NONE',  ( 12.43045822248789456, -5.000000000000014211, 38.25701663089573401 ) ) ;
#12639 = AXIS2_PLACEMENT_3D ( 'NONE', #4986, #2571, #21466 ) ;
#12640 = CARTESIAN_POINT ( 'NONE',  ( 12.03006260835556951, 9.306948544855226046, -16.69048869075990638 ) ) ;
#12641 = CARTESIAN_POINT ( 'NONE',  ( 32.97927115036063839, -11.75136040154610662, -17.31233706439427067 ) ) ;
#12642 = VERTEX_POINT ( 'NONE', #1177 ) ;
#12643 = CARTESIAN_POINT ( 'NONE',  ( 9.113591243665672081, 16.17650713204097102, -17.05428594964136835 ) ) ;
#12644 = CARTESIAN_POINT ( 'NONE',  ( 27.31974442496251143, -5.660127319198639206, -14.41990313654811651 ) ) ;
#12645 = CARTESIAN_POINT ( 'NONE',  ( 12.83122539074939894, 9.545332027449857648, -16.14146395906381670 ) ) ;
#12646 = FACE_BOUND ( 'NONE', #18851, .T. ) ;
#12647 = ORIENTED_EDGE ( 'NONE', *, *, #5086, .F. ) ;
#12648 = EDGE_CURVE ( 'NONE', #5025, #23986, #29287, .T. ) ;
#12649 = ORIENTED_EDGE ( 'NONE', *, *, #24528, .T. ) ;
#12650 = CARTESIAN_POINT ( 'NONE',  ( 157.0152310637604955, -1.999999999999974021, -17.38167787843871182 ) ) ;
#12651 = CARTESIAN_POINT ( 'NONE',  ( 12.13006862794127017, 8.527244997094612700, -15.41586291625151972 ) ) ;
#12652 = LINE ( 'NONE', #29032, #18414 ) ;
#12653 = VERTEX_POINT ( 'NONE', #21769 ) ;
#12654 = LINE ( 'NONE', #5349, #350 ) ;
#12655 = ORIENTED_EDGE ( 'NONE', *, *, #9834, .T. ) ;
#12656 = VECTOR ( 'NONE', #3320, 1000.000000000000000 ) ;
#12657 = CARTESIAN_POINT ( 'NONE',  ( 12.03055882466574289, 9.304755949677762317, -16.69027714870545864 ) ) ;
#12658 = ORIENTED_EDGE ( 'NONE', *, *, #23456, .T. ) ;
#12659 = AXIS2_PLACEMENT_3D ( 'NONE', #3991, #18470, #13290 ) ;
#12660 = CARTESIAN_POINT ( 'NONE',  ( 19.69280650922798515, 8.111729275751024204, -19.45082099569356160 ) ) ;
#12661 = CARTESIAN_POINT ( 'NONE',  ( 29.82081855766934453, -7.722587238354316597, -15.76009366473342332 ) ) ;
#12662 = CARTESIAN_POINT ( 'NONE',  ( 159.5152310637604955, -1.999999999999973577, -11.28819510263909542 ) ) ;
#12663 = ORIENTED_EDGE ( 'NONE', *, *, #20036, .T. ) ;
#12664 = VECTOR ( 'NONE', #25453, 1000.000000000000000 ) ;
#12665 = CIRCLE ( 'NONE', #988, 13.00000000000000178 ) ;
#12666 = CARTESIAN_POINT ( 'NONE',  ( 13.00000000000000178, -2.870178842070716726E-15, -18.00000000000000000 ) ) ;
#12667 = PRODUCT_CONTEXT ( 'NONE', #13575, 'mechanical' ) ;
#12668 = CARTESIAN_POINT ( 'NONE',  ( 17.24163842130223046, 3.474294283696999219, -15.80253352452890425 ) ) ;
#12669 = CARTESIAN_POINT ( 'NONE',  ( 16.21960234321935701, 7.070186740785398882, -14.59618053200276044 ) ) ;
#12670 = B_SPLINE_CURVE_WITH_KNOTS ( 'NONE', 3,
 ( #3619, #14883, #10317, #6055, #5606, #1184 ),
 .UNSPECIFIED., .F., .F.,
 ( 4, 2, 4 ),
 ( 2.380731629581860062E-07, 0.002336973833157567678, 0.004673709593152178265 ),
 .UNSPECIFIED. ) ;
#12671 = DIRECTION ( 'NONE',  ( 0.9510565162951536422, 0.000000000000000000, -0.3090169943749475623 ) ) ;
#12672 = DIRECTION ( 'NONE',  ( 0.3090169943749472292, 8.338696094057992503E-17, -0.9510565162951536422 ) ) ;
#12673 = VECTOR ( 'NONE', #6021, 1000.000000000000000 ) ;
#12674 = AXIS2_PLACEMENT_3D ( 'NONE', #12239, #14966, #1117 ) ;
#12675 = FACE_OUTER_BOUND ( 'NONE', #23631, .T. ) ;
#12676 = PLANE ( 'NONE',  #13059 ) ;
#12677 = VECTOR ( 'NONE', #8180, 1000.000000000000000 ) ;
#12678 = FACE_OUTER_BOUND ( 'NONE', #20099, .T. ) ;
#12679 = LINE ( 'NONE', #21999, #8540 ) ;
#12680 = CARTESIAN_POINT ( 'NONE',  ( 12.27434273475605409, 9.502313893772186049, -15.31206391052669602 ) ) ;
#12681 = DIRECTION ( 'NONE',  ( 0.000000000000000000, 0.000000000000000000, -1.000000000000000000 ) ) ;
#12682 = ADVANCED_FACE ( 'NONE', ( #5902 ), #15183, .T. ) ;
#12683 = CARTESIAN_POINT ( 'NONE',  ( 136.1922820468854241, -1.999999999999980460, -2.083034168790677043 ) ) ;
#12684 = ORIENTED_EDGE ( 'NONE', *, *, #5122, .T. ) ;
#12685 = CARTESIAN_POINT ( 'NONE',  ( 12.63667343406881294, 8.631100619704961119, -15.02124387326777111 ) ) ;
#12686 = ADVANCED_FACE ( 'NONE', ( #26986 ), #1030, .F. ) ;
#12687 = CARTESIAN_POINT ( 'NONE',  ( 10.66927416475804158, 9.041953549878499530, -16.41095583421565962 ) ) ;
#12688 = DIRECTION ( 'NONE',  ( 0.000000000000000000, 0.000000000000000000, 1.000000000000000000 ) ) ;
#12689 = CARTESIAN_POINT ( 'NONE',  ( 132.0152310637605524, -10.00000000000000711, -8.721423840594310306 ) ) ;
#12690 = CARTESIAN_POINT ( 'NONE',  ( 152.2287565553229740, -10.00000000000000178, -12.16987298107780369 ) ) ;
#12691 = VERTEX_POINT ( 'NONE', #28840 ) ;
#12692 = CARTESIAN_POINT ( 'NONE',  ( 172.0152310637604387, -4.999999999999970690, -6.958068083716895558 ) ) ;
#12693 = ORIENTED_EDGE ( 'NONE', *, *, #18075, .T. ) ;
#12694 = CARTESIAN_POINT ( 'NONE',  ( 12.86387084073970222, 9.514634738764476296, -16.11888650007813339 ) ) ;
#12696 = VECTOR ( 'NONE', #15578, 1000.000000000000000 ) ;
#12695 = CARTESIAN_POINT ( 'NONE',  ( 34.53678113438137842, -12.15940631226206925, -18.93201839848989465 ) ) ;
#12697 = CARTESIAN_POINT ( 'NONE',  ( 17.21692058948253035, 4.245457944912791604, -14.13226496128363863 ) ) ;
#12698 = EDGE_LOOP ( 'NONE', ( #22927, #15226, #2811, #22697, #7967 ) ) ;
#12699 = CARTESIAN_POINT ( 'NONE',  ( 149.5152310637604955, -1.999999999999976685, -4.391296821672111328 ) ) ;
#12700 = CARTESIAN_POINT ( 'NONE',  ( 31.01114313885700824, -11.37490951371675507, -12.31627997798639917 ) ) ;
#12701 = LINE ( 'NONE', #19714, #15543 ) ;
#12702 = PLANE ( 'NONE',  #11509 ) ;
#12703 = VECTOR ( 'NONE', #10650, 1000.000000000000000 ) ;
#12704 = CARTESIAN_POINT ( 'NONE',  ( 22.96196402503608169, -2.069733343145511828, -19.51364111617685992 ) ) ;
#12705 = CARTESIAN_POINT ( 'NONE',  ( 18.87764716858279002, 3.471780965079254599, -19.68009874701989048 ) ) ;
#12706 = EDGE_LOOP ( 'NONE', ( #13112, #12851, #29450, #7108 ) ) ;
#12707 = EDGE_LOOP ( 'NONE', ( #11514, #23948, #23349, #23767, #249, #20794, #8116, #24455 ) ) ;
#12708 = FACE_OUTER_BOUND ( 'NONE', #3115, .T. ) ;
#12709 = CARTESIAN_POINT ( 'NONE',  ( 174.5152310637604103, -4.999999999999970690, -2.627941064794695691 ) ) ;
#12710 = VECTOR ( 'NONE', #9254, 1000.000000000000000 ) ;
#12711 = LINE ( 'NONE', #8135, #1779 ) ;
#12712 = DIRECTION ( 'NONE',  ( 1.000000000000000000, 2.698458740408365879E-16, -1.110223024625156540E-16 ) ) ;
#12713 = VECTOR ( 'NONE', #3754, 1000.000000000000000 ) ;
#12714 = DIRECTION ( 'NONE',  ( -0.9510565162951536422, -2.566386769018988816E-16, -0.3090169943749472292 ) ) ;
#12715 = EDGE_LOOP ( 'NONE', ( #11284, #8734, #11249, #6547 ) ) ;
#12716 = CARTESIAN_POINT ( 'NONE',  ( 10.07879545831710999, 15.66271422494645904, -16.43741374977755143 ) ) ;
#12717 = CARTESIAN_POINT ( 'NONE',  ( 25.72483820513325270, -9.972596264566449875, -15.12420980763781664 ) ) ;
#12718 = CARTESIAN_POINT ( 'NONE',  ( 24.59975295023496855, -6.462932407320696626, -12.83695652901824147 ) ) ;
#12719 = EDGE_CURVE ( 'NONE', #3985, #15063, #21835, .T. ) ;
#12720 = ORIENTED_EDGE ( 'NONE', *, *, #26320, .F. ) ;
#12721 = DIRECTION ( 'NONE',  ( 0.000000000000000000, 0.000000000000000000, -1.000000000000000000 ) ) ;
#12722 = PLANE ( 'NONE',  #7250 ) ;
#12723 = LINE ( 'NONE', #10585, #15050 ) ;
#12724 = CARTESIAN_POINT ( 'NONE',  ( 130.7287565553229456, -4.999999999999982236, -22.10610323145026257 ) ) ;
#12725 = EDGE_CURVE ( 'NONE', #6718, #26068, #5595, .T. ) ;
#12726 = CYLINDRICAL_SURFACE ( 'NONE', #22002, 3.000000000000002665 ) ;
#12727 = DIRECTION ( 'NONE',  ( 0.000000000000000000, 0.000000000000000000, 1.000000000000000000 ) ) ;
#12728 = ADVANCED_FACE ( 'NONE', ( #3322 ), #12601, .T. ) ;
#12729 = CARTESIAN_POINT ( 'NONE',  ( 20.23291344124205793, 5.521974472852556381, -14.51730806008046137 ) ) ;
#12730 = ORIENTED_EDGE ( 'NONE', *, *, #19233, .T. ) ;
#12731 = DIRECTION ( 'NONE',  ( 0.000000000000000000, 2.775557561562890735E-17, -1.000000000000000000 ) ) ;
#12732 = CARTESIAN_POINT ( 'NONE',  ( 11.23952829215726901, 14.25220214615140257, -15.73968358775164056 ) ) ;
#12733 = CARTESIAN_POINT ( 'NONE',  ( 32.52799721746220740, -11.03300674309804386, -18.03857687357939099 ) ) ;
#12734 = LINE ( 'NONE', #700, #21500 ) ;
#12735 = ORIENTED_EDGE ( 'NONE', *, *, #19274, .T. ) ;
#12736 = CARTESIAN_POINT ( 'NONE',  ( 20.22088415693689356, -1.238650738454883493, -19.72259765018230482 ) ) ;
#12737 = FACE_OUTER_BOUND ( 'NONE', #21414, .T. ) ;
#12738 = CARTESIAN_POINT ( 'NONE',  ( 20.08305308227469510, 0.3843232119764288246, -14.09874237319206358 ) ) ;
#12739 = ORIENTED_EDGE ( 'NONE', *, *, #23377, .T. ) ;
#12741 = VECTOR ( 'NONE', #2548, 1000.000000000000000 ) ;
#12740 = CARTESIAN_POINT ( 'NONE',  ( 133.7287565553229456, -1.999999999999980904, 0.5000000000000029976 ) ) ;
#12742 = ADVANCED_FACE ( 'NONE', ( #13354 ), #18910, .T. ) ;
#12743 = CARTESIAN_POINT ( 'NONE',  ( 24.25137658470242386, -8.936440734373054084, -19.04774169986686161 ) ) ;
#12744 = VECTOR ( 'NONE', #21740, 1000.000000000000000 ) ;
#12745 = CARTESIAN_POINT ( 'NONE',  ( 22.15378238435969394, -4.028439702987021143, -12.64872919198682943 ) ) ;
#12746 = CARTESIAN_POINT ( 'NONE',  ( 25.79824969357368047, -12.24460132778619226, -15.92960863319586906 ) ) ;
#12747 = PRODUCT_DEFINITION_SHAPE ( 'NONE', 'NONE',  #30267 ) ;
#12748 = ORIENTED_EDGE ( 'NONE', *, *, #14912, .T. ) ;
#12749 = DIRECTION ( 'NONE',  ( -2.698458740408365879E-16, 1.000000000000000000, 0.000000000000000000 ) ) ;
#12750 = LINE ( 'NONE', #24365, #11206 ) ;
#12751 = CARTESIAN_POINT ( 'NONE',  ( 20.00000000000017053, 41.64101615137744972, 12.00000000000000178 ) ) ;
#12752 = CARTESIAN_POINT ( 'NONE',  ( 134.5152310637605524, -1.999999999999980460, -30.37205893520530964 ) ) ;
#12753 = LINE ( 'NONE', #27139, #6341 ) ;
#12754 = CARTESIAN_POINT ( 'NONE',  ( 34.43765690731135720, -12.70119407716533111, -19.95187818093482335 ) ) ;
#12755 = CARTESIAN_POINT ( 'NONE',  ( 9.879812780108833792, 16.57527415160161510, -16.52987074417163527 ) ) ;
#12756 = EDGE_CURVE ( 'NONE', #16032, #29409, #16089, .T. ) ;
#12757 = LINE ( 'NONE', #9866, #22488 ) ;
#12758 = DIRECTION ( 'NONE',  ( -0.5877852522924731371, 0.000000000000000000, 0.8090169943749474513 ) ) ;
#12759 = EDGE_CURVE ( 'NONE', #26933, #24650, #4206, .T. ) ;
#12760 = EDGE_CURVE ( 'NONE', #11338, #20741, #3909, .T. ) ;
#12761 = CARTESIAN_POINT ( 'NONE',  ( 17.47275436513300662, 10.49281628697410262, -12.44556591811621082 ) ) ;
#12762 = DIRECTION ( 'NONE',  ( 0.000000000000000000, -2.775557561562890735E-17, 1.000000000000000000 ) ) ;
#12763 = EDGE_CURVE ( 'NONE', #22297, #15701, #23120, .T. ) ;
#12764 = ORIENTED_EDGE ( 'NONE', *, *, #9412, .F. ) ;
#12765 = CARTESIAN_POINT ( 'NONE',  ( -16.00000000000017053, 34.64101615137744972, 0.000000000000000000 ) ) ;
#12766 = ORIENTED_EDGE ( 'NONE', *, *, #17070, .T. ) ;
#12767 = CARTESIAN_POINT ( 'NONE',  ( 24.55500000000002103, 0.000000000000000000, 2.500000000000001332 ) ) ;
#12768 = CARTESIAN_POINT ( 'NONE',  ( 123.8989781914840336, -4.999999999999984013, -90.01787683252187833 ) ) ;
#12769 = VECTOR ( 'NONE', #25371, 1000.000000000000000 ) ;
#12770 = DIRECTION ( 'NONE',  ( 0.000000000000000000, 0.000000000000000000, 1.000000000000000000 ) ) ;
#12771 = VERTEX_POINT ( 'NONE', #25414 ) ;
#12772 = B_SPLINE_CURVE_WITH_KNOTS ( 'NONE', 3,
 ( #1604, #4029, #22952, #9029, #22796, #25236, #1904, #2052, #11331, #20338, #4322, #6767, #27107, #6169, #24793, #4173, #24947, #6613, #20191, #27416, #13178, #29572, #6320, #25084, #8591, #22504, #18053, #15616, #13621, #20637, #17889, #13324, #18200, #27270, #6467, #22648, #18353, #1747, #27709, #11036, #29728, #16059, #20493, #29879, #27561, #3732, #13029, #22346, #10743, #20052, #29424, #4478, #358, #2802, #9642, #4923, #23097, #21244, #25530, #204, #4769, #23240, #14362, #18961, #2511, #7221, #28315, #54, #507, #23697, #2200, #9793, #28009, #21402, #16215, #14065, #11777, #13913, #7376, #25993, #16671, #6922, #5070, #12083, #18663, #2356, #13768, #11628, #25844, #20940, #23394, #21097, #9484, #19110, #18807, #14216, #7068, #4622, #20788, #30173, #28166, #28464, #11469, #7513, #25387, #9181, #16515, #18507, #27865, #9335, #23544, #2648, #16362, #25684, #11924, #10542, #21694, #26595, #23859, #10392, #21550, #17122, #24296, #8102, #15116, #2957, #9939, #26447, #24151, #5381, #14809, #19701, #29065, #5683, #3255, #12835, #10088, #14666, #26146, #24011, #17266, #654, #5829, #14963, #19251, #16970, #3106, #24448, #28607, #21846, #7664, #17412, #26296, #3541, #12236, #1113, #22148, #1255, #956, #22007, #14515, #12382, #12529, #10240, #26759, #798, #19401, #19850, #29215, #16814, #5223, #28771, #7815, #5528, #3392, #19555, #28922, #7956, #12685, #8552, #15575, #17711, #1408, #22919 ),
 .UNSPECIFIED., .F., .F.,
 ( 4, 2, 2, 2, 2, 2, 2, 2, 2, 2, 2, 2, 2, 2, 2, 2, 2, 2, 2, 2, 2, 2, 2, 2, 2, 2, 2, 2, 2, 2, 2, 2, 2, 2, 2, 2, 2, 2, 2, 2, 2, 2, 2, 2, 2, 2, 2, 2, 2, 2, 2, 2, 2, 2, 2, 2, 2, 2, 2, 2, 2, 2, 2, 2, 2, 2, 2, 2, 2, 2, 2, 2, 2, 2, 2, 2, 2, 2, 2, 2, 2, 2, 2, 2, 2, 2, 2, 2, 2, 2, 2, 4 ),
 ( 0.000000000000000000, 0.2329478137359916601, 0.2349098735327963261, 0.2358909034311986452, 0.2363814183803998326, 0.2366266758550004123, 0.2367493045923006745, 0.2368106189609508194, 0.2368719333296009921, 0.2369056680493116518, 0.2369394027690223392, 0.2370068722084437141, 0.2371418110872864082, 0.2374116888449718521, 0.2379514443603427676, 0.2390309553910845153, 0.2411899774525680384, 0.2455080215755350015, 0.2541441098214690109, 0.2714162863133369741, 0.2886884628052049373, 0.2973245510511389189, 0.3016425951741059097, 0.3038016172355894051, 0.3048811282663311251, 0.3054208837817020128, 0.3056907615393874567, 0.3058257004182301508, 0.3058931698576515257, 0.3059269045773622131, 0.3059606392970729005, 0.3060023410584322701, 0.3060440428197916396, 0.3061274463425104342, 0.3062942533879479678, 0.3066278674788230352, 0.3072950956605731698, 0.3086295520240734391, 0.3112984647510739777, 0.3166362902050751105, 0.3273119411130773204, 0.3486632429290816848, 0.3913658465610905246, 0.4767710538251080932, 0.5621762610891257728, 0.6048788647211346126, 0.6262301665371389214, 0.6369058174451410759, 0.6422436428991421531, 0.6449125556261426917, 0.6462470119896429610, 0.6469142401713930957, 0.6472478542622682740, 0.6474146613077057522, 0.6474980648304246023, 0.6475397665917840273, 0.6475814683531433413, 0.6476196945210074274, 0.6476579206888716245, 0.6477343730245997966, 0.6478872776960561408, 0.6481930870389688293, 0.6488047057247942062, 0.6500279430964451821, 0.6524744178397469119, 0.6573673673263503714, 0.6671532662995571794, 0.6769391652727643205, 0.6867250642459713506, 0.6965109632191783806, 0.7062968621923852997, 0.7160827611655923297, 0.7209757106521957892, 0.7234221853954975190, 0.7246454227671484949, 0.7252570414529738718, 0.7255628507958865603, 0.7257157554673429045, 0.7257922078030710766, 0.7258304339709352737, 0.7258686601387993598, 0.7259088784260311344, 0.7259490967132626871, 0.7260295332877261254, 0.7261904064366527800, 0.7265121527345063113, 0.7271556453302132628, 0.7284426305216268327, 0.7310166009044544166, 0.7361645416701094735, 0.7464604232014194762, 0.7670521862640397037 ),
 .UNSPECIFIED. ) ;
#12773 = EDGE_LOOP ( 'NONE', ( #13886, #21960, #13814, #21055 ) ) ;
#12774 = VERTEX_POINT ( 'NONE', #13794 ) ;
#12775 = CARTESIAN_POINT ( 'NONE',  ( 13.27290874800832121, 7.583804977141803683, -15.79253525446438999 ) ) ;
#12776 = CARTESIAN_POINT ( 'NONE',  ( 27.89044320811645505, -9.967159925860730851, -19.81290489186636350 ) ) ;
#12777 = CARTESIAN_POINT ( 'NONE',  ( 28.56280713547801398, -4.978584871567802494, -14.74258920993753641 ) ) ;
#12778 = DIRECTION ( 'NONE',  ( 0.5877852522924731371, 1.586114251531760728E-16, 0.8090169943749474513 ) ) ;
#12779 = CARTESIAN_POINT ( 'NONE',  ( 158.6922820468853104, -4.999999999999975131, -0.6060766987539614181 ) ) ;
#12780 = VECTOR ( 'NONE', #6261, 1000.000000000000000 ) ;
#12781 = DIRECTION ( 'NONE',  ( 0.5877852522924731371, 0.000000000000000000, 0.8090169943749474513 ) ) ;
#12782 = ORIENTED_EDGE ( 'NONE', *, *, #9964, .F. ) ;
#12783 = VERTEX_POINT ( 'NONE', #20520 ) ;
#12784 = DIRECTION ( 'NONE',  ( -1.000000000000000000, 0.000000000000000000, -0.000000000000000000 ) ) ;
#12785 = VERTEX_POINT ( 'NONE', #4058 ) ;
#12786 = VERTEX_POINT ( 'NONE', #22980 ) ;
#12787 = EDGE_CURVE ( 'NONE', #2431, #2626, #13502, .T. ) ;
#12788 = CARTESIAN_POINT ( 'NONE',  ( 130.7287565553229456, -4.999999999999983125, 3.500000000000003109 ) ) ;
#12789 = AXIS2_PLACEMENT_3D ( 'NONE', #19200, #12180, #20886 ) ;
#12790 = DIRECTION ( 'NONE',  ( -0.000000000000000000, -0.000000000000000000, 1.000000000000000000 ) ) ;
#12791 = FACE_OUTER_BOUND ( 'NONE', #11183, .T. ) ;
#12792 = CARTESIAN_POINT ( 'NONE',  ( 13.12299649507002464, 8.570581087883812899, -15.91239967140973022 ) ) ;
#12793 = CARTESIAN_POINT ( 'NONE',  ( 35.54787733059053778, -22.18129662410796854, -18.46719521006932396 ) ) ;
#12794 = EDGE_LOOP ( 'NONE', ( #2014, #12135, #23747, #7324, #30145 ) ) ;
#12795 = CARTESIAN_POINT ( 'NONE',  ( 9.128787768473113573, 16.10681393216777835, -17.04800165206417972 ) ) ;
#12796 = EDGE_CURVE ( 'NONE', #20051, #26875, #15491, .T. ) ;
#12797 = VECTOR ( 'NONE', #23722, 1000.000000000000000 ) ;
#12798 = CARTESIAN_POINT ( 'NONE',  ( 27.83100014064079275, -5.545984359997562230, -15.13782040115233052 ) ) ;
#12799 = EDGE_CURVE ( 'NONE', #8506, #29328, #2856, .T. ) ;
#12800 = CARTESIAN_POINT ( 'NONE',  ( 10.35865057885519214, 16.97211863855931924, -17.91295731025335414 ) ) ;
#12801 = FACE_BOUND ( 'NONE', #4744, .T. ) ;
#12802 = EDGE_CURVE ( 'NONE', #2569, #5343, #6646, .T. ) ;
#12803 = EDGE_LOOP ( 'NONE', ( #7357, #1819, #11158, #11164 ) ) ;
#12804 = ORIENTED_EDGE ( 'NONE', *, *, #9204, .F. ) ;
#12805 = CARTESIAN_POINT ( 'NONE',  ( 7.896494747980494111, -5.000000000000015987, 24.30291188725040641 ) ) ;
#12806 = CARTESIAN_POINT ( 'NONE',  ( 12.29195110325218288, 8.516770644378290456, -15.29309475950548958 ) ) ;
#12807 = DIRECTION ( 'NONE',  ( -2.698458740408365879E-16, 1.000000000000000000, 0.000000000000000000 ) ) ;
#12808 = ORIENTED_EDGE ( 'NONE', *, *, #25485, .F. ) ;
#12809 = LINE ( 'NONE', #3515, #5706 ) ;
#12810 = ORIENTED_EDGE ( 'NONE', *, *, #7533, .F. ) ;
#12811 = CARTESIAN_POINT ( 'NONE',  ( 12.02305193244137449, 9.338961869187645704, -16.69339841729684437 ) ) ;
#12812 = VERTEX_POINT ( 'NONE', #11064 ) ;
#12813 = CARTESIAN_POINT ( 'NONE',  ( 21.84805831652669283, 4.237162156985878170, -20.00989837289113282 ) ) ;
#12814 = CARTESIAN_POINT ( 'NONE',  ( 19.73194482477335399, 0.5267938184197646923, -13.16654652480547583 ) ) ;
#12815 = CARTESIAN_POINT ( 'NONE',  ( 13.00000000000000178, 0.000000000000000000, 4.999999999999998224 ) ) ;
#12816 = ORIENTED_EDGE ( 'NONE', *, *, #18728, .F. ) ;
#12817 = CARTESIAN_POINT ( 'NONE',  ( 35.77509030908504428, -18.70957389315904962, -20.35615221346758474 ) ) ;
#12818 = CONTEXT_DEPENDENT_SHAPE_REPRESENTATION ( #20777, #12747 ) ;
#12819 = CARTESIAN_POINT ( 'NONE',  ( 18.21616227284554057, 4.699354889203569918, -13.86658597208997179 ) ) ;
#12820 = VECTOR ( 'NONE', #16737, 1000.000000000000000 ) ;
#12821 = FILL_AREA_STYLE ('',( #3528 ) ) ;
#12822 = FACE_BOUND ( 'NONE', #22972, .T. ) ;
#12823 = CARTESIAN_POINT ( 'NONE',  ( 166.1922820468853388, -9.999999999999998224, -13.59645775552055902 ) ) ;
#12824 = AXIS2_PLACEMENT_3D ( 'NONE', #11113, #9255, #22876 ) ;
#12825 = CARTESIAN_POINT ( 'NONE',  ( 33.75544676243647757, -14.12885555826641593, -19.81592319558764004 ) ) ;
#12826 = CARTESIAN_POINT ( 'NONE',  ( 420.0000000000002274, 34.64101615137744972, 12.00000000000000178 ) ) ;
#12827 = EDGE_LOOP ( 'NONE', ( #5463, #4815, #5348, #16388 ) ) ;
#12828 = LINE ( 'NONE', #26589, #22680 ) ;
#12829 = CARTESIAN_POINT ( 'NONE',  ( 12.27687350794345456, 9.494798321042301481, -15.31070534102384251 ) ) ;
#12830 = EDGE_CURVE ( 'NONE', #7141, #7643, #1632, .T. ) ;
#12831 = LINE ( 'NONE', #21843, #22601 ) ;
#12832 = EDGE_LOOP ( 'NONE', ( #16668, #312, #20582, #17458 ) ) ;
#12833 = DIRECTION ( 'NONE',  ( -0.5877852522924731371, 0.000000000000000000, 0.8090169943749474513 ) ) ;
#12834 = VERTEX_POINT ( 'NONE', #29906 ) ;
#12835 = CARTESIAN_POINT ( 'NONE',  ( 11.77869587587188249, 8.711114196793760200, -15.67004689359726299 ) ) ;
#12836 = EDGE_LOOP ( 'NONE', ( #4751, #23825, #24428, #28171, #24271 ) ) ;
#12837 = VECTOR ( 'NONE', #9208, 1000.000000000000000 ) ;
#12838 = CARTESIAN_POINT ( 'NONE',  ( 10.40934825891211979, 10.23400028951819607, -16.51844484289298265 ) ) ;
#12839 = CARTESIAN_POINT ( 'NONE',  ( 130.7287565553229456, -4.999999999999983125, 3.500000000000003109 ) ) ;
#12840 = DIRECTION ( 'NONE',  ( -2.698458740408365879E-16, 1.000000000000000000, 0.000000000000000000 ) ) ;
#12841 = DIRECTION ( 'NONE',  ( -0.5877852522924731371, 0.000000000000000000, 0.8090169943749474513 ) ) ;
#12842 = ORIENTED_EDGE ( 'NONE', *, *, #12330, .T. ) ;
#12843 = CARTESIAN_POINT ( 'NONE',  ( 12.83173194157631514, 9.543008920787411142, -16.14125448247791184 ) ) ;
#12844 = ORIENTED_EDGE ( 'NONE', *, *, #13348, .F. ) ;
#12845 = CARTESIAN_POINT ( 'NONE',  ( 34.55638066306561029, -12.23714146529668234, -18.94394112255963236 ) ) ;
#12846 = CARTESIAN_POINT ( 'NONE',  ( 21.69765170278760280, -5.035756590920279940, -14.89200278627170881 ) ) ;
#12847 = ORIENTED_EDGE ( 'NONE', *, *, #17279, .F. ) ;
#12848 = ORIENTED_EDGE ( 'NONE', *, *, #7980, .F. ) ;
#12849 = CARTESIAN_POINT ( 'NONE',  ( 154.7287565553229172, -1.999999999999975353, -16.50000000000000000 ) ) ;
#12850 = CARTESIAN_POINT ( 'NONE',  ( 27.15828739042733631, -11.95405637977086677, -19.54710185400437794 ) ) ;
#12851 = ORIENTED_EDGE ( 'NONE', *, *, #4160, .F. ) ;
#12852 = FACE_OUTER_BOUND ( 'NONE', #21719, .T. ) ;
#12853 = VECTOR ( 'NONE', #13550, 1000.000000000000000 ) ;
#12854 = CARTESIAN_POINT ( 'NONE',  ( 19.39950943988042553, -1.649204456521256246, -16.58530004841527727 ) ) ;
#12855 = CARTESIAN_POINT ( 'NONE',  ( 19.55603740332541918, 4.113176889600292263, -19.54140316641015573 ) ) ;
#12856 = VERTEX_POINT ( 'NONE', #29759 ) ;
#12857 = ORIENTED_EDGE ( 'NONE', *, *, #28067, .F. ) ;
#12858 = EDGE_CURVE ( 'NONE', #16768, #22950, #11111, .T. ) ;
#12859 = CARTESIAN_POINT ( 'NONE',  ( 154.5152310637604671, -4.999999999999976019, -4.391296821672111328 ) ) ;
#12860 = VECTOR ( 'NONE', #20890, 1000.000000000000000 ) ;
#12861 = CARTESIAN_POINT ( 'NONE',  ( 3.999999999999980904, -2.309401076758567317, -2.092734410091829034 ) ) ;
#12862 = EDGE_LOOP ( 'NONE', ( #3267, #14773, #7559, #9377 ) ) ;
#12863 = LINE ( 'NONE', #20180, #18863 ) ;
#12864 = LINE ( 'NONE', #15145, #17001 ) ;
#12865 = CARTESIAN_POINT ( 'NONE',  ( 0.2500000000000002220, 0.000000000000000000, 0.000000000000000000 ) ) ;
#12866 = CARTESIAN_POINT ( 'NONE',  ( 11.46877092736959014, 9.288109543210406827, -15.86260999805022820 ) ) ;
#12867 = CARTESIAN_POINT ( 'NONE',  ( 17.69365662292968366, 10.27476822432933545, -17.01437286930526227 ) ) ;
#12868 = CARTESIAN_POINT ( 'NONE',  ( 24.77705064808911217, -2.604154092221317551, -13.46095375842554098 ) ) ;
#12869 = ORIENTED_EDGE ( 'NONE', *, *, #27136, .T. ) ;
#12870 = CYLINDRICAL_SURFACE ( 'NONE', #11984, 2.500000000000002665 ) ;
#12871 = FACE_OUTER_BOUND ( 'NONE', #26568, .T. ) ;
#12872 = CARTESIAN_POINT ( 'NONE',  ( 11.50000000000008171, 17.32050807568872486, -17.99999999999999645 ) ) ;
#12873 = PLANE ( 'NONE',  #9259 ) ;
#12874 = DIRECTION ( 'NONE',  ( -0.5877852522924731371, -1.586114251531760728E-16, -0.8090169943749474513 ) ) ;
#12875 = DIRECTION ( 'NONE',  ( 0.5877852522924731371, 1.586114251531760728E-16, 0.8090169943749474513 ) ) ;
#12876 = CARTESIAN_POINT ( 'NONE',  ( 17.88091890332929523, 4.544920326333207861, -13.91018511019278669 ) ) ;
#12877 = VERTEX_POINT ( 'NONE', #22678 ) ;
#12878 = DIRECTION ( 'NONE',  ( 0.9510565162951536422, 2.566386769018988816E-16, 0.3090169943749472292 ) ) ;
#12879 = CARTESIAN_POINT ( 'NONE',  ( 12.27688791398868950, 9.494734666090453246, -15.31069919958039804 ) ) ;
#12880 = DIRECTION ( 'NONE',  ( 0.000000000000000000, 0.000000000000000000, -1.000000000000000000 ) ) ;
#12881 = LINE ( 'NONE', #1014, #8343 ) ;
#12882 = CARTESIAN_POINT ( 'NONE',  ( 23.36212950203212557, 2.915605996956767587, -15.34809340432955693 ) ) ;
#12883 = AXIS2_PLACEMENT_3D ( 'NONE', #12602, #28384, #1031 ) ;
#12884 = FACE_OUTER_BOUND ( 'NONE', #28690, .T. ) ;
#12885 = CARTESIAN_POINT ( 'NONE',  ( 21.03983889671009422, 4.536326888612346231, -13.89983168792289270 ) ) ;
#12886 = ORIENTED_EDGE ( 'NONE', *, *, #27766, .T. ) ;
#12887 = CARTESIAN_POINT ( 'NONE',  ( 132.0152310637605808, -10.00000000000000711, 1.702185954127501066 ) ) ;
#12888 = SHAPE_REPRESENTATION_RELATIONSHIP ( 'NONE' , 'NONE' ,  #17708, #28104 ) ;
#12889 = CARTESIAN_POINT ( 'NONE',  ( 25.50153931649120764, -9.195696458170099064, -12.32940773450113170 ) ) ;
#12890 = CARTESIAN_POINT ( 'NONE',  ( 22.17025134254096130, -8.444422103036636429, -16.38876926059057126 ) ) ;
#12891 = EDGE_CURVE ( 'NONE', #23695, #22008, #6498, .T. ) ;
#12892 = EDGE_CURVE ( 'NONE', #9080, #20712, #19387, .T. ) ;
#12893 = CARTESIAN_POINT ( 'NONE',  ( -4.683753385137379155E-14, -9.237604307034027684, -0.7145311798163362926 ) ) ;
#12894 = B_SPLINE_CURVE_WITH_KNOTS ( 'NONE', 3,
 ( #27552, #13614, #6607, #4617, #22944, #18345 ),
 .UNSPECIFIED., .F., .F.,
 ( 4, 2, 4 ),
 ( 0.01291313371729459203, 0.01525081363757311605, 0.01758849355785164006 ),
 .UNSPECIFIED. ) ;
#12895 = EDGE_CURVE ( 'NONE', #3997, #6165, #20219, .T. ) ;
#12896 = EDGE_CURVE ( 'NONE', #983, #2523, #17922, .T. ) ;
#12897 = CARTESIAN_POINT ( 'NONE',  ( 162.2287565553228887, -10.00000000000000000, -3.509618943233403510 ) ) ;
#12898 = ORIENTED_EDGE ( 'NONE', *, *, #16900, .T. ) ;
#12899 = DIRECTION ( 'NONE',  ( 1.000000000000000000, 2.698458740408365879E-16, -1.110223024625156540E-16 ) ) ;
#12900 = LINE ( 'NONE', #7881, #23785 ) ;
#12901 = LINE ( 'NONE', #1633, #24096 ) ;
#12902 = VECTOR ( 'NONE', #25833, 1000.000000000000000 ) ;
#12903 = FACE_OUTER_BOUND ( 'NONE', #16260, .T. ) ;
#12904 = CARTESIAN_POINT ( 'NONE',  ( 27.25745087693901425, -5.581270904725432302, -18.17424208600867175 ) ) ;
#12905 = CARTESIAN_POINT ( 'NONE',  ( 147.0152310637604955, -1.999999999999977573, -0.06116980274991495881 ) ) ;
#12906 = CARTESIAN_POINT ( 'NONE',  ( 36.53271160917758209, -22.11316507130252873, -18.90714217169671230 ) ) ;
#12907 = CARTESIAN_POINT ( 'NONE',  ( 157.2287565553229740, -1.999999999999973577, -20.83012701892220520 ) ) ;
#12908 = CARTESIAN_POINT ( 'NONE',  ( 9.915538251416846194, 16.41143258624473233, -16.50493629029764264 ) ) ;
#12909 = CARTESIAN_POINT ( 'NONE',  ( 162.2287565553229740, -9.999999999999998224, -29.49038105676660493 ) ) ;
#12910 = CARTESIAN_POINT ( 'NONE',  ( 0.000000000000000000, 0.000000000000000000, -4.449444346342715129 ) ) ;
#12911 = CARTESIAN_POINT ( 'NONE',  ( 9.661883061612440926, 16.25482663361732705, -17.92279151347708677 ) ) ;
#12912 = DIRECTION ( 'NONE',  ( 0.000000000000000000, -1.000000000000000000, 0.000000000000000000 ) ) ;
#12913 = LINE ( 'NONE', #5914, #17324 ) ;
#12914 = CARTESIAN_POINT ( 'NONE',  ( 11.55687758731922798, 9.016417257711555777, -15.81607864292198329 ) ) ;
#12915 = VECTOR ( 'NONE', #12004, 1000.000000000000000 ) ;
#12916 = ORIENTED_EDGE ( 'NONE', *, *, #9628, .T. ) ;
#12917 = CARTESIAN_POINT ( 'NONE',  ( 19.74162731500053525, -5.000000000000012434, -60.75848138442648860 ) ) ;
#12918 = DIRECTION ( 'NONE',  ( -2.698458740408365879E-16, 1.000000000000000000, 0.000000000000000000 ) ) ;
#12919 = LINE ( 'NONE', #10175, #15124 ) ;
#12920 = ORIENTED_EDGE ( 'NONE', *, *, #24742, .T. ) ;
#12921 = ORIENTED_EDGE ( 'NONE', *, *, #22283, .F. ) ;
#12922 = CARTESIAN_POINT ( 'NONE',  ( 8.944584683310379702, 16.95159276115599667, -17.91664992932185996 ) ) ;
#12923 = CARTESIAN_POINT ( 'NONE',  ( 30.38377115645388571, -7.011354780429720712, -16.65419678813778503 ) ) ;
#12924 = CARTESIAN_POINT ( 'NONE',  ( 25.05301747714807448, -9.477991407908255894, -18.78921932654604632 ) ) ;
#12925 = DIRECTION ( 'NONE',  ( 0.9510565162951536422, 0.000000000000000000, -0.3090169943749475623 ) ) ;
#12926 = PLANE ( 'NONE',  #17951 ) ;
#12927 = VECTOR ( 'NONE', #25496, 1000.000000000000000 ) ;
#12928 = CARTESIAN_POINT ( 'NONE',  ( 130.7287565553229456, -9.999999999999982236, 3.500000000000003109 ) ) ;
#12929 = EDGE_CURVE ( 'NONE', #2363, #10720, #6800, .T. ) ;
#12930 = EDGE_CURVE ( 'NONE', #966, #18633, #27739, .T. ) ;
#12931 = EDGE_CURVE ( 'NONE', #2910, #23077, #27133, .T. ) ;
#12932 = VERTEX_POINT ( 'NONE', #18952 ) ;
#12933 = EDGE_CURVE ( 'NONE', #24767, #11084, #944, .T. ) ;
#12934 = DIRECTION ( 'NONE',  ( -0.8090169943749474513, -2.183098979609982436E-16, -0.5877852522924731371 ) ) ;
#12935 = ORIENTED_EDGE ( 'NONE', *, *, #3148, .T. ) ;
#12936 = AXIS2_PLACEMENT_3D ( 'NONE', #9982, #4809, #26340 ) ;
#12938 = ORIENTED_EDGE ( 'NONE', *, *, #22704, .T. ) ;
#12937 = CARTESIAN_POINT ( 'NONE',  ( -24.99999999999999289, 60.00000000000000711, -30.00000000000000711 ) ) ;
#12939 = DIRECTION ( 'NONE',  ( -2.698458740408365879E-16, 1.000000000000000000, 0.000000000000000000 ) ) ;
#12940 = DIRECTION ( 'NONE',  ( 0.000000000000000000, 0.000000000000000000, 1.000000000000000000 ) ) ;
#12941 = VECTOR ( 'NONE', #23168, 1000.000000000000000 ) ;
#12942 = CARTESIAN_POINT ( 'NONE',  ( 13.09018272752966716, 8.557097568986355540, -15.93847522207377310 ) ) ;
#12943 = CARTESIAN_POINT ( 'NONE',  ( 33.19002920664139111, -11.78337016499817658, -17.90800870513906773 ) ) ;
#12944 = EDGE_LOOP ( 'NONE', ( #15621, #15032, #1978, #3904, #14079 ) ) ;
#12945 = VECTOR ( 'NONE', #17051, 1000.000000000000000 ) ;
#12946 = CARTESIAN_POINT ( 'NONE',  ( 8.977559110355956662, 16.80036783546273327, -17.41076197725142194 ) ) ;
#12947 = ORIENTED_EDGE ( 'NONE', *, *, #26743, .F. ) ;
#12948 = CARTESIAN_POINT ( 'NONE',  ( 25.55230692589818631, -0.5649882819070038975, -17.32853901032857280 ) ) ;
#12949 = CARTESIAN_POINT ( 'NONE',  ( 12.86818510107347890, 9.516005823298000266, -16.11548879760486130 ) ) ;
#12950 = FACE_BOUND ( 'NONE', #1900, .T. ) ;
#12951 = ORIENTED_EDGE ( 'NONE', *, *, #22881, .T. ) ;
#12952 = ORIENTED_EDGE ( 'NONE', *, *, #2530, .T. ) ;
#12953 = LINE ( 'NONE', #6249, #27260 ) ;
#12954 = CARTESIAN_POINT ( 'NONE',  ( 11.55687758731922798, 9.016417257711555777, -15.81607864292198329 ) ) ;
#12955 = CARTESIAN_POINT ( 'NONE',  ( 137.0152310637605808, -10.00000000000000533, -17.38167787843870826 ) ) ;
#12956 = ORIENTED_EDGE ( 'NONE', *, *, #12216, .F. ) ;
#12957 = FACE_OUTER_BOUND ( 'NONE', #7639, .T. ) ;
#12958 = ORIENTED_EDGE ( 'NONE', *, *, #19776, .F. ) ;
#12959 = CARTESIAN_POINT ( 'NONE',  ( 13.17827647522021906, 8.595009676161804890, -15.86834059905992511 ) ) ;
#12960 = ADVANCED_FACE ( 'NONE', ( #9634 ), #2947, .T. ) ;
#12961 = ORIENTED_EDGE ( 'NONE', *, *, #11114, .F. ) ;
#12962 = CARTESIAN_POINT ( 'NONE',  ( 19.20998527735078198, 1.665648160765265784, -20.80323043525838855 ) ) ;
#12963 = CARTESIAN_POINT ( 'NONE',  ( 18.86526831082781541, 1.353360947173176232, -20.65364330072180366 ) ) ;
#12964 = AXIS2_PLACEMENT_3D ( 'NONE', #19301, #699, #7266 ) ;
#12965 = LINE ( 'NONE', #21670, #16957 ) ;
#12966 = VERTEX_POINT ( 'NONE', #12226 ) ;
#12967 = CARTESIAN_POINT ( 'NONE',  ( 36.54859590101256828, -22.18452478037840336, -18.26685560724362034 ) ) ;
#12968 = EDGE_LOOP ( 'NONE', ( #11258, #7780, #19604, #10021 ) ) ;
#12969 = VECTOR ( 'NONE', #7560, 1000.000000000000000 ) ;
#12970 = CARTESIAN_POINT ( 'NONE',  ( 17.32695330507268494, 5.471673316493076200, -20.08600194542987794 ) ) ;
#12971 = ADVANCED_FACE ( 'NONE', ( #21839 ), #5520, .T. ) ;
#12972 = ADVANCED_FACE ( 'NONE', ( #14656 ), #10231, .T. ) ;
#12973 = AXIS2_PLACEMENT_3D ( 'NONE', #28505, #5265, #14553 ) ;
#12974 = EDGE_CURVE ( 'NONE', #9725, #9311, #1393, .T. ) ;
#12975 = LINE ( 'NONE', #10979, #16416 ) ;
#12976 = EDGE_CURVE ( 'NONE', #9008, #14061, #7947, .T. ) ;
#12977 = DIRECTION ( 'NONE',  ( 1.000000000000000000, 2.698458740408365879E-16, 0.000000000000000000 ) ) ;
#12978 = VERTEX_POINT ( 'NONE', #28914 ) ;
#12979 = DIRECTION ( 'NONE',  ( -2.698458740408365879E-16, 1.000000000000000000, 0.000000000000000000 ) ) ;
#12980 = CARTESIAN_POINT ( 'NONE',  ( 32.68951927270060764, -11.07419627511998605, -18.48540492261787449 ) ) ;
#12981 = EDGE_LOOP ( 'NONE', ( #12804, #23606, #15886, #22099, #16872, #21071 ) ) ;
#12982 = ORIENTED_EDGE ( 'NONE', *, *, #19136, .T. ) ;
#12983 = CARTESIAN_POINT ( 'NONE',  ( 175.7287565553229456, -4.999999999999970690, -2.233642730705308832 ) ) ;
#12984 = AXIS2_PLACEMENT_3D ( 'NONE', #3560, #22324, #15282 ) ;
#12985 = CARTESIAN_POINT ( 'NONE',  ( 12.24516416863347956, 9.516115402270077794, -15.33328367062981279 ) ) ;
#12986 = CARTESIAN_POINT ( 'NONE',  ( -20.00000000000017053, 34.64101615137744972, 4.999999999999998224 ) ) ;
#12987 = EDGE_LOOP ( 'NONE', ( #28931, #18381, #3999, #21879 ) ) ;
#12988 = VECTOR ( 'NONE', #25243, 1000.000000000000000 ) ;
#12989 = DIRECTION ( 'NONE',  ( 0.000000000000000000, 0.000000000000000000, 1.000000000000000000 ) ) ;
#12990 = ORIENTED_EDGE ( 'NONE', *, *, #22628, .F. ) ;
#12991 = APPLICATION_CONTEXT ( 'automotive_design' ) ;
#12992 = AXIS2_PLACEMENT_3D ( 'NONE', #15561, #29367, #10686 ) ;
#12993 = CARTESIAN_POINT ( 'NONE',  ( 12.22241433628510165, 7.513235304754858568, -15.34201686955167609 ) ) ;
#12994 = DIRECTION ( 'NONE',  ( 0.9510565162951536422, 0.000000000000000000, -0.3090169943749475623 ) ) ;
#12995 = DIRECTION ( 'NONE',  ( -2.698458740408365879E-16, 1.000000000000000000, 0.000000000000000000 ) ) ;
#12996 = ORIENTED_EDGE ( 'NONE', *, *, #11516, .F. ) ;
#12997 = CARTESIAN_POINT ( 'NONE',  ( 174.5152310637603819, -1.999999999999970024, -4.391296821672111328 ) ) ;
#12998 = ORIENTED_EDGE ( 'NONE', *, *, #2348, .T. ) ;
#12999 = CARTESIAN_POINT ( 'NONE',  ( 12.83240265444113071, 9.539962209189782882, -16.14097488725632346 ) ) ;
#13000 = CARTESIAN_POINT ( 'NONE',  ( 36.21506517127201619, -19.68614788779310132, -19.44682451121369482 ) ) ;
#13001 = CARTESIAN_POINT ( 'NONE',  ( 23.36212950203212557, 2.915605996956767587, -15.34809340432955693 ) ) ;
#13002 = CARTESIAN_POINT ( 'NONE',  ( 175.7287565553229456, -9.999999999999971578, 0.5000000000000029976 ) ) ;
#13003 = CARTESIAN_POINT ( 'NONE',  ( 13.78676817088038931, 5.425489125369224119, -17.89072192914586168 ) ) ;
#13004 = DIRECTION ( 'NONE',  ( -0.5877852522924731371, 0.000000000000000000, 0.8090169943749474513 ) ) ;
#13005 = CARTESIAN_POINT ( 'NONE',  ( -13.00000000000000178, -2.870178842070716726E-15, 23.00000000000000000 ) ) ;
#13006 = CARTESIAN_POINT ( 'NONE',  ( 30.50670359208957905, -8.903545733563623443, -17.67935522427464079 ) ) ;
#13007 = CARTESIAN_POINT ( 'NONE',  ( 23.36829581039676640, 3.373260575288004937, -18.04565522708177738 ) ) ;
#13008 = EDGE_CURVE ( 'NONE', #23323, #357, #14350, .T. ) ;
#13009 = EDGE_CURVE ( 'NONE', #17627, #29771, #21541, .T. ) ;
#13010 = VERTEX_POINT ( 'NONE', #5059 ) ;
#13012 = ORIENTED_EDGE ( 'NONE', *, *, #27134, .F. ) ;
#13011 = EDGE_CURVE ( 'NONE', #29392, #2975, #23687, .T. ) ;
#13013 = ORIENTED_EDGE ( 'NONE', *, *, #31, .T. ) ;
#13014 = LINE ( 'NONE', #24325, #10326 ) ;
#13015 = VECTOR ( 'NONE', #22123, 1000.000000000000000 ) ;
#13016 = DIRECTION ( 'NONE',  ( -2.698458740408365879E-16, 1.000000000000000000, 0.000000000000000000 ) ) ;
#13017 = FACE_OUTER_BOUND ( 'NONE', #13755, .T. ) ;
#13018 = PLANE ( 'NONE',  #9087 ) ;
#13019 = FACE_OUTER_BOUND ( 'NONE', #7540, .T. ) ;
#13020 = CARTESIAN_POINT ( 'NONE',  ( 15.00000000000000000, 0.000000000000000000, 0.000000000000000000 ) ) ;
#13021 = CARTESIAN_POINT ( 'NONE',  ( 13.36280753930113363, 7.618652675320872980, -15.72125653641924892 ) ) ;
#13022 = ORIENTED_EDGE ( 'NONE', *, *, #29829, .F. ) ;
#13023 = CARTESIAN_POINT ( 'NONE',  ( 10.33811693838771717, 18.38618951776012267, -17.92454625180715411 ) ) ;
#13024 = CARTESIAN_POINT ( 'NONE',  ( 29.02390443993225588, -5.138988301204332920, -16.36505798003706857 ) ) ;
#13025 = ORIENTED_EDGE ( 'NONE', *, *, #12300, .T. ) ;
#13026 = DIRECTION ( 'NONE',  ( -0.9510565162951536422, 0.000000000000000000, -0.3090169943749472292 ) ) ;
#13027 = DIRECTION ( 'NONE',  ( -0.9510565162951536422, -2.566386769018988816E-16, -0.3090169943749472292 ) ) ;
#13028 = ORIENTED_EDGE ( 'NONE', *, *, #5468, .F. ) ;
#13029 = CARTESIAN_POINT ( 'NONE',  ( 9.898178882064430084, 16.49104486689975246, -16.51464960819000893 ) ) ;
#13030 = FACE_OUTER_BOUND ( 'NONE', #23860, .T. ) ;
#13031 = LINE ( 'NONE', #21892, #996 ) ;
#13033 = ORIENTED_EDGE ( 'NONE', *, *, #7370, .T. ) ;
#13032 = CARTESIAN_POINT ( 'NONE',  ( 22.09544204423535874, -4.864148257255451746, -14.35781331922719772 ) ) ;
#13034 = ORIENTED_EDGE ( 'NONE', *, *, #8865, .F. ) ;
#13035 = FACE_OUTER_BOUND ( 'NONE', #27560, .T. ) ;
#13036 = CARTESIAN_POINT ( 'NONE',  ( 12.19589625337134997, 9.866176767462979669, -15.34419179356244634 ) ) ;
#13037 = ADVANCED_FACE ( 'NONE', ( #9782 ), #3243, .F. ) ;
#13038 = AXIS2_PLACEMENT_3D ( 'NONE', #18819, #28178, #665 ) ;
#13039 = FACE_OUTER_BOUND ( 'NONE', #7870, .T. ) ;
#13040 = LINE ( 'NONE', #15919, #24938 ) ;
#13041 = CARTESIAN_POINT ( 'NONE',  ( 22.97938783112199701, -3.359759438970757017, -19.62490732200095067 ) ) ;
#13042 = DIRECTION ( 'NONE',  ( 0.9510565162951535312, 2.566386769018988816E-16, -0.3090169943749475623 ) ) ;
#13043 = CARTESIAN_POINT ( 'NONE',  ( 16.82931527361030533, 7.354042003703605168, -13.11858969620360504 ) ) ;
#13044 = VERTEX_POINT ( 'NONE', #14507 ) ;
#13045 = DIRECTION ( 'NONE',  ( 0.000000000000000000, 0.000000000000000000, 1.000000000000000000 ) ) ;
#13046 = CARTESIAN_POINT ( 'NONE',  ( 23.38597214775318278, -9.778565425610747042, -17.35394146810280347 ) ) ;
#13047 = CARTESIAN_POINT ( 'NONE',  ( 23.10480167063333212, 0.6704577443818302562, -13.62402792225823944 ) ) ;
#13048 = CARTESIAN_POINT ( 'NONE',  ( 27.76312469413510442, -10.32446017237915648, -18.80420148706337358 ) ) ;
#13049 = AXIS2_PLACEMENT_3D ( 'NONE', #22121, #7925, #5494 ) ;
#13050 = LINE ( 'NONE', #13350, #3095 ) ;
#13051 = CARTESIAN_POINT ( 'NONE',  ( 152.0152310637604671, -10.00000000000000178, -0.06116980274991495881 ) ) ;
#13052 = AXIS2_PLACEMENT_3D ( 'NONE', #6292, #6905, #11165 ) ;
#13053 = FACE_OUTER_BOUND ( 'NONE', #5514, .T. ) ;
#13054 = CARTESIAN_POINT ( 'NONE',  ( 1.214306433183764966E-14, 4.618802153517016507, -2.450000000000000178 ) ) ;
#13055 = DIRECTION ( 'NONE',  ( 8.163404592832029035E-16, 0.000000000000000000, 1.000000000000000000 ) ) ;
#13056 = CARTESIAN_POINT ( 'NONE',  ( 24.53726495287250486, -4.893489461768670168, -18.28393818840952534 ) ) ;
#13057 = CARTESIAN_POINT ( 'NONE',  ( 17.27944038698359464, 10.59897317215052226, -14.78577975581568360 ) ) ;
#13058 = CARTESIAN_POINT ( 'NONE',  ( 34.03885009341546208, -11.93819216554969742, -20.85700406890413916 ) ) ;
#13059 = AXIS2_PLACEMENT_3D ( 'NONE', #3834, #10983, #13285 ) ;
#13060 = DIRECTION ( 'NONE',  ( 0.3090169943749472292, 8.338696094057992503E-17, -0.9510565162951536422 ) ) ;
#13061 = CARTESIAN_POINT ( 'NONE',  ( 9.914377700407460026, 16.41675502110963336, -16.50544604630902867 ) ) ;
#13062 = DIRECTION ( 'NONE',  ( -2.698458740408365879E-16, 1.000000000000000000, 0.000000000000000000 ) ) ;
#13063 = DIRECTION ( 'NONE',  ( -0.5877852522924731371, -1.586114251531760235E-16, 0.8090169943749474513 ) ) ;
#13064 = CARTESIAN_POINT ( 'NONE',  ( 9.661883795922106444, 16.25482326597959926, -17.91529654610192424 ) ) ;
#13065 = LINE ( 'NONE', #15801, #13163 ) ;
#13066 = VERTEX_POINT ( 'NONE', #12519 ) ;
#13067 = DIRECTION ( 'NONE',  ( -0.5877852522924731371, -1.586114251531760235E-16, 0.8090169943749474513 ) ) ;
#13068 = CARTESIAN_POINT ( 'NONE',  ( 11.47511325496290624, 9.259230714725578792, -15.85997136665693041 ) ) ;
#13069 = EDGE_CURVE ( 'NONE', #6853, #7751, #26286, .T. ) ;
#13070 = VERTEX_POINT ( 'NONE', #26135 ) ;
#13071 = PLANE ( 'NONE',  #30069 ) ;
#13072 = PLANE ( 'NONE',  #28375 ) ;
#13073 = EDGE_CURVE ( 'NONE', #3516, #23103, #10078, .T. ) ;
#13074 = AXIS2_PLACEMENT_3D ( 'NONE', #19097, #16661, #14800 ) ;
#13075 = CARTESIAN_POINT ( 'NONE',  ( 16.77165338796101324, 10.12286561294300569, -15.51291369241808304 ) ) ;
#13076 = ORIENTED_EDGE ( 'NONE', *, *, #23166, .T. ) ;
#13077 = CARTESIAN_POINT ( 'NONE',  ( 8.944584694422324844, 16.95159271019519664, -17.91554756312530117 ) ) ;
#13078 = CARTESIAN_POINT ( 'NONE',  ( 34.69314741404605229, -14.84897758684750890, -21.07142838010442176 ) ) ;
#13079 = VECTOR ( 'NONE', #7305, 1000.000000000000000 ) ;
#13080 = CARTESIAN_POINT ( 'NONE',  ( 25.64452216564459164, -12.66255397501067570, -13.70049860994083701 ) ) ;
#13081 = CARTESIAN_POINT ( 'NONE',  ( 24.59975295023496855, -6.462932407320696626, -12.83695652901824147 ) ) ;
#13082 = FACE_OUTER_BOUND ( 'NONE', #15473, .T. ) ;
#13083 = PLANE ( 'NONE',  #18968 ) ;
#13084 = CARTESIAN_POINT ( 'NONE',  ( 130.7287565553229172, -4.999999999999983125, -36.50000000000000711 ) ) ;
#13085 = VERTEX_POINT ( 'NONE', #7654 ) ;
#13086 = CARTESIAN_POINT ( 'NONE',  ( -1.310841663519413114, 0.000000000000000000, 0.000000000000000000 ) ) ;
#13087 = FILL_AREA_STYLE ('',( #22569 ) ) ;
#13088 = LINE ( 'NONE', #11658, #22455 ) ;
#13089 = CARTESIAN_POINT ( 'NONE',  ( 122.2076721278953642, -4.999999999999984901, -88.78907104945136552 ) ) ;
#13090 = CARTESIAN_POINT ( 'NONE',  ( 12.03309083968702886, 9.293808706017943067, -16.68917936036902105 ) ) ;
#13091 = CARTESIAN_POINT ( 'NONE',  ( 35.54859390953724585, -21.18451583373416014, -17.99055332684694974 ) ) ;
#13092 = AXIS2_PLACEMENT_3D ( 'NONE', #17439, #26792, #5863 ) ;
#13093 = ORIENTED_EDGE ( 'NONE', *, *, #22031, .T. ) ;
#13094 = CARTESIAN_POINT ( 'NONE',  ( 9.631286188771861489, 13.80229212302790920, -16.84020087884530881 ) ) ;
#13095 = VERTEX_POINT ( 'NONE', #28597 ) ;
#13096 = CARTESIAN_POINT ( 'NONE',  ( 27.26129135193747999, -10.77754955263135095, -18.64424489656416739 ) ) ;
#13097 = CARTESIAN_POINT ( 'NONE',  ( 10.35864918915110877, 16.97212501191939538, -17.91664992932186351 ) ) ;
#13098 = FACE_BOUND ( 'NONE', #28343, .T. ) ;
#13099 = AXIS2_PLACEMENT_3D ( 'NONE', #21739, #24337, #28959 ) ;
#13100 = EDGE_CURVE ( 'NONE', #22805, #20403, #26586, .T. ) ;
#13101 = CIRCLE ( 'NONE', #11142, 5.000000000000000888 ) ;
#13102 = ORIENTED_EDGE ( 'NONE', *, *, #11792, .T. ) ;
#13103 = CARTESIAN_POINT ( 'NONE',  ( 130.7287565553229456, -4.999999999999983125, -2.233642730705363455 ) ) ;
#13104 = ADVANCED_FACE ( 'NONE', ( #28761 ), #17111, .F. ) ;
#13105 = CARTESIAN_POINT ( 'NONE',  ( 11.47464782381437587, 9.261287281732329291, -15.86016978468419936 ) ) ;
#13106 = LINE ( 'NONE', #8824, #14502 ) ;
#13107 = EDGE_CURVE ( 'NONE', #9848, #14997, #20813, .T. ) ;
#13108 = ORIENTED_EDGE ( 'NONE', *, *, #29078, .F. ) ;
#13109 = CARTESIAN_POINT ( 'NONE',  ( -8.000000000000003553, -4.618802153517037823, -0.7145311798163362926 ) ) ;
#13110 = ORIENTED_EDGE ( 'NONE', *, *, #25877, .T. ) ;
#13111 = CARTESIAN_POINT ( 'NONE',  ( 13.12341270237516078, 8.570764515250925086, -15.91206798513452192 ) ) ;
#13112 = ORIENTED_EDGE ( 'NONE', *, *, #24142, .T. ) ;
#13113 = CARTESIAN_POINT ( 'NONE',  ( 14.76280285026742867, 7.190900411307756812, -14.35234371774122408 ) ) ;
#13114 = CARTESIAN_POINT ( 'NONE',  ( 18.01687101988986583, 8.608027666922664523, -14.27462087050975015 ) ) ;
#13115 = DIRECTION ( 'NONE',  ( 0.000000000000000000, 0.000000000000000000, -1.000000000000000000 ) ) ;
#13116 = EDGE_LOOP ( 'NONE', ( #28427, #4180, #22196, #855 ) ) ;
#13117 = CARTESIAN_POINT ( 'NONE',  ( 35.48977118337261771, -17.42778619908077076, -20.26990708652652629 ) ) ;
#13118 = ITEM_DEFINED_TRANSFORMATION ( 'NONE', 'NONE', #6835,  #13190 ) ;
#13119 = ORIENTED_EDGE ( 'NONE', *, *, #27691, .F. ) ;
#13120 = CARTESIAN_POINT ( 'NONE',  ( 19.40121574091639189, 1.432572567346982240, -13.43353846741550406 ) ) ;
#13121 = COLOUR_RGB ( '', 0.66274510, 0.83137255, 0.94901961) ;
#13122 = LINE ( 'NONE', #17549, #10068 ) ;
#13123 = FACE_BOUND ( 'NONE', #28827, .T. ) ;
#13124 = ORIENTED_EDGE ( 'NONE', *, *, #12931, .F. ) ;
#13125 = LINE ( 'NONE', #22600, #17194 ) ;
#13126 = CARTESIAN_POINT ( 'NONE',  ( 32.36240160181304759, -11.00785621467150044, -17.57054915585148436 ) ) ;
#13127 = DIRECTION ( 'NONE',  ( -2.698458740408365879E-16, 1.000000000000000000, 0.000000000000000000 ) ) ;
#13128 = ORIENTED_EDGE ( 'NONE', *, *, #27, .F. ) ;
#13129 = ORIENTED_EDGE ( 'NONE', *, *, #23600, .T. ) ;
#13130 = DIRECTION ( 'NONE',  ( -2.698458740408365879E-16, 1.000000000000000000, 0.000000000000000000 ) ) ;
#13131 = CARTESIAN_POINT ( 'NONE',  ( 11.05541531668977662, 17.68942339022145305, -17.98596209335946128 ) ) ;
#13132 = CARTESIAN_POINT ( 'NONE',  ( 35.53993026725221682, -23.14559467820676275, -18.82474504553469075 ) ) ;
#13133 = CIRCLE ( 'NONE', #9225, 2.500000000000001332 ) ;
#13134 = CARTESIAN_POINT ( 'NONE',  ( 172.7287565553229456, -4.999999999999971578, 3.500000000000003109 ) ) ;
#13135 = ORIENTED_EDGE ( 'NONE', *, *, #14057, .F. ) ;
#13136 = PLANE ( 'NONE',  #4410 ) ;
#13137 = EDGE_CURVE ( 'NONE', #25794, #13010, #14029, .T. ) ;
#13138 = CARTESIAN_POINT ( 'NONE',  ( 10.66819573146529621, 9.046892785011555915, -16.41140230749465800 ) ) ;
#13139 = DIRECTION ( 'NONE',  ( -0.5877852522924731371, -1.586114251531760235E-16, 0.8090169943749474513 ) ) ;
#13140 = LINE ( 'NONE', #8556, #3761 ) ;
#13141 = EDGE_CURVE ( 'NONE', #14190, #12612, #17891, .T. ) ;
#13142 = ADVANCED_FACE ( 'NONE', ( #4175 ), #28127, .T. ) ;
#13143 = AXIS2_PLACEMENT_3D ( 'NONE', #27373, #27220, #17698 ) ;
#13144 = ORIENTED_EDGE ( 'NONE', *, *, #27871, .F. ) ;
#13145 = VECTOR ( 'NONE', #29758, 1000.000000000000000 ) ;
#13146 = CARTESIAN_POINT ( 'NONE',  ( -19.99999999999999289, 60.00000000000000711, -25.00000000000000000 ) ) ;
#13147 = EDGE_CURVE ( 'NONE', #27090, #7113, #22799, .T. ) ;
#13148 = VERTEX_POINT ( 'NONE', #23357 ) ;
#13149 = CARTESIAN_POINT ( 'NONE',  ( 12.86812980024498643, 9.515982172609518841, -16.11553281326163045 ) ) ;
#13150 = CARTESIAN_POINT ( 'NONE',  ( 36.30315773322485740, -20.08190110472122214, -19.47147371593984388 ) ) ;
#13151 = CARTESIAN_POINT ( 'NONE',  ( 18.97268594440662426, -2.511067197207834667, -17.06021009607598415 ) ) ;
#13152 = EDGE_LOOP ( 'NONE', ( #1368, #17944, #29477, #2867 ) ) ;
#13153 = ORIENTED_EDGE ( 'NONE', *, *, #4435, .T. ) ;
#13154 = VERTEX_POINT ( 'NONE', #2473 ) ;
#13155 = CARTESIAN_POINT ( 'NONE',  ( 136.1922820468854241, -1.999999999999980460, -4.936203717676158398 ) ) ;
#13156 = CARTESIAN_POINT ( 'NONE',  ( 161.1922820468853956, -1.999999999999972244, -28.06379628232387802 ) ) ;
#13157 = DIRECTION ( 'NONE',  ( 0.5877852522924731371, 1.586114251531760728E-16, 0.8090169943749474513 ) ) ;
#13158 = CARTESIAN_POINT ( 'NONE',  ( 26.69342817538273138, -7.978421288772274522, -19.59580293194042966 ) ) ;
#13159 = CARTESIAN_POINT ( 'NONE',  ( 25.59095072769168766, -7.385909681514642777, -13.40699837787023618 ) ) ;
#13160 = STYLED_ITEM ( 'NONE', ( #13451 ), #12376 ) ;
#13161 = ORIENTED_EDGE ( 'NONE', *, *, #7705, .T. ) ;
#13162 = DIRECTION ( 'NONE',  ( -2.698458740408365879E-16, 1.000000000000000000, 0.000000000000000000 ) ) ;
#13163 = VECTOR ( 'NONE', #24990, 1000.000000000000000 ) ;
#13165 = LINE ( 'NONE', #18458, #1427 ) ;
#13164 = VECTOR ( 'NONE', #7089, 1000.000000000000000 ) ;
#13166 = CARTESIAN_POINT ( 'NONE',  ( 159.7287565553229740, -9.999999999999998224, -25.16025403784440329 ) ) ;
#13167 = DIRECTION ( 'NONE',  ( -2.698458740408365879E-16, 1.000000000000000000, 0.000000000000000000 ) ) ;
#13168 = FACE_OUTER_BOUND ( 'NONE', #8210, .T. ) ;
#13169 = CARTESIAN_POINT ( 'NONE',  ( 137.2287565553230309, -1.999999999999979572, -3.509618943233403510 ) ) ;
#13170 = CARTESIAN_POINT ( 'NONE',  ( 12.16405474897817207, 7.700086518927777846, -16.63006945039463247 ) ) ;
#13171 = CARTESIAN_POINT ( 'NONE',  ( 12.49742530276927610, 8.569573706352677789, -15.13222638044318735 ) ) ;
#13173 = AXIS2_PLACEMENT_3D ( 'NONE', #7145, #9719, #7450 ) ;
#13172 = LINE ( 'NONE', #13464, #23387 ) ;
#13174 = VERTEX_POINT ( 'NONE', #4031 ) ;
#13175 = PLANE ( 'NONE',  #13938 ) ;
#13176 = DIRECTION ( 'NONE',  ( 0.000000000000000000, -1.000000000000000000, 0.000000000000000000 ) ) ;
#13177 = EDGE_LOOP ( 'NONE', ( #12357, #3246, #19786, #12257, #14683 ) ) ;
#13178 = CARTESIAN_POINT ( 'NONE',  ( 9.641351021852148762, 17.66889017177091503, -17.91406276888456617 ) ) ;
#13179 = EDGE_CURVE ( 'NONE', #6891, #4371, #11592, .T. ) ;
#13180 = DIRECTION ( 'NONE',  ( -0.8090169943749474513, -2.183098979609982436E-16, 0.5877852522924731371 ) ) ;
#13181 = DIRECTION ( 'NONE',  ( 0.5877852522924731371, 1.586114251531760728E-16, 0.8090169943749474513 ) ) ;
#13182 = CARTESIAN_POINT ( 'NONE',  ( 20.00000000000017053, 25.64101615137744616, 12.00000000000000178 ) ) ;
#13183 = EDGE_CURVE ( 'NONE', #30043, #29696, #29729, .T. ) ;
#13185 = ORIENTED_EDGE ( 'NONE', *, *, #9665, .F. ) ;
#13184 = CARTESIAN_POINT ( 'NONE',  ( 23.60870351872479844, -7.222488552757559077, -14.83554404960226947 ) ) ;
#13186 = ORIENTED_EDGE ( 'NONE', *, *, #18612, .T. ) ;
#13187 = DIRECTION ( 'NONE',  ( -0.8090169943749474513, -2.183098979609982436E-16, -0.5877852522924731371 ) ) ;
#13188 = EDGE_CURVE ( 'NONE', #30193, #8651, #22649, .T. ) ;
#13189 = CARTESIAN_POINT ( 'NONE',  ( 16.59405769476016701, 11.43796928512929867, -11.86713876492064124 ) ) ;
#13190 = AXIS2_PLACEMENT_3D ( 'NONE', #5435, #19606, #10446 ) ;
#13191 = LINE ( 'NONE', #17900, #25180 ) ;
#13192 = CARTESIAN_POINT ( 'NONE',  ( 20.00000000000017053, 27.64101615137744972, 14.00000000000000178 ) ) ;
#13193 = CARTESIAN_POINT ( 'NONE',  ( 26.18758235895636233, -4.355437658720127558, -18.53605802859044260 ) ) ;
#13194 = DIRECTION ( 'NONE',  ( -2.698458740408365879E-16, 1.000000000000000000, 0.000000000000000000 ) ) ;
#13195 = CARTESIAN_POINT ( 'NONE',  ( 21.44242187996815119, -3.785596145164559445, -16.19382493935754397 ) ) ;
#13196 = VERTEX_POINT ( 'NONE', #1749 ) ;
#13197 = FACE_OUTER_BOUND ( 'NONE', #14071, .T. ) ;
#13198 = ORIENTED_EDGE ( 'NONE', *, *, #2349, .T. ) ;
#13199 = PRESENTATION_STYLE_ASSIGNMENT (( #27123 ) ) ;
#13200 = CARTESIAN_POINT ( 'NONE',  ( 15.17188473929424930, 6.803351907998973935, -20.50413427079521256 ) ) ;
#13201 = CARTESIAN_POINT ( 'NONE',  ( 25.20506945179333513, 0.8918220058822420304, -17.26233558910082166 ) ) ;
#13202 = ORIENTED_EDGE ( 'NONE', *, *, #6639, .F. ) ;
#13203 = ORIENTED_EDGE ( 'NONE', *, *, #5670, .T. ) ;
#13204 = VECTOR ( 'NONE', #4079, 1000.000000000000000 ) ;
#13205 = CARTESIAN_POINT ( 'NONE',  ( -3.318518101603040726, -7.321656987762888313, -1.321710210895610091E-14 ) ) ;
#13206 = AXIS2_PLACEMENT_3D ( 'NONE', #19704, #29068, #8107 ) ;
#13207 = LINE ( 'NONE', #24513, #7493 ) ;
#13208 = EDGE_CURVE ( 'NONE', #10971, #16231, #16328, .T. ) ;
#13209 = PLANE ( 'NONE',  #20462 ) ;
#13210 = CARTESIAN_POINT ( 'NONE',  ( 0.000000000000000000, 0.000000000000000000, -15.00000000000000355 ) ) ;
#13211 = LINE ( 'NONE', #24671, #712 ) ;
#13212 = DIRECTION ( 'NONE',  ( 0.5877852522924731371, 1.586114251531760728E-16, -0.8090169943749474513 ) ) ;
#13213 = CARTESIAN_POINT ( 'NONE',  ( 23.91915341143258544, -8.806945430038833678, -17.38103690300000181 ) ) ;
#13214 = CARTESIAN_POINT ( 'NONE',  ( 18.23802153489769751, 0.9697156596711644649, -18.35043786425562828 ) ) ;
#13215 = CARTESIAN_POINT ( 'NONE',  ( 32.39840662109286029, -9.588391805189495187, -17.44209920064860597 ) ) ;
#13216 = DIRECTION ( 'NONE',  ( 1.000000000000000000, 0.000000000000000000, 0.000000000000000000 ) ) ;
#13217 = CARTESIAN_POINT ( 'NONE',  ( 11.47338783222600789, 9.266948822715743717, -15.86069975447064806 ) ) ;
#13218 = CARTESIAN_POINT ( 'NONE',  ( 153.6922820468854241, -10.00000000000000000, -23.73366926340167637 ) ) ;
#13219 = DIRECTION ( 'NONE',  ( -0.8090169943749474513, -2.183098979609982436E-16, -0.5877852522924731371 ) ) ;
#13220 = CARTESIAN_POINT ( 'NONE',  ( 13.15105351193492744, 8.582979361647906202, -15.89003778131599098 ) ) ;
#13221 = CARTESIAN_POINT ( 'NONE',  ( -13.00000000000000178, -2.870178842070716726E-15, 23.00000000000000000 ) ) ;
#13222 = VERTEX_POINT ( 'NONE', #9304 ) ;
#13223 = DIRECTION ( 'NONE',  ( 1.110223024625156540E-16, 2.995891024602366092E-32, 1.000000000000000000 ) ) ;
#13224 = ADVANCED_FACE ( 'NONE', ( #7036 ), #20340, .T. ) ;
#13225 = AXIS2_PLACEMENT_3D ( 'NONE', #12909, #14586, #12305 ) ;
#13226 = CARTESIAN_POINT ( 'NONE',  ( 12.77278825050581013, 8.691252192278360766, -14.91275796197543890 ) ) ;
#13227 = VECTOR ( 'NONE', #14854, 1000.000000000000000 ) ;
#13228 = ORIENTED_EDGE ( 'NONE', *, *, #24395, .F. ) ;
#13229 = AXIS2_PLACEMENT_3D ( 'NONE', #21603, #25249, #24960 ) ;
#13230 = LINE ( 'NONE', #10631, #6634 ) ;
#13231 = DIRECTION ( 'NONE',  ( -0.9510565162951536422, -2.566386769018988323E-16, 0.3090169943749475623 ) ) ;
#13232 = DIRECTION ( 'NONE',  ( -0.8090169943749474513, -2.183098979609982436E-16, 0.5877852522924731371 ) ) ;
#13233 = ORIENTED_EDGE ( 'NONE', *, *, #26745, .F. ) ;
#13234 = ORIENTED_EDGE ( 'NONE', *, *, #20027, .F. ) ;
#13235 = CARTESIAN_POINT ( 'NONE',  ( 13.40647825129878612, 7.637826363492710158, -15.68645975549014082 ) ) ;
#13236 = CARTESIAN_POINT ( 'NONE',  ( 32.11502935538656800, -10.34531343835429062, -18.85863636141847621 ) ) ;
#13237 = ORIENTED_EDGE ( 'NONE', *, *, #29578, .T. ) ;
#13238 = CARTESIAN_POINT ( 'NONE',  ( 14.70433163182692482, 6.391443753141328621, -13.74806202935933541 ) ) ;
#13239 = CARTESIAN_POINT ( 'NONE',  ( 27.15223745481332784, -12.21752729395051063, -18.24437427626675046 ) ) ;
#13240 = LINE ( 'NONE', #15358, #8711 ) ;
#13241 = LINE ( 'NONE', #20105, #20891 ) ;
#13242 = CARTESIAN_POINT ( 'NONE',  ( 0.000000000000000000, 0.000000000000000000, -25.03750572909317285 ) ) ;
#13243 = CARTESIAN_POINT ( 'NONE',  ( 17.46640274557904959, 4.060524459741898795, -18.82505950134852313 ) ) ;
#13244 = EDGE_LOOP ( 'NONE', ( #6576, #26668, #4811, #23653, #12553 ) ) ;
#13245 = DIRECTION ( 'NONE',  ( 0.9510565162951535312, 2.566386769018988816E-16, -0.3090169943749475623 ) ) ;
#13246 = EDGE_CURVE ( 'NONE', #220, #7982, #7338, .T. ) ;
#13247 = LINE ( 'NONE', #1818, #9712 ) ;
#13248 = EDGE_CURVE ( 'NONE', #28330, #24722, #27417, .T. ) ;
#13249 = DIRECTION ( 'NONE',  ( -2.698458740408365879E-16, 1.000000000000000000, 0.000000000000000000 ) ) ;
#13250 = FACE_OUTER_BOUND ( 'NONE', #10443, .T. ) ;
#13251 = CARTESIAN_POINT ( 'NONE',  ( 13.05603179413191839, 8.545058472539723837, -15.96546128479914373 ) ) ;
#13252 = CARTESIAN_POINT ( 'NONE',  ( 33.98143228033899987, -14.14408878234146982, -18.84191164812894570 ) ) ;
#13253 = VERTEX_POINT ( 'NONE', #21065 ) ;
#13254 = CARTESIAN_POINT ( 'NONE',  ( 12.74324588813389170, 7.620242904383297322, -14.93629796730785486 ) ) ;
#13255 = PRODUCT_DEFINITION_SHAPE ( 'NONE', 'NONE',  #30270 ) ;
#13256 = VERTEX_POINT ( 'NONE', #10881 ) ;
#13257 = CARTESIAN_POINT ( 'NONE',  ( 28.09718568327657806, -5.958257988085632562, -17.17874431236187149 ) ) ;
#13258 = CARTESIAN_POINT ( 'NONE',  ( 13.30397322184224329, 9.708587077508630259, -15.76815807330931030 ) ) ;
#13259 = FACE_OUTER_BOUND ( 'NONE', #7494, .T. ) ;
#13260 = ORIENTED_EDGE ( 'NONE', *, *, #29249, .F. ) ;
#13261 = ORIENTED_EDGE ( 'NONE', *, *, #13183, .T. ) ;
#13262 = CARTESIAN_POINT ( 'NONE',  ( 176.1922820468852535, -9.999999999999994671, -4.936203717676158398 ) ) ;
#13263 = CARTESIAN_POINT ( 'NONE',  ( 12.50736435846123484, 8.573956625762026107, -15.12430548898761806 ) ) ;
#13265 = LINE ( 'NONE', #29351, #12067 ) ;
#13264 = CIRCLE ( 'NONE', #112, 13.00000000000000178 ) ;
#13266 = ORIENTED_EDGE ( 'NONE', *, *, #12648, .T. ) ;
#13267 = DIRECTION ( 'NONE',  ( 0.3090169943749475623, 8.338696094058001131E-17, 0.9510565162951536422 ) ) ;
#13268 = ORIENTED_EDGE ( 'NONE', *, *, #5551, .F. ) ;
#13269 = CARTESIAN_POINT ( 'NONE',  ( 16.24089679924285790, 9.948436389806387226, -13.42737814189079337 ) ) ;
#13270 = CARTESIAN_POINT ( 'NONE',  ( 21.88956083454650781, 5.816198478639956093, -14.73130718433538178 ) ) ;
#13271 = CARTESIAN_POINT ( 'NONE',  ( 17.13759149762038803, 5.494404601539362609, -21.09448147619161418 ) ) ;
#13272 = CARTESIAN_POINT ( 'NONE',  ( 0.000000000000000000, 0.000000000000000000, 0.000000000000000000 ) ) ;
#13273 = DIRECTION ( 'NONE',  ( 0.5877852522924731371, 0.000000000000000000, 0.8090169943749474513 ) ) ;
#13274 = CARTESIAN_POINT ( 'NONE',  ( 16.94076125623460527, 0.4124075662712927692, -16.40086227390004936 ) ) ;
#13275 = VECTOR ( 'NONE', #25784, 1000.000000000000000 ) ;
#13276 = ORIENTED_EDGE ( 'NONE', *, *, #30084, .F. ) ;
#13277 = FACE_OUTER_BOUND ( 'NONE', #27913, .T. ) ;
#13278 = ADVANCED_FACE ( 'NONE', ( #20192 ), #15617, .T. ) ;
#13279 = DIRECTION ( 'NONE',  ( 0.000000000000000000, 0.000000000000000000, 1.000000000000000000 ) ) ;
#13280 = EDGE_CURVE ( 'NONE', #21455, #4011, #18774, .T. ) ;
#13281 = ADVANCED_FACE ( 'NONE', ( #6470 ), #15761, .T. ) ;
#13282 = VECTOR ( 'NONE', #7904, 1000.000000000000000 ) ;
#13283 = ADVANCED_FACE ( 'NONE', ( #23508 ), #11891, .T. ) ;
#13284 = DIRECTION ( 'NONE',  ( -2.698458740408365879E-16, 1.000000000000000000, 0.000000000000000000 ) ) ;
#13285 = DIRECTION ( 'NONE',  ( -0.9510565162951536422, 0.000000000000000000, -0.3090169943749472292 ) ) ;
#13286 = DIRECTION ( 'NONE',  ( 2.908569913943825061E-16, -1.000000000000000000, -6.826925868028081731E-18 ) ) ;
#13287 = ORIENTED_EDGE ( 'NONE', *, *, #9887, .T. ) ;
#13288 = FACE_OUTER_BOUND ( 'NONE', #24273, .T. ) ;
#13289 = CARTESIAN_POINT ( 'NONE',  ( 11.05541529015696156, 17.68942351190433726, -17.91624098666951070 ) ) ;
#13290 = DIRECTION ( 'NONE',  ( 0.4108911781748707526, -0.9116843969807022496, 0.000000000000000000 ) ) ;
#13291 = EDGE_LOOP ( 'NONE', ( #13093, #25160, #7552, #26672 ) ) ;
#13292 = LINE ( 'NONE', #1709, #10737 ) ;
#13293 = CARTESIAN_POINT ( 'NONE',  ( 12.75629879507850717, 7.625935294889710114, -14.92590036059129943 ) ) ;
#13294 = FACE_BOUND ( 'NONE', #28997, .T. ) ;
#13295 = LINE ( 'NONE', #23070, #5236 ) ;
#13296 = VERTEX_POINT ( 'NONE', #28429 ) ;
#13297 = CARTESIAN_POINT ( 'NONE',  ( 13.86283076467578113, -5.000000000000014211, 42.66540602308926111 ) ) ;
#13298 = EDGE_LOOP ( 'NONE', ( #13565, #25765, #3460, #9990, #27341 ) ) ;
#13299 = CARTESIAN_POINT ( 'NONE',  ( 10.35864918915110877, 16.97212501191939538, -17.91796598306941135 ) ) ;
#13300 = CARTESIAN_POINT ( 'NONE',  ( 35.91774987194125401, -19.35046774019819438, -20.39927477693754554 ) ) ;
#13301 = CARTESIAN_POINT ( 'NONE',  ( 20.22088415693689356, -1.238650738454883493, -19.72259765018230482 ) ) ;
#13302 = CARTESIAN_POINT ( 'NONE',  ( -11.85189716074912880, -5.341585316273318895, 9.999999999999998224 ) ) ;
#13303 = VECTOR ( 'NONE', #3050, 1000.000000000000000 ) ;
#13304 = PLANE ( 'NONE',  #11610 ) ;
#13305 = LINE ( 'NONE', #22779, #23501 ) ;
#13306 = CARTESIAN_POINT ( 'NONE',  ( 29.49448338005720416, -10.05855281841770221, -18.88094824714235642 ) ) ;
#13307 = CARTESIAN_POINT ( 'NONE',  ( 25.48002462322397577, -3.608900787083736184, -12.74538502395823691 ) ) ;
#13308 = ORIENTED_EDGE ( 'NONE', *, *, #3957, .T. ) ;
#13309 = AXIS2_PLACEMENT_3D ( 'NONE', #10537, #28603, #12378 ) ;
#13310 = DIRECTION ( 'NONE',  ( -0.000000000000000000, 1.000000000000000000, 0.000000000000000000 ) ) ;
#13311 = ADVANCED_FACE ( 'NONE', ( #3071 ), #2766, .T. ) ;
#13312 = EDGE_CURVE ( 'NONE', #26603, #29341, #885, .T. ) ;
#13313 = DIRECTION ( 'NONE',  ( 0.000000000000000000, 0.000000000000000000, 1.000000000000000000 ) ) ;
#13314 = CARTESIAN_POINT ( 'NONE',  ( 138.6922820468854525, -10.00000000000000533, -35.24709285013155835 ) ) ;
#13315 = CARTESIAN_POINT ( 'NONE',  ( 175.7287565553229456, -4.999999999999970690, 3.500000000000003109 ) ) ;
#13316 = CARTESIAN_POINT ( 'NONE',  ( 139.7287565553230309, -10.00000000000000533, -16.50000000000000000 ) ) ;
#13317 = VECTOR ( 'NONE', #27582, 999.9999999999998863 ) ;
#13318 = CARTESIAN_POINT ( 'NONE',  ( 11.26737699260669778, 8.919714795263022467, -17.22149591130980184 ) ) ;
#13319 = CARTESIAN_POINT ( 'NONE',  ( 12.50268541164654756, 8.571888915454989544, -15.12803469218787811 ) ) ;
#13320 = CARTESIAN_POINT ( 'NONE',  ( 27.15223745481332784, -12.21752729395051063, -18.24437427626675046 ) ) ;
#13321 = CARTESIAN_POINT ( 'NONE',  ( 159.5152310637604671, -1.999999999999973577, -13.05155085951651195 ) ) ;
#13322 = DIRECTION ( 'NONE',  ( 0.000000000000000000, 0.000000000000000000, 1.000000000000000000 ) ) ;
#13323 = VERTEX_POINT ( 'NONE', #16784 ) ;
#13324 = CARTESIAN_POINT ( 'NONE',  ( 9.641890818133653340, 17.66641459721583374, -17.82828029666912073 ) ) ;
#13325 = CARTESIAN_POINT ( 'NONE',  ( 173.6922820468853672, -9.999999999999994671, -32.39392330124607611 ) ) ;
#13326 = CARTESIAN_POINT ( 'NONE',  ( 144.7287565553229740, -1.999999999999978018, 0.8205080756887930260 ) ) ;
#13327 = LINE ( 'NONE', #6473, #24471 ) ;
#13329 = ORIENTED_EDGE ( 'NONE', *, *, #10769, .F. ) ;
#13328 = CARTESIAN_POINT ( 'NONE',  ( 20.72626264887238534, -1.914771856900582714, -13.62749948506543518 ) ) ;
#13330 = ORIENTED_EDGE ( 'NONE', *, *, #25451, .T. ) ;
#13331 = CARTESIAN_POINT ( 'NONE',  ( 4.000000000000000000, -0.7779732554280925916, -2.416455648918321764 ) ) ;
#13332 = CARTESIAN_POINT ( 'NONE',  ( 14.13034256312282189, 10.34920949090176201, -13.83076321228938887 ) ) ;
#13333 = AXIS2_PLACEMENT_3D ( 'NONE', #20861, #18434, #4404 ) ;
#13334 = CARTESIAN_POINT ( 'NONE',  ( 33.96943610671532809, -15.09019632882451134, -19.88060704079178720 ) ) ;
#13335 = DIRECTION ( 'NONE',  ( -0.9510565162951536422, 0.000000000000000000, -0.3090169943749472292 ) ) ;
#13336 = EDGE_LOOP ( 'NONE', ( #17770, #3888, #28477, #10945 ) ) ;
#13337 = CARTESIAN_POINT ( 'NONE',  ( 25.04992766293576878, -3.547109489677171101, -13.67097983722207033 ) ) ;
#13338 = LINE ( 'NONE', #6784, #23278 ) ;
#13339 = CARTESIAN_POINT ( 'NONE',  ( 22.40033610297568956, 1.362009800809227178, -14.54093962742820700 ) ) ;
#13340 = ORIENTED_EDGE ( 'NONE', *, *, #14608, .T. ) ;
#13341 = DIRECTION ( 'NONE',  ( 0.5877852522924731371, 1.586114251531760728E-16, -0.8090169943749474513 ) ) ;
#13342 = CARTESIAN_POINT ( 'NONE',  ( 14.30110556002302680, 5.443193088601498530, -15.49285935407157666 ) ) ;
#13343 = CARTESIAN_POINT ( 'NONE',  ( 28.63790973356518776, -5.888324979419876648, -13.82040474618100312 ) ) ;
#13344 = VECTOR ( 'NONE', #21644, 1000.000000000000000 ) ;
#13345 = ORIENTED_EDGE ( 'NONE', *, *, #9404, .F. ) ;
#13346 = DIRECTION ( 'NONE',  ( -0.9510565162951536422, -2.566386769018988323E-16, 0.3090169943749475623 ) ) ;
#13347 = EDGE_CURVE ( 'NONE', #7328, #12130, #758, .T. ) ;
#13348 = EDGE_CURVE ( 'NONE', #16735, #12932, #5036, .T. ) ;
#13349 = EDGE_CURVE ( 'NONE', #12321, #7426, #5492, .T. ) ;
#13350 = CARTESIAN_POINT ( 'NONE',  ( 169.5152310637604671, -1.999999999999970912, -11.28819510263909542 ) ) ;
#13352 = ORIENTED_EDGE ( 'NONE', *, *, #26083, .F. ) ;
#13351 = EDGE_CURVE ( 'NONE', #23086, #10981, #26562, .T. ) ;
#13353 = FACE_OUTER_BOUND ( 'NONE', #14445, .T. ) ;
#13354 = FACE_OUTER_BOUND ( 'NONE', #22549, .T. ) ;
#13355 = LINE ( 'NONE', #22679, #15315 ) ;
#13356 = CARTESIAN_POINT ( 'NONE',  ( 9.641350810849047548, 17.66889113945805789, -17.93331994345748370 ) ) ;
#13357 = CARTESIAN_POINT ( 'NONE',  ( 23.38178567734072999, -4.037937620979102249, -14.56836966348588369 ) ) ;
#13358 = CARTESIAN_POINT ( 'NONE',  ( 19.14398323884976350, 7.495936751868839565, -14.71076302495156263 ) ) ;
#13359 = CARTESIAN_POINT ( 'NONE',  ( 34.16709027601721971, -12.48568152589075098, -20.91241392730897886 ) ) ;
#13360 = CARTESIAN_POINT ( 'NONE',  ( 146.1922820468854525, -10.00000000000000178, -30.91696583120935671 ) ) ;
#13361 = CARTESIAN_POINT ( 'NONE',  ( 12.43696608443014284, 8.546664718661613591, -15.18012293544581226 ) ) ;
#13362 = VECTOR ( 'NONE', #5751, 1000.000000000000000 ) ;
#13363 = DIRECTION ( 'NONE',  ( 0.3090169943749475623, 8.338696094058001131E-17, 0.9510565162951536422 ) ) ;
#13364 = CARTESIAN_POINT ( 'NONE',  ( 164.5152310637604671, -4.999999999999973355, -13.05155085951651195 ) ) ;
#13365 = CARTESIAN_POINT ( 'NONE',  ( 9.661883061612440926, 16.25482663361732705, -19.66666666666843000 ) ) ;
#13366 = CARTESIAN_POINT ( 'NONE',  ( -2.645508037661914891, -7.710219529346629130, -4.931901280394557219 ) ) ;
#13367 = ORIENTED_EDGE ( 'NONE', *, *, #2826, .F. ) ;
#13368 = CARTESIAN_POINT ( 'NONE',  ( 0.000000000000000000, 0.000000000000000000, 23.00000000000000000 ) ) ;
#13369 = CARTESIAN_POINT ( 'NONE',  ( 12.50035968906703765, 8.570861208087439564, -15.12988832871674560 ) ) ;
#13370 = ORIENTED_EDGE ( 'NONE', *, *, #20369, .T. ) ;
#13371 = PLANE ( 'NONE',  #4668 ) ;
#13372 = LINE ( 'NONE', #29926, #21961 ) ;
#13373 = FACE_OUTER_BOUND ( 'NONE', #24449, .T. ) ;
#13374 = VECTOR ( 'NONE', #10084, 1000.000000000000114 ) ;
#13375 = ORIENTED_EDGE ( 'NONE', *, *, #13348, .T. ) ;
#13376 = CARTESIAN_POINT ( 'NONE',  ( 13.37966566800644763, 7.625977406171305262, -15.70782985742499527 ) ) ;
#13377 = CARTESIAN_POINT ( 'NONE',  ( 30.54120030308987666, -10.08143909378498293, -14.42492330020037272 ) ) ;
#13378 = CARTESIAN_POINT ( 'NONE',  ( 19.35412429307980986, 8.340480409601783052, -14.20924892776020343 ) ) ;
#13379 = CARTESIAN_POINT ( 'NONE',  ( 18.16542447708646790, 4.701683080007062365, -19.22226433900947029 ) ) ;
#13380 = CARTESIAN_POINT ( 'NONE',  ( 115.6625871560206491, -4.999999999999985789, -84.03378846797562574 ) ) ;
#13381 = CARTESIAN_POINT ( 'NONE',  ( 138.6922820468854525, -1.999999999999979572, -9.266330736598359152 ) ) ;
#13382 = CARTESIAN_POINT ( 'NONE',  ( 22.44149885728860028, -8.037961521189897596, -18.19026436706728234 ) ) ;
#13383 = VECTOR ( 'NONE', #15749, 1000.000000000000000 ) ;
#13384 = EDGE_LOOP ( 'NONE', ( #10372, #3184, #28399, #27269, #11930 ) ) ;
#13385 = EDGE_CURVE ( 'NONE', #9036, #475, #3215, .T. ) ;
#13386 = CARTESIAN_POINT ( 'NONE',  ( 143.6922820468854525, -1.999999999999978018, -26.58683881228715506 ) ) ;
#13387 = ADVANCED_FACE ( 'NONE', ( #470 ), #12492, .T. ) ;
#13389 = VERTEX_POINT ( 'NONE', #23821 ) ;
#13388 = CARTESIAN_POINT ( 'NONE',  ( 139.7287565553230309, -1.999999999999978684, -33.82050807568879947 ) ) ;
#13390 = APPLICATION_CONTEXT ( 'automotive_design' ) ;
#13391 = CARTESIAN_POINT ( 'NONE',  ( -7.999999999999998224, 3.115336682266997670, -0.3193931313915031045 ) ) ;
#13392 = PLANE ( 'NONE',  #676 ) ;
#13393 = CARTESIAN_POINT ( 'NONE',  ( 169.5152310637604387, -1.999999999999970912, -13.05155085951651195 ) ) ;
#13394 = CARTESIAN_POINT ( 'NONE',  ( 33.87301206822314725, -11.11198276574163302, -17.60644260715651299 ) ) ;
#13395 = EDGE_LOOP ( 'NONE', ( #6754, #7544, #19846, #18987, #8186 ) ) ;
#13396 = CARTESIAN_POINT ( 'NONE',  ( 10.66961851098191083, 9.040384230280389843, -16.41081268017797257 ) ) ;
#13397 = ORIENTED_EDGE ( 'NONE', *, *, #23769, .T. ) ;
#13398 = CARTESIAN_POINT ( 'NONE',  ( 25.24878800877705487, -9.370948223588685622, -14.18615728435988288 ) ) ;
#13399 = CARTESIAN_POINT ( 'NONE',  ( 177.2287565553228603, -1.999999999999968914, -12.16987298107780369 ) ) ;
#13400 = CARTESIAN_POINT ( 'NONE',  ( 12.86837137031974621, 9.516086858917468305, -16.11534043535873906 ) ) ;
#13401 = PLANE ( 'NONE',  #3900 ) ;
#13402 = VERTEX_POINT ( 'NONE', #916 ) ;
#13403 = DIRECTION ( 'NONE',  ( -1.110223024625156540E-16, 0.000000000000000000, -1.000000000000000000 ) ) ;
#13404 = EDGE_LOOP ( 'NONE', ( #28964, #27680, #2463, #23073 ) ) ;
#13405 = VECTOR ( 'NONE', #22755, 1000.000000000000000 ) ;
#13406 = DIRECTION ( 'NONE',  ( 0.000000000000000000, -1.000000000000000000, 0.000000000000000000 ) ) ;
#13407 = DIRECTION ( 'NONE',  ( -1.000000000000000000, -4.440892098500622217E-16, 0.000000000000000000 ) ) ;
#13408 = VERTEX_POINT ( 'NONE', #12650 ) ;
#13409 = CARTESIAN_POINT ( 'NONE',  ( -7.999999999999994671, -1.555946510856154985, -0.06708870216335502401 ) ) ;
#13410 = ORIENTED_EDGE ( 'NONE', *, *, #4465, .T. ) ;
#13411 = CARTESIAN_POINT ( 'NONE',  ( 13.11965390131543430, 8.569119222385459977, -15.91506261175275760 ) ) ;
#13412 = EDGE_CURVE ( 'NONE', #26117, #29919, #25759, .T. ) ;
#13413 = CARTESIAN_POINT ( 'NONE',  ( 19.97442599234820193, -2.778558858265142373, -17.76606689721253574 ) ) ;
#13414 = CARTESIAN_POINT ( 'NONE',  ( 15.83402620853355636, 4.298615461832955731, -20.35054180922590916 ) ) ;
#13415 = CARTESIAN_POINT ( 'NONE',  ( 149.5152310637605808, -1.999999999999975797, -19.94844914048349693 ) ) ;
#13416 = LINE ( 'NONE', #24891, #12780 ) ;
#13417 = CARTESIAN_POINT ( 'NONE',  ( 20.52488529563827058, 3.974637744936419637, -19.97762432673833288 ) ) ;
#13418 = VERTEX_POINT ( 'NONE', #28892 ) ;
#13419 = DIRECTION ( 'NONE',  ( 0.7071067811865474617, 6.696944989000215441E-17, 0.7071067811865475727 ) ) ;
#13420 = DIRECTION ( 'NONE',  ( 0.3090169943749472292, 8.338696094057992503E-17, -0.9510565162951536422 ) ) ;
#13421 = VECTOR ( 'NONE', #19628, 1000.000000000000000 ) ;
#13422 = VECTOR ( 'NONE', #21508, 1000.000000000000000 ) ;
#13423 = ORIENTED_EDGE ( 'NONE', *, *, #20443, .F. ) ;
#13424 = CARTESIAN_POINT ( 'NONE',  ( 10.47079889355419446, 16.45779217176459852, -17.33533584583738829 ) ) ;
#13425 = CARTESIAN_POINT ( 'NONE',  ( 33.41663030065195272, -12.60673267154789201, -19.71350710734569134 ) ) ;
#13426 = PLANE ( 'NONE',  #985 ) ;
#13427 = ORIENTED_EDGE ( 'NONE', *, *, #13852, .T. ) ;
#13428 = ORIENTED_EDGE ( 'NONE', *, *, #24738, .T. ) ;
#13429 = CARTESIAN_POINT ( 'NONE',  ( 164.5152310637604955, -1.999999999999971800, -19.94844914048349693 ) ) ;
#13430 = CARTESIAN_POINT ( 'NONE',  ( 15.14574614762244487, 6.587483969391940697, -15.14885142785537830 ) ) ;
#13431 = CARTESIAN_POINT ( 'NONE',  ( 12.24726067228269422, 9.517041913610183812, -15.33161271801373182 ) ) ;
#13432 = CARTESIAN_POINT ( 'NONE',  ( 147.0152310637605240, -4.999999999999977796, -1.632196944975744790E-14 ) ) ;
#13433 = AXIS2_PLACEMENT_3D ( 'NONE', #12910, #3467, #15193 ) ;
#13434 = ORIENTED_EDGE ( 'NONE', *, *, #10502, .F. ) ;
#13435 = LINE ( 'NONE', #8404, #21528 ) ;
#13436 = VECTOR ( 'NONE', #7000, 1000.000000000000000 ) ;
#13437 = CARTESIAN_POINT ( 'NONE',  ( 15.87304960759194650, 9.003283391651189405, -12.44179493704351280 ) ) ;
#13438 = DIRECTION ( 'NONE',  ( -0.5877852522924731371, 0.000000000000000000, 0.8090169943749474513 ) ) ;
#13439 = DIRECTION ( 'NONE',  ( -2.698458740408365879E-16, 1.000000000000000000, 0.000000000000000000 ) ) ;
#13440 = LINE ( 'NONE', #6442, #16412 ) ;
#13441 = VERTEX_POINT ( 'NONE', #9906 ) ;
#13442 = CARTESIAN_POINT ( 'NONE',  ( 10.35865005771744762, 16.97212102856341787, -17.91352035578586310 ) ) ;
#13443 = ADVANCED_FACE ( 'NONE', ( #28573 ), #10150, .F. ) ;
#13444 = EDGE_CURVE ( 'NONE', #25744, #16524, #19663, .T. ) ;
#13446 = CARTESIAN_POINT ( 'NONE',  ( 32.71419323209526908, -10.28616775856061416, -16.33292762241428520 ) ) ;
#13445 = VECTOR ( 'NONE', #20987, 1000.000000000000000 ) ;
#13447 = CARTESIAN_POINT ( 'NONE',  ( 25.55230692589818631, -0.5649882819070038975, -17.32853901032857280 ) ) ;
#13448 = EDGE_CURVE ( 'NONE', #24792, #6067, #14040, .T. ) ;
#13449 = DIRECTION ( 'NONE',  ( 4.440892098500622217E-16, -1.000000000000000000, 0.000000000000000000 ) ) ;
#13450 = CARTESIAN_POINT ( 'NONE',  ( 159.5152310637605524, -9.999999999999998224, -28.60870317832789667 ) ) ;
#13451 = PRESENTATION_STYLE_ASSIGNMENT (( #10860 ) ) ;
#13452 = CARTESIAN_POINT ( 'NONE',  ( 27.87518295380144551, -11.54787579004265652, -18.81772651352153858 ) ) ;
#13453 = CARTESIAN_POINT ( 'NONE',  ( 27.54556670433429488, -3.970347839692917713, -18.20727554117155123 ) ) ;
#13454 = EDGE_LOOP ( 'NONE', ( #5808, #16713, #25157, #10192, #17056, #2059, #17239, #11554 ) ) ;
#13455 = FACE_OUTER_BOUND ( 'NONE', #12832, .T. ) ;
#13456 = AXIS2_PLACEMENT_3D ( 'NONE', #4665, #4816, #13958 ) ;
#13457 = ADVANCED_BREP_SHAPE_REPRESENTATION ( '', ( #21992, #13190 ), #7783 ) ;
#13458 = CARTESIAN_POINT ( 'NONE',  ( 177.2287565553228887, -1.999999999999968470, -20.83012701892220520 ) ) ;
#13459 = CARTESIAN_POINT ( 'NONE',  ( 169.7287565553228603, -1.999999999999971356, 0.8205080756887930260 ) ) ;
#13460 = VECTOR ( 'NONE', #27424, 1000.000000000000000 ) ;
#13461 = CARTESIAN_POINT ( 'NONE',  ( 172.0152310637604387, -9.999999999999996447, -6.958068083716895558 ) ) ;
#13462 = VECTOR ( 'NONE', #24741, 1000.000000000000000 ) ;
#13463 = CARTESIAN_POINT ( 'NONE',  ( 10.33811693838771717, 18.38618951776012267, -17.92015940598198753 ) ) ;
#13464 = CARTESIAN_POINT ( 'NONE',  ( 157.0152310637604671, -1.999999999999974465, -8.721423840594312082 ) ) ;
#13465 = ORIENTED_EDGE ( 'NONE', *, *, #20921, .T. ) ;
#13466 = DIRECTION ( 'NONE',  ( 0.9510565162951535312, 2.566386769018988816E-16, -0.3090169943749475623 ) ) ;
#13467 = ORIENTED_EDGE ( 'NONE', *, *, #20071, .T. ) ;
#13468 = DIRECTION ( 'NONE',  ( -1.000000000000000000, 0.000000000000000000, 0.000000000000000000 ) ) ;
#13469 = DIRECTION ( 'NONE',  ( -0.5877852522924731371, -1.586114251531760235E-16, 0.8090169943749474513 ) ) ;
#13470 = CARTESIAN_POINT ( 'NONE',  ( 18.77375537285786322, 7.252522315878067616, -16.50763127152984566 ) ) ;
#13471 = PLANE ( 'NONE',  #21461 ) ;
#13472 = CARTESIAN_POINT ( 'NONE',  ( 172.0152310637603819, -4.999999999999970690, -0.06116980274991495881 ) ) ;
#13474 = VERTEX_POINT ( 'NONE', #19521 ) ;
#13473 = CARTESIAN_POINT ( 'NONE',  ( 23.22413189157496305, -7.367447486509826504, -15.63851824576001981 ) ) ;
#13475 = ORIENTED_EDGE ( 'NONE', *, *, #3856, .T. ) ;
#13476 = LINE ( 'NONE', #11480, #13460 ) ;
#13477 = CARTESIAN_POINT ( 'NONE',  ( 12.24938746628909492, 9.517981781931423413, -15.32991762565031202 ) ) ;
#13478 = ADVANCED_FACE ( 'NONE', ( #23979 ), #10054, .T. ) ;
#13479 = CARTESIAN_POINT ( 'NONE',  ( 33.48796008207983022, -12.92717959506727965, -19.73506838908087246 ) ) ;
#13480 = DIRECTION ( 'NONE',  ( 0.3090169943749475623, 8.338696094058001131E-17, 0.9510565162951536422 ) ) ;
#13481 = ORIENTED_EDGE ( 'NONE', *, *, #16792, .T. ) ;
#13482 = EDGE_CURVE ( 'NONE', #28074, #11734, #7777, .T. ) ;
#13483 = AXIS2_PLACEMENT_3D ( 'NONE', #6939, #16232, #21710 ) ;
#13484 = CARTESIAN_POINT ( 'NONE',  ( 21.43917814492346707, -4.799604530101110988, -17.97822123721208243 ) ) ;
#13485 = CARTESIAN_POINT ( 'NONE',  ( 8.000000000000014211, 1.572549600175630502, -4.931055444744863792 ) ) ;
#13486 = EDGE_CURVE ( 'NONE', #16252, #18592, #17234, .T. ) ;
#13487 = B_SPLINE_CURVE_WITH_KNOTS ( 'NONE', 3,
 ( #1863, #8843, #16014, #23055, #13582, #13727, #9288, #27962, #13868, #25340, #156, #16313, #4430, #22906, #11140, #7023, #20444, #25630, #11577, #20892, #28113, #29838, #2010, #2154, #11427, #11290, #20734, #14010, #23343, #23191, #30126, #9434, #2458, #9133, #20593, #29976, #16168, #18461, #11732, #8982, #27814, #21050, #18304, #27659, #6880, #2304, #3, #18760, #15714, #25046, #4131, #13424, #309, #23809, #4871, #9592, #26247, #25790, #21350, #12483, #16622, #18913, #5481, #28267, #14313, #21807, #28560, #17077, #7470, #7319, #16464, #14168, #23494, #12329, #14764, #21645, #16917, #2604, #3056, #25941, #12185, #11878, #5022, #26402, #743, #14468, #19204, #10041, #12036, #904, #24103, #21192, #10196, #9742, #3205, #23648, #16773, #2907, #2749, #19354, #7764, #456, #19060, #28715, #19508, #28416, #26097, #5176, #21503, #7614, #605, #9894, #5334, #14618, #7173, #23967, #17670, #1212, #19655, #24256, #3353, #12640, #17812, #14916, #13090, #27185, #3950, #3647, #3800, #26552, #15068, #8364, #22256, #6238, #21957, #15533, #29495, #24406, #26873, #1069, #10349, #24865, #10494, #8055, #29020, #13251, #24555, #12942, #29166, #10951, #1364, #10652, #8206, #22571, #22416, #19966, #3502, #17364, #12792, #1671, #22110, #5938, #28882, #26713, #17518, #7914, #17225, #15222, #29335, #5633, #5785, #19806, #27027, #6082, #15378, #24712, #1522, #10805, #20115, #8513, #18577, #11256, #2124, #4396 ),
 .UNSPECIFIED., .F., .F.,
 ( 4, 2, 2, 2, 2, 2, 2, 2, 2, 2, 2, 2, 2, 2, 2, 2, 2, 2, 2, 2, 2, 2, 2, 2, 2, 2, 2, 2, 2, 2, 2, 2, 2, 2, 2, 2, 2, 2, 2, 2, 2, 2, 2, 2, 2, 2, 2, 2, 2, 2, 2, 2, 2, 2, 2, 2, 2, 2, 2, 2, 2, 2, 2, 2, 2, 2, 2, 2, 2, 2, 2, 2, 2, 2, 2, 2, 2, 2, 2, 2, 2, 2, 2, 2, 2, 2, 2, 2, 2, 2, 2, 4 ),
 ( 0.000000000000000000, 0.2329478137359917711, 0.2349098735327964371, 0.2358909034311987563, 0.2363814183803999158, 0.2366266758550005234, 0.2367493045923007855, 0.2368106189609509304, 0.2368719333296011031, 0.2369056680493117628, 0.2369394027690224502, 0.2370068722084438251, 0.2371418110872865193, 0.2374116888449719631, 0.2379514443603428231, 0.2390309553910846263, 0.2411899774525681217, 0.2455080215755351125, 0.2541441098214691219, 0.2714162863133370851, 0.2886884628052050483, 0.2973245510511390299, 0.3016425951741060207, 0.3038016172355895161, 0.3048811282663312361, 0.3054208837817021238, 0.3056907615393875677, 0.3058257004182302619, 0.3058931698576516367, 0.3059269045773623241, 0.3059606392970730115, 0.3060023410584323811, 0.3060440428197917506, 0.3061274463425105452, 0.3062942533879481344, 0.3066278674788231462, 0.3072950956605732808, 0.3086295520240735502, 0.3112984647510740888, 0.3166362902050752215, 0.3273119411130774314, 0.3486632429290818513, 0.3913658465610906356, 0.4767710538251083152, 0.5621762610891259948, 0.6048788647211348346, 0.6262301665371391435, 0.6369058174451412979, 0.6422436428991423751, 0.6449125556261429137, 0.6462470119896432941, 0.6469142401713934287, 0.6472478542622684961, 0.6474146613077059742, 0.6474980648304248243, 0.6475397665917842493, 0.6475814683531435634, 0.6476196945210076494, 0.6476579206888718465, 0.6477343730246000186, 0.6478872776960563629, 0.6481930870389690513, 0.6488047057247944283, 0.6500279430964454042, 0.6524744178397472449, 0.6573673673263507045, 0.6671532662995575125, 0.6769391652727646536, 0.6867250642459716836, 0.6965109632191786027, 0.7062968621923857437, 0.7160827611655926628, 0.7209757106521960113, 0.7234221853954977410, 0.7246454227671487169, 0.7252570414529740939, 0.7255628507958867823, 0.7257157554673431266, 0.7257922078030714097, 0.7258304339709356068, 0.7258686601387995818, 0.7259088784260314675, 0.7259490967132631312, 0.7260295332877264585, 0.7261904064366531131, 0.7265121527345066443, 0.7271556453302134848, 0.7284426305216270547, 0.7310166009044546387, 0.7361645416701096956, 0.7464604232014198093, 0.7670521862640400368 ),
 .UNSPECIFIED. ) ;
#13488 = CARTESIAN_POINT ( 'NONE',  ( 24.34695368780276681, -2.542362794815061999, -14.38654857168906886 ) ) ;
#13489 = ORIENTED_EDGE ( 'NONE', *, *, #20169, .F. ) ;
#13490 = CARTESIAN_POINT ( 'NONE',  ( 167.2287565553229740, -1.999999999999970468, -29.49038105676660493 ) ) ;
#13491 = CARTESIAN_POINT ( 'NONE',  ( 26.40146419187390947, -13.39824708621661919, -13.49681364666919059 ) ) ;
#13492 = VECTOR ( 'NONE', #27795, 1000.000000000000000 ) ;
#13493 = CARTESIAN_POINT ( 'NONE',  ( 27.66237087416717699, -12.37519551434573017, -14.68082181149132204 ) ) ;
#13494 = AXIS2_PLACEMENT_3D ( 'NONE', #8099, #10539, #24149 ) ;
#13495 = VERTEX_POINT ( 'NONE', #29029 ) ;
#13496 = DIRECTION ( 'NONE',  ( 5.782411586589357392E-17, -0.000000000000000000, 1.000000000000000000 ) ) ;
#13497 = VECTOR ( 'NONE', #1737, 1000.000000000000000 ) ;
#13498 = PRODUCT_DEFINITION_SHAPE ( 'NONE', 'NONE',  #9305 ) ;
#13499 = DIRECTION ( 'NONE',  ( 0.3090169943749475623, 8.338696094058001131E-17, 0.9510565162951536422 ) ) ;
#13500 = VERTEX_POINT ( 'NONE', #9757 ) ;
#13501 = LINE ( 'NONE', #6497, #1974 ) ;
#13502 = LINE ( 'NONE', #6197, #2357 ) ;
#13503 = FACE_OUTER_BOUND ( 'NONE', #16485, .T. ) ;
#13504 = CIRCLE ( 'NONE', #26699, 8.000000000000000000 ) ;
#13505 = CARTESIAN_POINT ( 'NONE',  ( 9.641350810849047548, 17.66889113945805789, -17.92279151347709032 ) ) ;
#13506 = CARTESIAN_POINT ( 'NONE',  ( 24.47745745569867637, -8.908941985067972524, -13.71056886683244258 ) ) ;
#13507 = CARTESIAN_POINT ( 'NONE',  ( 18.72775033408030154, 1.433941090885695768, -19.03071139844121262 ) ) ;
#13508 = ADVANCED_FACE ( 'NONE', ( #8067, #12050 ), #1220, .T. ) ;
#13509 = CARTESIAN_POINT ( 'NONE',  ( 36.54859390953724585, -22.18451583373416014, -17.22552805718784441 ) ) ;
#13510 = LINE ( 'NONE', #20375, #4174 ) ;
#13511 = VECTOR ( 'NONE', #20061, 1000.000000000000000 ) ;
#13512 = CARTESIAN_POINT ( 'NONE',  ( 11.77869587587188249, 8.711114196793760200, -15.67004689359726299 ) ) ;
#13513 = CARTESIAN_POINT ( 'NONE',  ( 4.000000000000003553, 2.309401076758525573, -2.092734410091829034 ) ) ;
#13514 = FACE_OUTER_BOUND ( 'NONE', #8565, .T. ) ;
#13515 = CARTESIAN_POINT ( 'NONE',  ( 9.664154528927689114, 16.24440939496457403, -17.89215119606715021 ) ) ;
#13516 = FACE_OUTER_BOUND ( 'NONE', #5160, .T. ) ;
#13517 = LINE ( 'NONE', #18096, #1775 ) ;
#13518 = CARTESIAN_POINT ( 'NONE',  ( 16.84948243412402036, 10.49281628697410262, -11.66356073909478575 ) ) ;
#13519 = AXIS2_PLACEMENT_3D ( 'NONE', #18953, #18496, #16663 ) ;
#13520 = ORIENTED_EDGE ( 'NONE', *, *, #23085, .T. ) ;
#13521 = DIRECTION ( 'NONE',  ( 5.782411586589357392E-17, -0.000000000000000000, 1.000000000000000000 ) ) ;
#13522 = DIRECTION ( 'NONE',  ( 1.000000000000000000, 2.698458740408365879E-16, -1.110223024625156540E-16 ) ) ;
#13523 = EDGE_CURVE ( 'NONE', #12812, #5460, #12953, .T. ) ;
#13524 = DIRECTION ( 'NONE',  ( -2.698458740408365879E-16, 1.000000000000000000, 0.000000000000000000 ) ) ;
#13525 = EDGE_CURVE ( 'NONE', #27161, #25583, #901, .T. ) ;
#13526 = EDGE_CURVE ( 'NONE', #8103, #7935, #5948, .T. ) ;
#13527 = ORIENTED_EDGE ( 'NONE', *, *, #7768, .F. ) ;
#13528 = EDGE_CURVE ( 'NONE', #14964, #2461, #26884, .T. ) ;
#13529 = CARTESIAN_POINT ( 'NONE',  ( 8.944584683310379702, 16.95159276115599667, -17.91928203681695564 ) ) ;
#13530 = CARTESIAN_POINT ( 'NONE',  ( 33.88611015167484197, -15.71585695178754882, -20.89774115172086510 ) ) ;
#13531 = CARTESIAN_POINT ( 'NONE',  ( 19.21851095677833499, -0.002285697959038230937, -14.55609667925758544 ) ) ;
#13532 = CARTESIAN_POINT ( 'NONE',  ( 18.54021783837685433, 9.946222303842617407, -15.54065090179396336 ) ) ;
#13533 = VECTOR ( 'NONE', #17980, 999.9999999999998863 ) ;
#13534 = CARTESIAN_POINT ( 'NONE',  ( 159.5152310637604671, -10.00000000000000000, -2.627941064794695691 ) ) ;
#13535 = CARTESIAN_POINT ( 'NONE',  ( 20.25494212361869728, -4.857969563408182090, -14.64469595162225701 ) ) ;
#13536 = VECTOR ( 'NONE', #16196, 1000.000000000000000 ) ;
#13537 = ORIENTED_EDGE ( 'NONE', *, *, #18299, .T. ) ;
#13538 = DIRECTION ( 'NONE',  ( 1.000000000000000000, 2.698458740408365879E-16, -1.110223024625156540E-16 ) ) ;
#13540 = ORIENTED_EDGE ( 'NONE', *, *, #25576, .F. ) ;
#13539 = DIRECTION ( 'NONE',  ( -0.5877852522924731371, -1.586114251531760728E-16, -0.8090169943749474513 ) ) ;
#13541 = CARTESIAN_POINT ( 'NONE',  ( 22.28681211727617040, -5.000000000000011546, -68.59175474945887174 ) ) ;
#13542 = CARTESIAN_POINT ( 'NONE',  ( 143.6922820468854241, -4.999999999999978684, -6.413161187712876909 ) ) ;
#13543 = CARTESIAN_POINT ( 'NONE',  ( 164.7287565553229172, -4.999999999999973355, -7.839745962155600267 ) ) ;
#13544 = CARTESIAN_POINT ( 'NONE',  ( 34.16485483951214519, -11.28898102658429536, -18.35413676833350038 ) ) ;
#13545 = EDGE_LOOP ( 'NONE', ( #25574, #28734, #20939, #2478 ) ) ;
#13546 = CARTESIAN_POINT ( 'NONE',  ( 10.90022735844294388, 8.411956631741958290, -16.28271526948893921 ) ) ;
#13547 = ORIENTED_EDGE ( 'NONE', *, *, #27585, .F. ) ;
#13548 = AXIS2_PLACEMENT_3D ( 'NONE', #347, #26439, #5669 ) ;
#13549 = DIRECTION ( 'NONE',  ( -2.698458740408365879E-16, 1.000000000000000000, 0.000000000000000000 ) ) ;
#13550 = DIRECTION ( 'NONE',  ( -1.110223024625156540E-16, 0.000000000000000000, -1.000000000000000000 ) ) ;
#13551 = CARTESIAN_POINT ( 'NONE',  ( 10.48009811366078381, 16.41514476298091907, -17.33146409796769660 ) ) ;
#13552 = FACE_BOUND ( 'NONE', #6928, .T. ) ;
#13553 = ORIENTED_EDGE ( 'NONE', *, *, #10905, .F. ) ;
#13554 = VECTOR ( 'NONE', #8196, 1000.000000000000000 ) ;
#13555 = CARTESIAN_POINT ( 'NONE',  ( 144.5152310637605524, -10.00000000000000355, -2.627941064794695691 ) ) ;
#13556 = ORIENTED_EDGE ( 'NONE', *, *, #20160, .F. ) ;
#13557 = EDGE_CURVE ( 'NONE', #22085, #20929, #17978, .T. ) ;
#13558 = LINE ( 'NONE', #18441, #25914 ) ;
#13560 = ORIENTED_EDGE ( 'NONE', *, *, #1589, .T. ) ;
#13559 = FACE_OUTER_BOUND ( 'NONE', #28434, .T. ) ;
#13561 = ORIENTED_EDGE ( 'NONE', *, *, #15930, .F. ) ;
#13562 = ORIENTED_EDGE ( 'NONE', *, *, #20073, .F. ) ;
#13563 = EDGE_CURVE ( 'NONE', #20421, #3893, #20124, .T. ) ;
#13564 = CARTESIAN_POINT ( 'NONE',  ( -24.99999999999998934, 60.00000000000000711, 24.99999999999998934 ) ) ;
#13565 = ORIENTED_EDGE ( 'NONE', *, *, #23106, .T. ) ;
#13566 = EDGE_CURVE ( 'NONE', #12292, #28726, #3510, .T. ) ;
#13567 = CARTESIAN_POINT ( 'NONE',  ( 9.661883061612440926, 16.25482663361732705, -23.00000000000000711 ) ) ;
#13568 = CARTESIAN_POINT ( 'NONE',  ( 20.98456156242603754, -1.805893270886621327, -19.41059277335735089 ) ) ;
#13569 = CARTESIAN_POINT ( 'NONE',  ( 19.97442599234820193, -2.778558858265142373, -17.76606689721253574 ) ) ;
#13570 = ORIENTED_EDGE ( 'NONE', *, *, #5784, .F. ) ;
#13571 = CARTESIAN_POINT ( 'NONE',  ( 16.54288150113237066, 3.399532473721276649, -19.15960874834559746 ) ) ;
#13572 = DIRECTION ( 'NONE',  ( -1.000000000000000000, -4.440892098500622217E-16, 0.000000000000000000 ) ) ;
#13573 = DIRECTION ( 'NONE',  ( -0.9510565162951536422, 0.000000000000000000, -0.3090169943749472292 ) ) ;
#13574 = CARTESIAN_POINT ( 'NONE',  ( 21.63873165585565417, 2.424707942738766331, -13.54651715722292060 ) ) ;
#13575 = APPLICATION_CONTEXT ( 'automotive_design' ) ;
#13576 = DIRECTION ( 'NONE',  ( 0.5877852522924731371, 0.000000000000000000, 0.8090169943749474513 ) ) ;
#13577 = CARTESIAN_POINT ( 'NONE',  ( 2.000000000000026201, 3.464101615137736623, 8.673617379884035472E-16 ) ) ;
#13578 = VECTOR ( 'NONE', #26177, 1000.000000000000000 ) ;
#13579 = VECTOR ( 'NONE', #22219, 1000.000000000000114 ) ;
#13580 = EDGE_LOOP ( 'NONE', ( #15436, #3128, #16656, #8597, #25343 ) ) ;
#13581 = ADVANCED_FACE ( 'NONE', ( #10669 ), #22266, .T. ) ;
#13582 = CARTESIAN_POINT ( 'NONE',  ( 10.35864918915110877, 16.97212501191939538, -17.97192418671891190 ) ) ;
#13583 = CARTESIAN_POINT ( 'NONE',  ( 0.000000000000000000, 0.000000000000000000, 1.700000000000000178 ) ) ;
#13584 = CIRCLE ( 'NONE', #440, 2.000000000000000000 ) ;
#13585 = DIRECTION ( 'NONE',  ( -0.8090169943749474513, -2.183098979609982436E-16, -0.5877852522924731371 ) ) ;
#13586 = ORIENTED_EDGE ( 'NONE', *, *, #9062, .F. ) ;
#13587 = ORIENTED_EDGE ( 'NONE', *, *, #3073, .T. ) ;
#13588 = DIRECTION ( 'NONE',  ( 0.9510565162951535312, 2.566386769018988816E-16, -0.3090169943749475623 ) ) ;
#13589 = CARTESIAN_POINT ( 'NONE',  ( 17.54642605795894994, 9.676486402519270058, -18.74681543856335608 ) ) ;
#13590 = CARTESIAN_POINT ( 'NONE',  ( 11.05541531668977662, 17.68942339022145305, -17.91928203681695564 ) ) ;
#13591 = CARTESIAN_POINT ( 'NONE',  ( 34.96805304670973413, -19.57645325810014114, -20.18246498508359466 ) ) ;
#13592 = EDGE_LOOP ( 'NONE', ( #4821, #5185, #13129, #18549 ) ) ;
#13593 = ORIENTED_EDGE ( 'NONE', *, *, #9275, .F. ) ;
#13594 = DIRECTION ( 'NONE',  ( -0.000000000000000000, -0.000000000000000000, -1.000000000000000000 ) ) ;
#13595 = CARTESIAN_POINT ( 'NONE',  ( 12.75811015101040446, 7.626735917299793499, -14.92445666636202617 ) ) ;
#13596 = DIRECTION ( 'NONE',  ( -0.9510565162951536422, 0.000000000000000000, -0.3090169943749472292 ) ) ;
#13597 = DIRECTION ( 'NONE',  ( 1.000000000000000000, 4.440892098500622217E-16, 0.000000000000000000 ) ) ;
#13598 = CARTESIAN_POINT ( 'NONE',  ( 0.000000000000000000, 0.000000000000000000, -2.424599999999998978 ) ) ;
#13599 = ORIENTED_EDGE ( 'NONE', *, *, #17744, .T. ) ;
#13600 = CARTESIAN_POINT ( 'NONE',  ( 12.87691298531170148, 9.519861518574414205, -16.10853261994384411 ) ) ;
#13601 = CARTESIAN_POINT ( 'NONE',  ( 34.33515578781254618, -12.24072284059296933, -19.92088757525016973 ) ) ;
#13602 = CARTESIAN_POINT ( 'NONE',  ( 27.91615220763155847, -6.225400021157185826, -17.67258836524805332 ) ) ;
#13603 = DIRECTION ( 'NONE',  ( 0.9510565162951535312, 2.566386769018988816E-16, -0.3090169943749475623 ) ) ;
#13604 = VECTOR ( 'NONE', #14849, 1000.000000000000000 ) ;
#13605 = LINE ( 'NONE', #22933, #24002 ) ;
#13606 = CARTESIAN_POINT ( 'NONE',  ( 24.40455984355908114, -10.10244183743681035, -17.68366952546245585 ) ) ;
#13607 = CARTESIAN_POINT ( 'NONE',  ( 25.81628275165185116, -0.2054900511636704452, -18.66752024111776009 ) ) ;
#13608 = ORIENTED_EDGE ( 'NONE', *, *, #6862, .F. ) ;
#13609 = CARTESIAN_POINT ( 'NONE',  ( 160.0000000000000000, -10.00000000000000000, -15.00000000000000000 ) ) ;
#13610 = EDGE_CURVE ( 'NONE', #28478, #1397, #27195, .T. ) ;
#13611 = CARTESIAN_POINT ( 'NONE',  ( 147.2287565553230309, -1.999999999999976241, -20.83012701892220520 ) ) ;
#13612 = AXIS2_PLACEMENT_3D ( 'NONE', #14442, #21022, #23781 ) ;
#13613 = CARTESIAN_POINT ( 'NONE',  ( 144.5152310637605808, -10.00000000000000178, -30.37205893520530964 ) ) ;
#13614 = CARTESIAN_POINT ( 'NONE',  ( 8.000000000000010658, 0.7809653281576138806, -7.280248181650708259E-15 ) ) ;
#13615 = CARTESIAN_POINT ( 'NONE',  ( 12.60945047077962933, 8.619070305187777947, -15.04294105552940231 ) ) ;
#13616 = VECTOR ( 'NONE', #13539, 1000.000000000000000 ) ;
#13617 = CARTESIAN_POINT ( 'NONE',  ( 28.92040988821396752, -12.03996551347764132, -12.87516188627701474 ) ) ;
#13618 = ORIENTED_EDGE ( 'NONE', *, *, #25069, .T. ) ;
#13619 = DIRECTION ( 'NONE',  ( 2.698458740408365879E-16, -1.000000000000000000, 0.000000000000000000 ) ) ;
#13620 = ORIENTED_EDGE ( 'NONE', *, *, #26927, .T. ) ;
#13621 = CARTESIAN_POINT ( 'NONE',  ( 9.641404825192898542, 17.66864342279195199, -17.88841768828662282 ) ) ;
#13622 = CARTESIAN_POINT ( 'NONE',  ( 17.24236049518817282, 9.271217979531970244, -15.28210331290996571 ) ) ;
#13623 = LINE ( 'NONE', #7071, #19999 ) ;
#13624 = DIRECTION ( 'NONE',  ( 0.3090169943749472292, 8.338696094057992503E-17, -0.9510565162951536422 ) ) ;
#13626 = ORIENTED_EDGE ( 'NONE', *, *, #13895, .F. ) ;
#13625 = CARTESIAN_POINT ( 'NONE',  ( 25.73595588610537277, -4.826321120321507507, -18.84379041344559269 ) ) ;
#13627 = ORIENTED_EDGE ( 'NONE', *, *, #21387, .F. ) ;
#13628 = CARTESIAN_POINT ( 'NONE',  ( -4.000000000000001776, 2.309401076758532678, -2.092734410091829034 ) ) ;
#13629 = CARTESIAN_POINT ( 'NONE',  ( 11.05541531668977662, 17.68942339022145305, -17.92454625180715411 ) ) ;
#13630 = ORIENTED_EDGE ( 'NONE', *, *, #12895, .F. ) ;
#13631 = CARTESIAN_POINT ( 'NONE',  ( 35.53434814243864537, -22.12051714835155281, -18.84852710552948096 ) ) ;
#13632 = PLANE ( 'NONE',  #3014 ) ;
#13633 = ORIENTED_EDGE ( 'NONE', *, *, #19722, .F. ) ;
#13634 = ORIENTED_EDGE ( 'NONE', *, *, #29176, .F. ) ;
#13635 = CARTESIAN_POINT ( 'NONE',  ( 26.72610680620850232, -7.491537437428757329, -18.63066883040512067 ) ) ;
#13636 = DIRECTION ( 'NONE',  ( -1.000000000000000000, 0.000000000000000000, 0.000000000000000000 ) ) ;
#13637 = CARTESIAN_POINT ( 'NONE',  ( 23.66523006742493251, -0.7244823556979478330, -15.35173719993635011 ) ) ;
#13638 = ORIENTED_EDGE ( 'NONE', *, *, #15591, .T. ) ;
#13639 = PRODUCT_DEFINITION_FORMATION_WITH_SPECIFIED_SOURCE ( 'ANY', '', #29395, .NOT_KNOWN. ) ;
#13640 = CARTESIAN_POINT ( 'NONE',  ( 129.5152310637605808, -1.999999999999982236, -2.627941064794695691 ) ) ;
#13641 = VECTOR ( 'NONE', #4218, 1000.000000000000000 ) ;
#13642 = CARTESIAN_POINT ( 'NONE',  ( 14.59671049609067950, 6.266606045730605423, -20.00302036566705155 ) ) ;
#13643 = CARTESIAN_POINT ( 'NONE',  ( 25.27233071153842303, -10.58027458246514207, -17.53878701932553952 ) ) ;
#13644 = CONICAL_SURFACE ( 'NONE', #26349, 4.000000000000003553, 1.047197551196597853 ) ;
#13645 = VECTOR ( 'NONE', #15785, 1000.000000000000000 ) ;
#13646 = EDGE_LOOP ( 'NONE', ( #3494, #19888, #55, #30236 ) ) ;
#13647 = DIRECTION ( 'NONE',  ( -2.698458740408365879E-16, 1.000000000000000000, 0.000000000000000000 ) ) ;
#13648 = CARTESIAN_POINT ( 'NONE',  ( -24.99999999999999289, 60.00000000000000711, -25.00000000000000000 ) ) ;
#13649 = VERTEX_POINT ( 'NONE', #19976 ) ;
#13650 = EDGE_CURVE ( 'NONE', #26271, #1554, #8523, .T. ) ;
#13651 = EDGE_CURVE ( 'NONE', #15181, #6555, #29657, .T. ) ;
#13652 = LINE ( 'NONE', #4057, #19016 ) ;
#13653 = VECTOR ( 'NONE', #693, 1000.000000000000000 ) ;
#13654 = DIRECTION ( 'NONE',  ( -0.5877852522924731371, -1.586114251531760235E-16, 0.8090169943749474513 ) ) ;
#13655 = EDGE_CURVE ( 'NONE', #22368, #220, #29504, .T. ) ;
#13656 = CARTESIAN_POINT ( 'NONE',  ( 169.5152310637605240, -4.999999999999971578, -28.60870317832789667 ) ) ;
#13657 = EDGE_CURVE ( 'NONE', #10342, #24640, #10961, .T. ) ;
#13658 = LINE ( 'NONE', #22982, #28728 ) ;
#13659 = CARTESIAN_POINT ( 'NONE',  ( 25.54411345550068191, -6.057473962578058035, -19.57277538061955013 ) ) ;
#13660 = CARTESIAN_POINT ( 'NONE',  ( 16.05281274719596496, 2.901206577426825639, -17.92093306952238407 ) ) ;
#13661 = CARTESIAN_POINT ( 'NONE',  ( 32.76003276007612186, -9.647047962658168885, -18.46200315532429315 ) ) ;
#13663 = DIRECTION ( 'NONE',  ( 1.000000000000000000, 0.000000000000000000, 0.000000000000000000 ) ) ;
#13662 = COLOUR_RGB ( '', 0.09019608, 0.27058824, 0.51372549) ;
#13664 = CARTESIAN_POINT ( 'NONE',  ( 11.47181023233108021, 9.274170903235749108, -15.86135313853478657 ) ) ;
#13665 = CARTESIAN_POINT ( 'NONE',  ( 12.74999999999999822, 0.000000000000000000, 0.000000000000000000 ) ) ;
#13666 = CARTESIAN_POINT ( 'NONE',  ( 2.500000000000000444, 1.178949249685215417, -2.042000000000002036 ) ) ;
#13667 = CARTESIAN_POINT ( 'NONE',  ( 9.829968513350019421, 15.48396532603707421, -17.81804186139787660 ) ) ;
#13668 = CARTESIAN_POINT ( 'NONE',  ( -4.000000000000020428, -6.928203230275511437, -5.000000000000000888 ) ) ;
#13669 = ORIENTED_EDGE ( 'NONE', *, *, #21164, .F. ) ;
#13670 = CARTESIAN_POINT ( 'NONE',  ( 110.3859817318374184, -4.999999999999987566, -80.20011022380273857 ) ) ;
#13671 = CARTESIAN_POINT ( 'NONE',  ( 11.69419402147360110, 8.800013620902292999, -15.72776802682527730 ) ) ;
#13672 = ORIENTED_EDGE ( 'NONE', *, *, #9062, .T. ) ;
#13673 = LINE ( 'NONE', #16413, #26654 ) ;
#13674 = CARTESIAN_POINT ( 'NONE',  ( -4.683753385137379155E-14, -9.237604307034027684, -4.285468820183664818 ) ) ;
#13675 = CARTESIAN_POINT ( 'NONE',  ( 15.73644607668725826, 9.740111719757674535, -14.94734896276200153 ) ) ;
#13676 = ORIENTED_EDGE ( 'NONE', *, *, #2713, .T. ) ;
#13677 = ORIENTED_EDGE ( 'NONE', *, *, #12929, .T. ) ;
#13678 = CARTESIAN_POINT ( 'NONE',  ( 9.105507159292685060, 16.21358177345661389, -17.05825009255364932 ) ) ;
#13680 = CONICAL_SURFACE ( 'NONE', #10761, 8.000000000000007105, 1.047197551196596077 ) ;
#13679 = CARTESIAN_POINT ( 'NONE',  ( 33.52946124453396237, -14.11362233419136381, -20.78993474304632372 ) ) ;
#13681 = CARTESIAN_POINT ( 'NONE',  ( 20.08305308227469510, 0.3843232119764288246, -14.09874237319206358 ) ) ;
#13682 = AXIS2_PLACEMENT_3D ( 'NONE', #5764, #8037, #14891 ) ;
#13683 = CARTESIAN_POINT ( 'NONE',  ( 16.80936620776159884, 5.784822248606665163, -14.58992565756060245 ) ) ;
#13684 = DIRECTION ( 'NONE',  ( 0.9510565162951535312, 2.566386769018988816E-16, -0.3090169943749475623 ) ) ;
#13685 = CARTESIAN_POINT ( 'NONE',  ( 24.74990718239607546, -5.907774739380937667, -20.30682099139976060 ) ) ;
#13686 = EDGE_CURVE ( 'NONE', #30115, #14294, #19816, .T. ) ;
#13687 = ORIENTED_EDGE ( 'NONE', *, *, #22321, .T. ) ;
#13688 = DIRECTION ( 'NONE',  ( 1.000000000000000000, 2.698458740408365879E-16, -1.110223024625156540E-16 ) ) ;
#13690 = ORIENTED_EDGE ( 'NONE', *, *, #24948, .F. ) ;
#13689 = SURFACE_SIDE_STYLE ('',( #8806 ) ) ;
#13691 = EDGE_CURVE ( 'NONE', #23457, #24548, #17681, .T. ) ;
#13692 = DIRECTION ( 'NONE',  ( 0.9510565162951536422, 0.000000000000000000, -0.3090169943749475623 ) ) ;
#13693 = EDGE_CURVE ( 'NONE', #17086, #6558, #8373, .T. ) ;
#13694 = ADVANCED_FACE ( 'NONE', ( #26723 ), #17826, .T. ) ;
#13695 = ADVANCED_FACE ( 'NONE', ( #1533 ), #17528, .T. ) ;
#13696 = VECTOR ( 'NONE', #29915, 1000.000000000000000 ) ;
#13697 = CARTESIAN_POINT ( 'NONE',  ( 143.6922820468853956, -1.999999999999978684, -0.6060766987539614181 ) ) ;
#13698 = CARTESIAN_POINT ( 'NONE',  ( 35.54859306210901337, -21.18451202668684985, -18.38798429269037271 ) ) ;
#13699 = VECTOR ( 'NONE', #19157, 1000.000000000000000 ) ;
#13700 = CARTESIAN_POINT ( 'NONE',  ( 10.67100603215144794, 9.034109945373653972, -16.41023209856668785 ) ) ;
#13701 = VERTEX_POINT ( 'NONE', #2432 ) ;
#13702 = CARTESIAN_POINT ( 'NONE',  ( 27.76312469413510442, -10.32446017237915648, -18.80420148706337358 ) ) ;
#13703 = DIRECTION ( 'NONE',  ( 0.9510565162951535312, 2.566386769018988816E-16, -0.3090169943749475623 ) ) ;
#13704 = CARTESIAN_POINT ( 'NONE',  ( 10.47184394332236224, 16.45299944031493311, -17.33487789703667303 ) ) ;
#13705 = FACE_BOUND ( 'NONE', #14146, .T. ) ;
#13706 = CARTESIAN_POINT ( 'NONE',  ( 141.1922820468854241, -10.00000000000000533, -4.936203717676158398 ) ) ;
#13707 = EDGE_LOOP ( 'NONE', ( #28062, #21462, #29170, #27194, #20363 ) ) ;
#13708 = CARTESIAN_POINT ( 'NONE',  ( 134.7287565553230024, -1.999999999999980460, -25.16025403784439973 ) ) ;
#13709 = CARTESIAN_POINT ( 'NONE',  ( 12.50140887008201851, 8.571324787501421127, -15.12905211845398412 ) ) ;
#13710 = ORIENTED_EDGE ( 'NONE', *, *, #29061, .F. ) ;
#13711 = LINE ( 'NONE', #23478, #3303 ) ;
#13712 = ORIENTED_EDGE ( 'NONE', *, *, #12510, .F. ) ;
#13713 = CARTESIAN_POINT ( 'NONE',  ( 9.708396314890595846, 16.04151092502291931, -17.86831624201546020 ) ) ;
#13714 = CARTESIAN_POINT ( 'NONE',  ( 23.24226111988221888, -3.343277867803439829, -18.62279721135557509 ) ) ;
#13715 = CARTESIAN_POINT ( 'NONE',  ( 20.60316120045176902, -2.756227665500133206, -14.85995437523845553 ) ) ;
#13716 = CARTESIAN_POINT ( 'NONE',  ( 22.47820520476076567, 2.340993144345510313, -15.49451772223075707 ) ) ;
#13717 = PLANE ( 'NONE',  #14526 ) ;
#13718 = FACE_OUTER_BOUND ( 'NONE', #28314, .T. ) ;
#13719 = AXIS2_PLACEMENT_3D ( 'NONE', #25202, #4294, #26916 ) ;
#13720 = CARTESIAN_POINT ( 'NONE',  ( 19.83745040964868522, -2.306422872736943575, -14.39351019504378293 ) ) ;
#13721 = CARTESIAN_POINT ( 'NONE',  ( 166.1922820468853672, -4.999999999999972466, -19.40354224447947828 ) ) ;
#13722 = CARTESIAN_POINT ( 'NONE',  ( 172.7287565553229740, -84.33034373659253902, 8.500000000000003553 ) ) ;
#13723 = EDGE_CURVE ( 'NONE', #10764, #26487, #16147, .T. ) ;
#13724 = EDGE_CURVE ( 'NONE', #8663, #5681, #15836, .T. ) ;
#13725 = EDGE_CURVE ( 'NONE', #8387, #22090, #23475, .T. ) ;
#13726 = ADVANCED_FACE ( 'NONE', ( #27496 ), #20713, .T. ) ;
#13727 = CARTESIAN_POINT ( 'NONE',  ( 10.35864918915110877, 16.97212501191939538, -17.95086732675817132 ) ) ;
#13728 = CARTESIAN_POINT ( 'NONE',  ( 35.22227017426903473, -20.71851614966110233, -20.19360243392694088 ) ) ;
#13729 = CARTESIAN_POINT ( 'NONE',  ( 4.000000000000000000, 0.000000000000000000, -2.450000000000000622 ) ) ;
#13730 = ORIENTED_EDGE ( 'NONE', *, *, #14021, .F. ) ;
#13731 = ORIENTED_EDGE ( 'NONE', *, *, #4156, .F. ) ;
#13732 = DIRECTION ( 'NONE',  ( -1.000000000000000000, 0.000000000000000000, -0.000000000000000000 ) ) ;
#13733 = VECTOR ( 'NONE', #15851, 1000.000000000000000 ) ;
#13734 = CARTESIAN_POINT ( 'NONE',  ( 15.54217852991911997, 3.796156774867226247, -18.16774540469225485 ) ) ;
#13735 = CARTESIAN_POINT ( 'NONE',  ( 11.23925813788225447, 16.84629677772421275, -16.81283633444384407 ) ) ;
#13736 = CARTESIAN_POINT ( 'NONE',  ( 35.13870703111577143, -20.34311121210408757, -20.23074448643712486 ) ) ;
#13737 = ORIENTED_EDGE ( 'NONE', *, *, #28410, .T. ) ;
#13738 = ORIENTED_EDGE ( 'NONE', *, *, #12554, .F. ) ;
#13739 = CARTESIAN_POINT ( 'NONE',  ( 9.641485839925177714, 17.66827187890266160, -17.87200850766020110 ) ) ;
#13740 = CARTESIAN_POINT ( 'NONE',  ( 14.64119204185053391, 8.458903494591371697, -13.42360716063767967 ) ) ;
#13741 = PLANE ( 'NONE',  #2006 ) ;
#13742 = CARTESIAN_POINT ( 'NONE',  ( 133.6922820468854241, -4.999999999999982236, -9.266330736598357376 ) ) ;
#13743 = VERTEX_POINT ( 'NONE', #1988 ) ;
#13744 = LINE ( 'NONE', #24915, #8610 ) ;
#13745 = ORIENTED_EDGE ( 'NONE', *, *, #3481, .F. ) ;
#13746 = CARTESIAN_POINT ( 'NONE',  ( 10.47212132250356120, 16.45172734403231729, -17.33476278219207956 ) ) ;
#13747 = CARTESIAN_POINT ( 'NONE',  ( 34.35798975979065517, -12.34328324435382207, -19.92780167937219815 ) ) ;
#13748 = CARTESIAN_POINT ( 'NONE',  ( 26.72181814967143509, -3.137724904577397389, -15.69709663067708050 ) ) ;
#13749 = PLANE ( 'NONE',  #27719 ) ;
#13750 = LINE ( 'NONE', #2184, #29406 ) ;
#13751 = PRODUCT_CONTEXT ( 'NONE', #28636, 'mechanical' ) ;
#13752 = CARTESIAN_POINT ( 'NONE',  ( 14.86918570794847305, 4.945381287188965302, -16.48322999939953704 ) ) ;
#13753 = CARTESIAN_POINT ( 'NONE',  ( 26.42757832573366983, -5.232593867482060013, -19.46531670327460617 ) ) ;
#13754 = VECTOR ( 'NONE', #8504, 1000.000000000000000 ) ;
#13755 = EDGE_LOOP ( 'NONE', ( #12982, #2916, #26807 ) ) ;
#13756 = CARTESIAN_POINT ( 'NONE',  ( 167.0152310637604103, -9.999999999999998224, -0.06116980274991495881 ) ) ;
#13757 = EDGE_CURVE ( 'NONE', #26976, #8129, #7144, .T. ) ;
#13758 = DIRECTION ( 'NONE',  ( 0.000000000000000000, -2.775557561562891351E-17, 1.000000000000000000 ) ) ;
#13759 = CARTESIAN_POINT ( 'NONE',  ( 152.0152310637604671, -1.999999999999976241, -17.38167787843870826 ) ) ;
#13760 = AXIS2_PLACEMENT_3D ( 'NONE', #2787, #25826, #14505 ) ;
#13761 = CARTESIAN_POINT ( 'NONE',  ( 147.0152310637605808, -10.00000000000000178, -26.04193191628311155 ) ) ;
#13762 = UNCERTAINTY_MEASURE_WITH_UNIT (LENGTH_MEASURE( 1.000000000000000082E-05 ), #1729, 'distance_accuracy_value', 'NONE');
#13763 = CARTESIAN_POINT ( 'NONE',  ( 10.80186837770346919, 16.25936630249904269, -15.92067135797631217 ) ) ;
#13764 = CARTESIAN_POINT ( 'NONE',  ( 26.35635630057183576, -13.06715036242849948, -16.03892985609963873 ) ) ;
#13765 = VERTEX_POINT ( 'NONE', #30102 ) ;
#13766 = PLANE ( 'NONE',  #3279 ) ;
#13767 = ORIENTED_EDGE ( 'NONE', *, *, #4832, .T. ) ;
#13768 = CARTESIAN_POINT ( 'NONE',  ( 10.56508425215480074, 13.43253182900300402, -16.23631622730588830 ) ) ;
#13769 = AXIS2_PLACEMENT_3D ( 'NONE', #14873, #5135, #4984 ) ;
#13770 = CARTESIAN_POINT ( 'NONE',  ( 18.33619432801213023, 6.228962682262685568, -18.83744168170139233 ) ) ;
#13771 = LINE ( 'NONE', #27869, #16088 ) ;
#13772 = CARTESIAN_POINT ( 'NONE',  ( 5.986664691729967736, -5.000000000000015987, 18.42505936432567282 ) ) ;
#13774 = ORIENTED_EDGE ( 'NONE', *, *, #16004, .T. ) ;
#13773 = CARTESIAN_POINT ( 'NONE',  ( 27.26129135193747999, -10.77754955263135095, -18.64424489656416739 ) ) ;
#13775 = ORIENTED_EDGE ( 'NONE', *, *, #14573, .F. ) ;
#13776 = DIRECTION ( 'NONE',  ( 0.000000000000000000, 0.000000000000000000, 1.000000000000000000 ) ) ;
#13777 = CARTESIAN_POINT ( 'NONE',  ( 12.24519447470441413, 9.516128708456710328, -15.33325952276184445 ) ) ;
#13778 = ORIENTED_EDGE ( 'NONE', *, *, #15683, .F. ) ;
#13779 = CARTESIAN_POINT ( 'NONE',  ( 33.35202879388211983, -12.33251541790028760, -19.68467382345759376 ) ) ;
#13780 = CARTESIAN_POINT ( 'NONE',  ( 154.7287565553230309, -1.999999999999973577, -33.82050807568879947 ) ) ;
#13781 = ORIENTED_EDGE ( 'NONE', *, *, #28910, .T. ) ;
#13782 = DIRECTION ( 'NONE',  ( -1.110223024625156540E-16, 0.000000000000000000, -1.000000000000000000 ) ) ;
#13783 = CARTESIAN_POINT ( 'NONE',  ( 22.42041779846375604, -0.009017426515379003624, -18.82878497401882001 ) ) ;
#13784 = ORIENTED_EDGE ( 'NONE', *, *, #23336, .F. ) ;
#13785 = FACE_OUTER_BOUND ( 'NONE', #11437, .T. ) ;
#13786 = EDGE_CURVE ( 'NONE', #9503, #5618, #18801, .T. ) ;
#13787 = CARTESIAN_POINT ( 'NONE',  ( 26.29067154119281824, -12.76617647537077538, -18.64558906701574514 ) ) ;
#13788 = CARTESIAN_POINT ( 'NONE',  ( 26.40217035250003974, -9.511505991202637844, -18.98702918838447573 ) ) ;
#13789 = ORIENTED_EDGE ( 'NONE', *, *, #28410, .F. ) ;
#13790 = DIRECTION ( 'NONE',  ( 0.9510565162951536422, 2.566386769018988816E-16, 0.3090169943749472292 ) ) ;
#13791 = VECTOR ( 'NONE', #29244, 1000.000000000000000 ) ;
#13792 = PLANE ( 'NONE',  #28981 ) ;
#13793 = DIRECTION ( 'NONE',  ( -1.000000000000000000, -4.440892098500622217E-16, 0.000000000000000000 ) ) ;
#13794 = CARTESIAN_POINT ( 'NONE',  ( 162.0152310637605240, -4.999999999999973355, -24.27857615940569502 ) ) ;
#13795 = CARTESIAN_POINT ( 'NONE',  ( 21.17399985718842714, -5.000000000000011546, -65.16687077662002991 ) ) ;
#13796 = CARTESIAN_POINT ( 'NONE',  ( 9.745779815811758340, 17.18996641109745482, -16.82979807527155458 ) ) ;
#13797 = CARTESIAN_POINT ( 'NONE',  ( 24.72855373928933531, -1.476844508782828802, -20.15487193605729033 ) ) ;
#13798 = CARTESIAN_POINT ( 'NONE',  ( 15.02162844583664736, 5.759011576665847620, -14.59661587647459591 ) ) ;
#13799 = CARTESIAN_POINT ( 'NONE',  ( 36.54859390953724585, -23.18451583373416014, -18.19919658220850422 ) ) ;
#13800 = FACE_OUTER_BOUND ( 'NONE', #3661, .T. ) ;
#13801 = CARTESIAN_POINT ( 'NONE',  ( 12.23783994716398560, 8.515526397163364791, -15.33449341356891615 ) ) ;
#13802 = LINE ( 'NONE', #30209, #3975 ) ;
#13803 = LINE ( 'NONE', #16102, #29520 ) ;
#13804 = CARTESIAN_POINT ( 'NONE',  ( 17.32873655921053313, 10.26331207550778579, -16.20725374984683143 ) ) ;
#13805 = ORIENTED_EDGE ( 'NONE', *, *, #26527, .T. ) ;
#13806 = LINE ( 'NONE', #20534, #10525 ) ;
#13807 = CARTESIAN_POINT ( 'NONE',  ( 12.50906579366657390, 8.574708520419219937, -15.12294941509656354 ) ) ;
#13808 = ORIENTED_EDGE ( 'NONE', *, *, #12172, .F. ) ;
#13809 = CARTESIAN_POINT ( 'NONE',  ( 166.1922820468853388, -1.999999999999972244, -13.59645775552055902 ) ) ;
#13810 = LINE ( 'NONE', #23444, #26902 ) ;
#13811 = CARTESIAN_POINT ( 'NONE',  ( 15.54217852991911997, 3.796156774867226247, -18.16774540469225485 ) ) ;
#13812 = VECTOR ( 'NONE', #6795, 1000.000000000000000 ) ;
#13813 = VERTEX_POINT ( 'NONE', #13708 ) ;
#13814 = ORIENTED_EDGE ( 'NONE', *, *, #9968, .T. ) ;
#13815 = CARTESIAN_POINT ( 'NONE',  ( 9.122709158550120989, 16.13469121211704049, -17.05051537109504523 ) ) ;
#13816 = CARTESIAN_POINT ( 'NONE',  ( 35.54859390953724585, -23.18451583373416014, -16.94733705004010105 ) ) ;
#13817 = EDGE_CURVE ( 'NONE', #27886, #14797, #25599, .T. ) ;
#13818 = EDGE_CURVE ( 'NONE', #8784, #563, #20571, .T. ) ;
#13819 = CARTESIAN_POINT ( 'NONE',  ( 20.91577097522866424, 8.170114823437694795, -18.25116917207579093 ) ) ;
#13820 = EDGE_CURVE ( 'NONE', #18076, #22605, #25169, .T. ) ;
#13821 = CARTESIAN_POINT ( 'NONE',  ( 29.95311431238071975, -11.57681909846818691, -12.96816900313696230 ) ) ;
#13822 = ADVANCED_FACE ( 'NONE', ( #18440 ), #6855, .T. ) ;
#13823 = ORIENTED_EDGE ( 'NONE', *, *, #18902, .T. ) ;
#13824 = DIRECTION ( 'NONE',  ( 0.000000000000000000, 0.000000000000000000, 1.000000000000000000 ) ) ;
#13825 = CARTESIAN_POINT ( 'NONE',  ( 22.08361411416106534, -2.618483922437499611, -20.46533185456077319 ) ) ;
#13826 = ORIENTED_EDGE ( 'NONE', *, *, #8280, .F. ) ;
#13827 = DIRECTION ( 'NONE',  ( -2.698458740408365879E-16, 1.000000000000000000, 0.000000000000000000 ) ) ;
#13828 = ORIENTED_EDGE ( 'NONE', *, *, #9336, .T. ) ;
#13830 = VERTEX_POINT ( 'NONE', #2283 ) ;
#13829 = DIRECTION ( 'NONE',  ( 1.000000000000000000, 0.000000000000000000, 0.000000000000000000 ) ) ;
#13831 = CARTESIAN_POINT ( 'NONE',  ( 2.500000000000002665, 1.110223024625156738E-15, 19.04999999999997229 ) ) ;
#13832 = CIRCLE ( 'NONE', #703, 4.000000000000004441 ) ;
#13833 = DIRECTION ( 'NONE',  ( 1.110223024625156540E-16, 2.995891024602366092E-32, 1.000000000000000000 ) ) ;
#13834 = CARTESIAN_POINT ( 'NONE',  ( 36.54859390953724585, -21.18451583373416014, -16.11276402859391510 ) ) ;
#13835 = CARTESIAN_POINT ( 'NONE',  ( 12.69188586677704400, 7.599409645471840058, -14.97709067247704340 ) ) ;
#13836 = ORIENTED_EDGE ( 'NONE', *, *, #4868, .T. ) ;
#13837 = DIRECTION ( 'NONE',  ( -2.698458740408365879E-16, 1.000000000000000000, 0.000000000000000000 ) ) ;
#13838 = CARTESIAN_POINT ( 'NONE',  ( 2.339468227445709925, 3.268109542640640353, 5.126666913256651224E-15 ) ) ;
#13839 = CARTESIAN_POINT ( 'NONE',  ( 10.51251736658329961, 16.26646593658467310, -17.31805759646961462 ) ) ;
#13840 = PLANE ( 'NONE',  #22410 ) ;
#13841 = CARTESIAN_POINT ( 'NONE',  ( 129.5152310637605524, -1.999999999999982236, -21.71180489736090991 ) ) ;
#13842 = VERTEX_POINT ( 'NONE', #18588 ) ;
#13843 = CARTESIAN_POINT ( 'NONE',  ( 24.11769355754544719, -5.000000000000010658, -74.22662841669534828 ) ) ;
#13844 = DIRECTION ( 'NONE',  ( 0.5877852522924731371, 1.586114251531760728E-16, -0.8090169943749474513 ) ) ;
#13845 = ORIENTED_EDGE ( 'NONE', *, *, #25254, .F. ) ;
#13846 = DIRECTION ( 'NONE',  ( 0.9510565162951536422, 0.000000000000000000, -0.3090169943749475623 ) ) ;
#13847 = ORIENTED_EDGE ( 'NONE', *, *, #14440, .T. ) ;
#13848 = CARTESIAN_POINT ( 'NONE',  ( 9.678003265275730627, 16.18089732476941833, -17.88088483716984811 ) ) ;
#13849 = ADVANCED_FACE ( 'NONE', ( #4848 ), #4555, .T. ) ;
#13850 = CARTESIAN_POINT ( 'NONE',  ( 24.16235420939608858, 2.058193855977920261, -15.89352170542055198 ) ) ;
#13851 = CARTESIAN_POINT ( 'NONE',  ( 21.88384027766407414, -2.187040905716116868, -14.00385029740408704 ) ) ;
#13852 = EDGE_CURVE ( 'NONE', #4340, #29774, #14148, .T. ) ;
#13853 = VERTEX_POINT ( 'NONE', #22885 ) ;
#13854 = EDGE_CURVE ( 'NONE', #5854, #26798, #29956, .T. ) ;
#13855 = CARTESIAN_POINT ( 'NONE',  ( 21.50147616854745891, 4.214167280306792662, -18.19698480873994839 ) ) ;
#13856 = CARTESIAN_POINT ( 'NONE',  ( 166.1922820468853388, -4.999999999999973355, -13.59645775552055902 ) ) ;
#13857 = DIRECTION ( 'NONE',  ( 1.000000000000000000, 0.000000000000000000, 0.000000000000000000 ) ) ;
#13858 = VECTOR ( 'NONE', #18873, 1000.000000000000000 ) ;
#13859 = ADVANCED_FACE ( 'NONE', ( #16444 ), #8964, .F. ) ;
#13860 = CARTESIAN_POINT ( 'NONE',  ( -4.680456609903995258, -6.535341423375610859, -0.01688885742778332977 ) ) ;
#13861 = CARTESIAN_POINT ( 'NONE',  ( 21.18945582756405344, -5.194394521544061227, -16.21196392551894405 ) ) ;
#13862 = EDGE_LOOP ( 'NONE', ( #10948, #18732, #27604, #13618, #13781, #8417, #23421, #30031 ) ) ;
#13863 = SURFACE_STYLE_FILL_AREA ( #8979 ) ;
#13864 = LINE ( 'NONE', #16769, #5979 ) ;
#13865 = DIRECTION ( 'NONE',  ( 1.000000000000000000, 2.698458740408365879E-16, -1.110223024625156540E-16 ) ) ;
#13866 = CARTESIAN_POINT ( 'NONE',  ( -4.000000000000005329, 2.309401076758490934, -0.3572655899081616515 ) ) ;
#13867 = CARTESIAN_POINT ( 'NONE',  ( 137.0152310637606092, -10.00000000000000533, -24.27857615940569147 ) ) ;
#13868 = CARTESIAN_POINT ( 'NONE',  ( 10.35864918915110877, 16.97212501191939538, -17.92981046679734547 ) ) ;
#13869 = CARTESIAN_POINT ( 'NONE',  ( 35.54859215833182873, -22.18450796649496226, -18.40462262104107083 ) ) ;
#13870 = CARTESIAN_POINT ( 'NONE',  ( 144.7287565553230309, -10.00000000000000355, -33.82050807568879947 ) ) ;
#13871 = ORIENTED_EDGE ( 'NONE', *, *, #30232, .T. ) ;
#13872 = CARTESIAN_POINT ( 'NONE',  ( 11.22197018571015725, 9.100068217651248403, -17.24240020332717904 ) ) ;
#13873 = EDGE_LOOP ( 'NONE', ( #767, #15256, #29160, #6885 ) ) ;
#13874 = LINE ( 'NONE', #29842, #7079 ) ;
#13875 = VECTOR ( 'NONE', #13906, 1000.000000000000000 ) ;
#13876 = CARTESIAN_POINT ( 'NONE',  ( 19.25770813156441008, -2.543370271471735222, -15.40753146551623587 ) ) ;
#13877 = CARTESIAN_POINT ( 'NONE',  ( 11.27605965875426541, 16.67752031190189399, -16.78457976421582742 ) ) ;
#13878 = CARTESIAN_POINT ( 'NONE',  ( 34.39741479528305490, -17.01287786994462792, -20.00997473120332515 ) ) ;
#13879 = ORIENTED_EDGE ( 'NONE', *, *, #13009, .F. ) ;
#13880 = CARTESIAN_POINT ( 'NONE',  ( 9.916411867603999397, 16.40742607105030260, -16.50456570466356965 ) ) ;
#13881 = CARTESIAN_POINT ( 'NONE',  ( 9.641350810849047548, 17.66889113945805789, -17.94384837343789485 ) ) ;
#13882 = CARTESIAN_POINT ( 'NONE',  ( 11.87405209244401760, -5.000000000000014211, 36.54457464447630599 ) ) ;
#13883 = DIRECTION ( 'NONE',  ( -0.8090169943749474513, -2.183098979609982436E-16, 0.5877852522924731371 ) ) ;
#13884 = ORIENTED_EDGE ( 'NONE', *, *, #7018, .T. ) ;
#13885 = CARTESIAN_POINT ( 'NONE',  ( 6.689127551062008514, 5.375634714784629509, -0.3173508448886592226 ) ) ;
#13886 = ORIENTED_EDGE ( 'NONE', *, *, #10958, .F. ) ;
#13887 = CARTESIAN_POINT ( 'NONE',  ( 10.46436961932593945, 16.48727764291732711, -17.33901581970886241 ) ) ;
#13888 = AXIS2_PLACEMENT_3D ( 'NONE', #4842, #7445, #276 ) ;
#13889 = CARTESIAN_POINT ( 'NONE',  ( 36.54645402898028550, -21.17490248391822050, -18.49223762587710951 ) ) ;
#13890 = CARTESIAN_POINT ( 'NONE',  ( 25.07290406138036687, -9.006318079059196791, -17.79994936451110732 ) ) ;
#13891 = EDGE_CURVE ( 'NONE', #23347, #1829, #18132, .T. ) ;
#13892 = EDGE_CURVE ( 'NONE', #5942, #134, #23033, .T. ) ;
#13893 = DIRECTION ( 'NONE',  ( 0.3090169943749472292, 8.338696094057992503E-17, -0.9510565162951536422 ) ) ;
#13894 = VERTEX_POINT ( 'NONE', #9873 ) ;
#13895 = EDGE_CURVE ( 'NONE', #633, #9909, #5152, .T. ) ;
#13896 = DIRECTION ( 'NONE',  ( -0.5877852522924731371, -1.586114251531760728E-16, -0.8090169943749474513 ) ) ;
#13897 = APPLICATION_PROTOCOL_DEFINITION ( 'draft international standard', 'automotive_design', 1998, #19802 ) ;
#13898 = CARTESIAN_POINT ( 'NONE',  ( 16.70639138691818459, 6.939553047386250562, -20.38695695975560085 ) ) ;
#13899 = CARTESIAN_POINT ( 'NONE',  ( 29.29611939376944107, -10.57052713796966081, -13.72407686852593400 ) ) ;
#13900 = VECTOR ( 'NONE', #2951, 1000.000000000000000 ) ;
#13901 = ORIENTED_EDGE ( 'NONE', *, *, #7876, .T. ) ;
#13902 = CARTESIAN_POINT ( 'NONE',  ( 172.0152310637604387, -9.999999999999994671, -17.38167787843871182 ) ) ;
#13903 = AXIS2_PLACEMENT_3D ( 'NONE', #7103, #26190, #395 ) ;
#13904 = LINE ( 'NONE', #13611, #11083 ) ;
#13905 = LINE ( 'NONE', #30166, #30240 ) ;
#13906 = DIRECTION ( 'NONE',  ( -2.698458740408365879E-16, 1.000000000000000000, 0.000000000000000000 ) ) ;
#13907 = VECTOR ( 'NONE', #17940, 1000.000000000000000 ) ;
#13908 = CARTESIAN_POINT ( 'NONE',  ( 10.52543090623380451, 17.52714378424053265, -16.25779133722369707 ) ) ;
#13909 = DIRECTION ( 'NONE',  ( -1.000000000000000000, 0.000000000000000000, 0.000000000000000000 ) ) ;
#13910 = DIRECTION ( 'NONE',  ( -2.698458740408365879E-16, 1.000000000000000000, -0.000000000000000000 ) ) ;
#13911 = ORIENTED_EDGE ( 'NONE', *, *, #20819, .T. ) ;
#13912 = AXIS2_PLACEMENT_3D ( 'NONE', #21745, #19451, #8895 ) ;
#13913 = CARTESIAN_POINT ( 'NONE',  ( 9.949118446627077006, 16.25742953053141804, -16.49103975576934644 ) ) ;
#13914 = VECTOR ( 'NONE', #20527, 1000.000000000000000 ) ;
#13915 = CARTESIAN_POINT ( 'NONE',  ( 15.53255613197921647, 5.987779765840379298, -16.04456276566740058 ) ) ;
#13916 = CARTESIAN_POINT ( 'NONE',  ( -2.000000000000026201, -3.464101615137764156, -2.450000000000000622 ) ) ;
#13917 = LINE ( 'NONE', #11782, #10077 ) ;
#13919 = ORIENTED_EDGE ( 'NONE', *, *, #16738, .T. ) ;
#13918 = CARTESIAN_POINT ( 'NONE',  ( 31.81434894052502571, -10.04473835610349397, -15.03854332269495764 ) ) ;
#13920 = VERTEX_POINT ( 'NONE', #432 ) ;
#13921 = CARTESIAN_POINT ( 'NONE',  ( 148.6922820468853956, -4.999999999999976907, -9.266330736598359152 ) ) ;
#13922 = CARTESIAN_POINT ( 'NONE',  ( 11.29232397858413250, 16.60293006794363535, -16.77785382704750461 ) ) ;
#13923 = CARTESIAN_POINT ( 'NONE',  ( 35.54859390953724585, -22.18451583373416014, -16.94733705004010460 ) ) ;
#13924 = CARTESIAN_POINT ( 'NONE',  ( 138.6922820468854525, -4.999999999999980460, -32.39392330124607611 ) ) ;
#13925 = EDGE_CURVE ( 'NONE', #6899, #9337, #9717, .T. ) ;
#13926 = DIRECTION ( 'NONE',  ( -2.698458740408365879E-16, 1.000000000000000000, 0.000000000000000000 ) ) ;
#13927 = CARTESIAN_POINT ( 'NONE',  ( 23.29143545295710638, -10.05536756138072718, -15.72373794962660831 ) ) ;
#13928 = ADVANCED_FACE ( 'NONE', ( #26382 ), #7592, .T. ) ;
#13929 = ORIENTED_EDGE ( 'NONE', *, *, #24184, .T. ) ;
#13930 = EDGE_CURVE ( 'NONE', #21255, #27047, #17201, .T. ) ;
#13931 = DIRECTION ( 'NONE',  ( -0.9510565162951536422, -2.566386769018988323E-16, 0.3090169943749475623 ) ) ;
#13932 = CARTESIAN_POINT ( 'NONE',  ( 18.12654306171327079, 0.8625984663607378922, -18.09208126113620452 ) ) ;
#13933 = CARTESIAN_POINT ( 'NONE',  ( 27.51083730600015897, -9.905735641176994122, -13.30399992039142099 ) ) ;
#13934 = VECTOR ( 'NONE', #12880, 1000.000000000000000 ) ;
#13935 = ORIENTED_EDGE ( 'NONE', *, *, #20854, .F. ) ;
#13936 = DIRECTION ( 'NONE',  ( -2.698458740408366372E-16, 1.000000000000000000, 0.000000000000000000 ) ) ;
#13937 = AXIS2_PLACEMENT_3D ( 'NONE', #29223, #5537, #10550 ) ;
#13938 = AXIS2_PLACEMENT_3D ( 'NONE', #22342, #8293, #22501 ) ;
#13939 = CARTESIAN_POINT ( 'NONE',  ( 161.1922820468853672, -9.999999999999998224, -22.25671179336496053 ) ) ;
#13940 = CARTESIAN_POINT ( 'NONE',  ( 164.5152310637604955, -1.999999999999971356, -30.37205893520531319 ) ) ;
#13941 = LINE ( 'NONE', #7252, #8976 ) ;
#13942 = CARTESIAN_POINT ( 'NONE',  ( 9.917015787971365626, 16.40465641526357743, -16.50431533440121257 ) ) ;
#13943 = CARTESIAN_POINT ( 'NONE',  ( 23.94974919959990345, -8.117095362258064384, -14.41405346848900848 ) ) ;
#13944 = CARTESIAN_POINT ( 'NONE',  ( 20.05514754915220266, -1.452567280579552866, -14.87399747198034738 ) ) ;
#13945 = EDGE_CURVE ( 'NONE', #1081, #12381, #2880, .T. ) ;
#13946 = CARTESIAN_POINT ( 'NONE',  ( 36.40320260674921116, -22.53134972621836241, -20.30234751949853589 ) ) ;
#13947 = SURFACE_STYLE_FILL_AREA ( #11665 ) ;
#13948 = CARTESIAN_POINT ( 'NONE',  ( 12.52778158092594474, 8.582979361647906202, -15.10803260229456946 ) ) ;
#13949 = VECTOR ( 'NONE', #30189, 1000.000000000000000 ) ;
#13950 = PLANE ( 'NONE',  #2029 ) ;
#13951 = LINE ( 'NONE', #23281, #18293 ) ;
#13952 = DIRECTION ( 'NONE',  ( 0.3090169943749472292, 8.338696094057992503E-17, -0.9510565162951536422 ) ) ;
#13953 = ORIENTED_EDGE ( 'NONE', *, *, #14540, .T. ) ;
#13954 = DIRECTION ( 'NONE',  ( 1.000000000000000000, 0.000000000000000000, 0.000000000000000000 ) ) ;
#13955 = CARTESIAN_POINT ( 'NONE',  ( 10.72588575366639674, 16.60783230186494563, -15.95209284586258214 ) ) ;
#13956 = ORIENTED_EDGE ( 'NONE', *, *, #18943, .F. ) ;
#13957 = VECTOR ( 'NONE', #22890, 1000.000000000000000 ) ;
#13958 = DIRECTION ( 'NONE',  ( -2.698458740408365879E-16, 1.000000000000000000, 0.000000000000000000 ) ) ;
#13959 = DIRECTION ( 'NONE',  ( 0.9510565162951536422, 0.000000000000000000, -0.3090169943749475623 ) ) ;
#13960 = VECTOR ( 'NONE', #6566, 1000.000000000000000 ) ;
#13961 = CARTESIAN_POINT ( 'NONE',  ( 18.47369133221681281, 7.987600538477567014, -15.27093437040897861 ) ) ;
#13962 = EDGE_CURVE ( 'NONE', #20312, #11101, #19185, .T. ) ;
#13963 = VERTEX_POINT ( 'NONE', #23945 ) ;
#13964 = CARTESIAN_POINT ( 'NONE',  ( 35.54859390953724585, -23.18451583373416014, -17.22552805718784441 ) ) ;
#13965 = CARTESIAN_POINT ( 'NONE',  ( 24.85091453934022709, -2.360935040140837771, -14.69038261433388293 ) ) ;
#13966 = CARTESIAN_POINT ( 'NONE',  ( 28.92040988821396752, -12.03996551347764132, -12.87516188627701474 ) ) ;
#13967 = CARTESIAN_POINT ( 'NONE',  ( 27.03394943597420408, -2.104382873295748801, -14.19367964525161163 ) ) ;
#13968 = VECTOR ( 'NONE', #9340, 999.9999999999998863 ) ;
#13969 = ORIENTED_EDGE ( 'NONE', *, *, #15442, .F. ) ;
#13970 = DIRECTION ( 'NONE',  ( -0.9510565162951536422, -2.566386769018988816E-16, -0.3090169943749472292 ) ) ;
#13972 = VERTEX_POINT ( 'NONE', #3035 ) ;
#13971 = PLANE ( 'NONE',  #17031 ) ;
#13973 = VECTOR ( 'NONE', #21415, 1000.000000000000000 ) ;
#13974 = ORIENTED_EDGE ( 'NONE', *, *, #6683, .F. ) ;
#13975 = DIRECTION ( 'NONE',  ( -1.110223024625156540E-16, 0.000000000000000000, -1.000000000000000000 ) ) ;
#13976 = CARTESIAN_POINT ( 'NONE',  ( 159.5152310637605524, -1.999999999999972689, -28.60870317832789667 ) ) ;
#13977 = ADVANCED_FACE ( 'NONE', ( #23784 ), #21783, .T. ) ;
#13978 = CARTESIAN_POINT ( 'NONE',  ( 36.54859390953724585, -21.18451583373416014, -17.78191007148576119 ) ) ;
#13979 = CARTESIAN_POINT ( 'NONE',  ( 9.641359250860388030, 17.66885243249017634, -17.90483003768722625 ) ) ;
#13980 = ADVANCED_FACE ( 'NONE', ( #28691 ), #12009, .T. ) ;
#13981 = ORIENTED_EDGE ( 'NONE', *, *, #11117, .F. ) ;
#13982 = B_SPLINE_CURVE_WITH_KNOTS ( 'NONE', 3,
 ( #17161, #21592, #691, #9978, #19294, #28651 ),
 .UNSPECIFIED., .F., .F.,
 ( 4, 2, 4 ),
 ( 0.002336974151641542981, 0.003500975885716449756, 0.004664977619791356098 ),
 .UNSPECIFIED. ) ;
#13983 = DIRECTION ( 'NONE',  ( 0.5877852522924731371, 1.586114251531760728E-16, 0.8090169943749474513 ) ) ;
#13984 = CARTESIAN_POINT ( 'NONE',  ( 157.0152310637604387, -1.999999999999974909, -0.06116980274991495881 ) ) ;
#13985 = CARTESIAN_POINT ( 'NONE',  ( 10.47079889355419446, 16.45779217176459852, -17.33533584583738829 ) ) ;
#13986 = CYLINDRICAL_SURFACE ( 'NONE', #10216, 4.000000000000000000 ) ;
#13987 = DIRECTION ( 'NONE',  ( -2.698458740408365879E-16, 1.000000000000000000, 0.000000000000000000 ) ) ;
#13988 = ORIENTED_EDGE ( 'NONE', *, *, #18337, .F. ) ;
#13989 = CARTESIAN_POINT ( 'NONE',  ( 164.5152310637604387, -4.999999999999973355, -1.826485974285146238E-14 ) ) ;
#13990 = VECTOR ( 'NONE', #23208, 1000.000000000000000 ) ;
#13991 = CARTESIAN_POINT ( 'NONE',  ( 156.1922820468853672, -4.999999999999975131, -10.74328820663507678 ) ) ;
#13992 = ORIENTED_EDGE ( 'NONE', *, *, #9375, .T. ) ;
#13993 = PLANE ( 'NONE',  #7184 ) ;
#13994 = ORIENTED_EDGE ( 'NONE', *, *, #13925, .F. ) ;
#13995 = CARTESIAN_POINT ( 'NONE',  ( 9.667904883771802460, 16.22720978959070592, -17.88506087084571305 ) ) ;
#13996 = VECTOR ( 'NONE', #28622, 1000.000000000000000 ) ;
#13997 = CARTESIAN_POINT ( 'NONE',  ( 25.76085037594245719, -3.206535967183471669, -15.98314152415894540 ) ) ;
#13998 = CARTESIAN_POINT ( 'NONE',  ( 24.16216977846044145, 1.369666316211566093, -18.31128106405367006 ) ) ;
#13999 = CARTESIAN_POINT ( 'NONE',  ( 16.63724033897865340, 2.930722838386041751, -15.17604395537502526 ) ) ;
#14000 = DIRECTION ( 'NONE',  ( -1.110223024625156540E-16, 0.000000000000000000, -1.000000000000000000 ) ) ;
#14001 = CARTESIAN_POINT ( 'NONE',  ( 159.5152310637605240, -4.999999999999973355, -19.94844914048349693 ) ) ;
#14002 = DIRECTION ( 'NONE',  ( 1.949100835863659470E-16, -2.773645458326357876E-16, -1.000000000000000000 ) ) ;
#14003 = CARTESIAN_POINT ( 'NONE',  ( 24.81358459371387326, -5.676498915796258871, -18.90393244824272756 ) ) ;
#14004 = DIRECTION ( 'NONE',  ( -2.698458740408365879E-16, 1.000000000000000000, 0.000000000000000000 ) ) ;
#14005 = DIRECTION ( 'NONE',  ( 0.5877852522924731371, 0.000000000000000000, 0.8090169943749474513 ) ) ;
#14006 = DIRECTION ( 'NONE',  ( -1.000000000000000000, 0.000000000000000000, 0.000000000000000000 ) ) ;
#14007 = AXIS2_PLACEMENT_3D ( 'NONE', #7481, #24117, #23662 ) ;
#14008 = CARTESIAN_POINT ( 'NONE',  ( 147.0152310637605240, -10.00000000000000355, 1.702185954127501066 ) ) ;
#14009 = DIRECTION ( 'NONE',  ( 1.000000000000000000, 0.000000000000000000, -0.000000000000000000 ) ) ;
#14010 = CARTESIAN_POINT ( 'NONE',  ( 10.35866308580767026, 16.97206128008099313, -17.90676409391864610 ) ) ;
#14011 = ADVANCED_FACE ( 'NONE', ( #723 ), #12459, .T. ) ;
#14013 = VERTEX_POINT ( 'NONE', #7744 ) ;
#14012 = LINE ( 'NONE', #16015, #17955 ) ;
#14014 = DIRECTION ( 'NONE',  ( 0.9510565162951536422, 0.000000000000000000, -0.3090169943749475623 ) ) ;
#14015 = AXIS2_PLACEMENT_3D ( 'NONE', #25513, #15884, #27540 ) ;
#14016 = VERTEX_POINT ( 'NONE', #12615 ) ;
#14017 = CARTESIAN_POINT ( 'NONE',  ( 11.23996880139866761, 9.021883543159612273, -17.23462466665071346 ) ) ;
#14018 = ADVANCED_FACE ( 'NONE', ( #7298 ), #4196, .T. ) ;
#14019 = ORIENTED_EDGE ( 'NONE', *, *, #23837, .F. ) ;
#14020 = DIRECTION ( 'NONE',  ( 1.000000000000000000, 0.000000000000000000, 0.000000000000000000 ) ) ;
#14021 = EDGE_CURVE ( 'NONE', #10807, #2818, #5611, .T. ) ;
#14022 = CARTESIAN_POINT ( 'NONE',  ( 17.72480397827495224, 1.356124466512965476, -19.40231245121514903 ) ) ;
#14023 = CARTESIAN_POINT ( 'NONE',  ( 11.30853360504539751, 16.52859065474556033, -16.77115057629831441 ) ) ;
#14024 = LINE ( 'NONE', #465, #1467 ) ;
#14025 = ORIENTED_EDGE ( 'NONE', *, *, #27215, .F. ) ;
#14026 = AXIS2_PLACEMENT_3D ( 'NONE', #3244, #945, #23849 ) ;
#14027 = ORIENTED_EDGE ( 'NONE', *, *, #11250, .T. ) ;
#14028 = CARTESIAN_POINT ( 'NONE',  ( 9.917712295358372288, 16.40146214360271770, -16.50402730409559027 ) ) ;
#14029 = LINE ( 'NONE', #4736, #20843 ) ;
#14030 = CARTESIAN_POINT ( 'NONE',  ( 9.981537699549546616, 16.10875070413535681, -16.47763325427154868 ) ) ;
#14031 = DIRECTION ( 'NONE',  ( 0.5877852522924731371, 1.586114251531760728E-16, 0.8090169943749474513 ) ) ;
#14032 = LINE ( 'NONE', #5038, #4278 ) ;
#14033 = EDGE_LOOP ( 'NONE', ( #13237, #5707, #5069, #24734, #21479 ) ) ;
#14034 = CARTESIAN_POINT ( 'NONE',  ( 176.1922820468853104, -9.999999999999994671, -19.40354224447947828 ) ) ;
#14035 = EDGE_LOOP ( 'NONE', ( #28132, #24728, #7432, #21215 ) ) ;
#14036 = CARTESIAN_POINT ( 'NONE',  ( 10.47300640208398370, 16.44766825625507778, -17.33439677017039671 ) ) ;
#14037 = ORIENTED_EDGE ( 'NONE', *, *, #27058, .F. ) ;
#14038 = CARTESIAN_POINT ( 'NONE',  ( 36.54859390953723874, -22.18451583373416014, -15.00000000000000000 ) ) ;
#14039 = CARTESIAN_POINT ( 'NONE',  ( 26.72610680620850232, -7.491537437428757329, -18.63066883040512067 ) ) ;
#14040 = CIRCLE ( 'NONE', #24298, 4.000000000000000000 ) ;
#14041 = PLANE ( 'NONE',  #4759 ) ;
#14042 = CARTESIAN_POINT ( 'NONE',  ( 32.71419323209526908, -10.28616775856061416, -16.33292762241428520 ) ) ;
#14043 = DIRECTION ( 'NONE',  ( 0.000000000000000000, 0.000000000000000000, -1.000000000000000000 ) ) ;
#14044 = CARTESIAN_POINT ( 'NONE',  ( 18.54021783837685433, 9.946222303842617407, -15.54065090179396336 ) ) ;
#14045 = AXIS2_PLACEMENT_3D ( 'NONE', #23485, #2592, #23329 ) ;
#14046 = CARTESIAN_POINT ( 'NONE',  ( 26.06970682676011464, -9.363093171025507644, -17.79562309782675911 ) ) ;
#14047 = VECTOR ( 'NONE', #19497, 1000.000000000000000 ) ;
#14048 = ORIENTED_EDGE ( 'NONE', *, *, #11078, .T. ) ;
#14049 = FACE_BOUND ( 'NONE', #1343, .T. ) ;
#14050 = VECTOR ( 'NONE', #4281, 1000.000000000000000 ) ;
#14051 = DIRECTION ( 'NONE',  ( 0.000000000000000000, 0.000000000000000000, 1.000000000000000000 ) ) ;
#14052 = CARTESIAN_POINT ( 'NONE',  ( 146.1922820468853956, -1.999999999999977573, -2.083034168790677043 ) ) ;
#14053 = ADVANCED_FACE ( 'NONE', ( #28245 ), #29094, .T. ) ;
#14054 = CARTESIAN_POINT ( 'NONE',  ( 5.000000000000004441, 0.000000000000000000, 0.000000000000000000 ) ) ;
#14055 = PRODUCT_DEFINITION_CONTEXT ( 'detailed design', #6759, 'design' ) ;
#14056 = EDGE_CURVE ( 'NONE', #10176, #27390, #14743, .T. ) ;
#14057 = EDGE_CURVE ( 'NONE', #3119, #15024, #21627, .T. ) ;
#14058 = CARTESIAN_POINT ( 'NONE',  ( 10.59516011209494302, 17.20735675775515361, -16.09619895116188815 ) ) ;
#14059 = EDGE_CURVE ( 'NONE', #1878, #24297, #12164, .T. ) ;
#14060 = DIRECTION ( 'NONE',  ( -0.000000000000000000, -0.000000000000000000, 1.000000000000000000 ) ) ;
#14061 = VERTEX_POINT ( 'NONE', #9565 ) ;
#14062 = AXIS2_PLACEMENT_3D ( 'NONE', #7702, #17013, #14704 ) ;
#14063 = CARTESIAN_POINT ( 'NONE',  ( 107.8490226364544498, -4.999999999999987566, -78.35690154919700490 ) ) ;
#14064 = ORIENTED_EDGE ( 'NONE', *, *, #5894, .T. ) ;
#14065 = CARTESIAN_POINT ( 'NONE',  ( 9.932908820165812003, 16.33176894372950727, -16.49774300651844072 ) ) ;
#14066 = CARTESIAN_POINT ( 'NONE',  ( 30.58694070296994028, -11.15840821071237698, -14.58880109071565556 ) ) ;
#14067 = FACE_OUTER_BOUND ( 'NONE', #20989, .T. ) ;
#14068 = CARTESIAN_POINT ( 'NONE',  ( 74.18800000000001660, 0.000000000000000000, 0.000000000000000000 ) ) ;
#14069 = CARTESIAN_POINT ( 'NONE',  ( 26.36224721256908410, -8.875037662531589433, -13.49479840426202948 ) ) ;
#14070 = VECTOR ( 'NONE', #5172, 999.9999999999998863 ) ;
#14071 = EDGE_LOOP ( 'NONE', ( #2885, #7398, #19518, #8496 ) ) ;
#14072 = CARTESIAN_POINT ( 'NONE',  ( 149.5152310637604955, -1.999999999999976685, -4.391296821672111328 ) ) ;
#14073 = CARTESIAN_POINT ( 'NONE',  ( 11.05714535396004727, 17.68148921877153157, -17.77574279453144968 ) ) ;
#14074 = EDGE_LOOP ( 'NONE', ( #27733, #27343, #23512, #29597 ) ) ;
#14075 = CARTESIAN_POINT ( 'NONE',  ( 33.91010249890941708, -13.82364185882242147, -18.82035036639317482 ) ) ;
#14076 = CARTESIAN_POINT ( 'NONE',  ( 17.69365662292968366, 10.27476822432933545, -17.01437286930526227 ) ) ;
#14077 = DIRECTION ( 'NONE',  ( -0.5877852522924731371, -1.586114251531760728E-16, -0.8090169943749474513 ) ) ;
#14078 = CARTESIAN_POINT ( 'NONE',  ( 28.21504805113574221, -4.147720155524260655, -15.34900075604336500 ) ) ;
#14079 = ORIENTED_EDGE ( 'NONE', *, *, #30163, .T. ) ;
#14080 = CARTESIAN_POINT ( 'NONE',  ( 3.999999999999996447, 0.000000000000000000, 8.673617379884035472E-16 ) ) ;
#14081 = CARTESIAN_POINT ( 'NONE',  ( 19.14470263920462401, 1.819183656627200829, -19.33730474122706866 ) ) ;
#14082 = CARTESIAN_POINT ( 'NONE',  ( 16.42791133306356599, 6.383902638027607601, -15.35376453018263199 ) ) ;
#14083 = VERTEX_POINT ( 'NONE', #8184 ) ;
#14084 = ORIENTED_EDGE ( 'NONE', *, *, #7018, .F. ) ;
#14085 = CARTESIAN_POINT ( 'NONE',  ( 19.50478146705679450, -5.000000000000012434, -60.02954481736172454 ) ) ;
#14086 = VECTOR ( 'NONE', #11322, 1000.000000000000000 ) ;
#14087 = CARTESIAN_POINT ( 'NONE',  ( 8.772461160124507273, -5.000000000000015099, 26.99885929302450904 ) ) ;
#14088 = AXIS2_PLACEMENT_3D ( 'NONE', #1176, #26830, #22072 ) ;
#14089 = PLANE ( 'NONE',  #29104 ) ;
#14090 = DIRECTION ( 'NONE',  ( 0.5877852522924731371, 1.586114251531760728E-16, 0.8090169943749474513 ) ) ;
#14091 = EDGE_CURVE ( 'NONE', #17985, #4670, #26848, .T. ) ;
#14092 = DIRECTION ( 'NONE',  ( -0.8090169943749474513, -2.183098979609982436E-16, -0.5877852522924731371 ) ) ;
#14093 = EDGE_CURVE ( 'NONE', #30260, #1558, #13230, .T. ) ;
#14094 = CARTESIAN_POINT ( 'NONE',  ( 9.843778300897430000, 16.74053286659246709, -16.57516421589427225 ) ) ;
#14095 = ADVANCED_FACE ( 'NONE', ( #3928 ), #13071, .T. ) ;
#14096 = CARTESIAN_POINT ( 'NONE',  ( 25.25929662509423324, 0.6462067467026075818, -14.45468018858982795 ) ) ;
#14097 = CARTESIAN_POINT ( 'NONE',  ( 23.93603600111211804, 0.1510904554606163908, -14.93755387302875448 ) ) ;
#14099 = EDGE_LOOP ( 'NONE', ( #8567, #5153, #1269, #96 ) ) ;
#14098 = CARTESIAN_POINT ( 'NONE',  ( 36.54859390953724585, -23.18451583373416014, -16.11276402859391510 ) ) ;
#14100 = DIRECTION ( 'NONE',  ( -1.110223024625156540E-16, 0.000000000000000000, -1.000000000000000000 ) ) ;
#14101 = CARTESIAN_POINT ( 'NONE',  ( 158.6922820468853104, -10.00000000000000000, -0.6060766987539614181 ) ) ;
#14102 = CARTESIAN_POINT ( 'NONE',  ( 143.6922820468854525, -4.999999999999978684, -17.92658477444275889 ) ) ;
#14103 = CARTESIAN_POINT ( 'NONE',  ( 168.6922820468852819, -1.999999999999971356, 2.247092850131519715 ) ) ;
#14105 = VERTEX_POINT ( 'NONE', #12767 ) ;
#14104 = CARTESIAN_POINT ( 'NONE',  ( 16.53342136567307108, 10.04554801986687629, -15.32032680638607047 ) ) ;
#14106 = EDGE_LOOP ( 'NONE', ( #16726, #7906, #19815, #18327 ) ) ;
#14107 = CARTESIAN_POINT ( 'NONE',  ( 148.6922820468854241, -10.00000000000000178, -15.07341522555727664 ) ) ;
#14108 = CARTESIAN_POINT ( 'NONE',  ( 10.34291491886349235, 18.36418536769788901, -17.61263766090776528 ) ) ;
#14109 = ORIENTED_EDGE ( 'NONE', *, *, #28546, .T. ) ;
#14110 = AXIS2_PLACEMENT_3D ( 'NONE', #15863, #8696, #29679 ) ;
#14111 = DIRECTION ( 'NONE',  ( -0.8090169943749474513, -2.183098979609982436E-16, 0.5877852522924731371 ) ) ;
#14112 = CARTESIAN_POINT ( 'NONE',  ( 168.6922820468852819, -9.999999999999998224, -0.6060766987539614181 ) ) ;
#14113 = VECTOR ( 'NONE', #2643, 1000.000000000000000 ) ;
#14114 = CARTESIAN_POINT ( 'NONE',  ( 19.23836061553175369, 5.151828676608854352, -13.99136221198299168 ) ) ;
#14115 = ORIENTED_EDGE ( 'NONE', *, *, #26991, .F. ) ;
#14116 = VECTOR ( 'NONE', #10313, 1000.000000000000000 ) ;
#14117 = CARTESIAN_POINT ( 'NONE',  ( 29.49229018507869071, -8.391778287988243434, -19.20830874944899236 ) ) ;
#14118 = STYLED_ITEM ( 'NONE', ( #15033 ), #1835 ) ;
#14119 = ORIENTED_EDGE ( 'NONE', *, *, #23378, .T. ) ;
#14120 = CARTESIAN_POINT ( 'NONE',  ( 34.59940796595157053, -18.92032618698594248, -21.11335396907232465 ) ) ;
#14121 = CARTESIAN_POINT ( 'NONE',  ( 22.82249278870453679, 0.4072072893072278821, -18.57859108775207702 ) ) ;
#14122 = CARTESIAN_POINT ( 'NONE',  ( 20.54317392443767076, 4.330699614500605144, -17.92201748610454715 ) ) ;
#14123 = EDGE_LOOP ( 'NONE', ( #20754, #28070, #10328, #26665, #20614 ) ) ;
#14124 = CARTESIAN_POINT ( 'NONE',  ( 25.33177305468611351, -7.180647579645999201, -12.45679661262278870 ) ) ;
#14125 = ADVANCED_FACE ( 'NONE', ( #10927 ), #6063, .T. ) ;
#14126 = VECTOR ( 'NONE', #22049, 1000.000000000000000 ) ;
#14127 = VECTOR ( 'NONE', #5074, 1000.000000000000000 ) ;
#14128 = VERTEX_POINT ( 'NONE', #3776 ) ;
#14129 = DIRECTION ( 'NONE',  ( 0.5877852522924731371, 1.586114251531760728E-16, -0.8090169943749474513 ) ) ;
#14130 = AXIS2_PLACEMENT_3D ( 'NONE', #304, #4577, #18756 ) ;
#14131 = LINE ( 'NONE', #14277, #5332 ) ;
#14132 = ORIENTED_EDGE ( 'NONE', *, *, #21975, .F. ) ;
#14133 = DIRECTION ( 'NONE',  ( 0.3090169943749472292, 8.338696094057992503E-17, -0.9510565162951536422 ) ) ;
#14134 = EDGE_CURVE ( 'NONE', #15955, #23249, #22394, .T. ) ;
#14135 = LINE ( 'NONE', #7440, #10725 ) ;
#14136 = CARTESIAN_POINT ( 'NONE',  ( 34.61906131182126245, -12.51614797404085877, -18.96439083239160439 ) ) ;
#14137 = CARTESIAN_POINT ( 'NONE',  ( 9.641350810849047548, 17.66889113945805789, -17.93331994345748370 ) ) ;
#14138 = ORIENTED_EDGE ( 'NONE', *, *, #15715, .T. ) ;
#14139 = DIRECTION ( 'NONE',  ( -0.5877852522924731371, 0.000000000000000000, 0.8090169943749474513 ) ) ;
#14140 = DIRECTION ( 'NONE',  ( 0.9510565162951536422, 2.566386769018988816E-16, 0.3090169943749472292 ) ) ;
#14141 = CARTESIAN_POINT ( 'NONE',  ( 10.47325967749744180, 16.44650670292386607, -17.33429203187744250 ) ) ;
#14142 = DIRECTION ( 'NONE',  ( -1.110223024625156540E-16, 0.000000000000000000, -1.000000000000000000 ) ) ;
#14143 = DIRECTION ( 'NONE',  ( 1.000000000000000000, 2.698458740408365879E-16, -1.110223024625156540E-16 ) ) ;
#14144 = VECTOR ( 'NONE', #8039, 1000.000000000000000 ) ;
#14145 = MECHANICAL_DESIGN_GEOMETRIC_PRESENTATION_REPRESENTATION (  '', ( #3455 ), #25382 ) ;
#14146 = EDGE_LOOP ( 'NONE', ( #19723, #28474, #4612, #14808, #19075 ) ) ;
#14147 = VECTOR ( 'NONE', #8786, 999.9999999999998863 ) ;
#14148 = LINE ( 'NONE', #13989, #1283 ) ;
#14149 = DIRECTION ( 'NONE',  ( 1.000000000000000000, 0.000000000000000000, 0.000000000000000000 ) ) ;
#14150 = VERTEX_POINT ( 'NONE', #1498 ) ;
#14151 = FACE_OUTER_BOUND ( 'NONE', #30180, .T. ) ;
#14152 = EDGE_LOOP ( 'NONE', ( #26358, #12857, #22939, #22159 ) ) ;
#14153 = CARTESIAN_POINT ( 'NONE',  ( 10.18658029549746935, 13.84849823568026217, -17.67057034492011525 ) ) ;
#14154 = VECTOR ( 'NONE', #12939, 1000.000000000000000 ) ;
#14155 = CARTESIAN_POINT ( 'NONE',  ( 23.80376867147650444, -3.845223433682474212, -14.48388124448521452 ) ) ;
#14156 = CARTESIAN_POINT ( 'NONE',  ( 16.00562779705659011, 2.776126820729137190, -17.20623408552720690 ) ) ;
#14157 = CARTESIAN_POINT ( 'NONE',  ( 164.5152310637604387, -1.999999999999972689, -4.391296821672111328 ) ) ;
#14158 = DIRECTION ( 'NONE',  ( 1.000000000000000000, 0.000000000000000000, 0.000000000000000000 ) ) ;
#14159 = CARTESIAN_POINT ( 'NONE',  ( 172.7287565553229456, -4.999999999999971578, 0.5000000000000029976 ) ) ;
#14160 = EDGE_CURVE ( 'NONE', #27873, #23858, #5918, .T. ) ;
#14161 = CARTESIAN_POINT ( 'NONE',  ( 21.16681283796276603, -5.103637247178538061, -17.00692323485822754 ) ) ;
#14162 = VECTOR ( 'NONE', #5757, 1000.000000000000000 ) ;
#14163 = CARTESIAN_POINT ( 'NONE',  ( 142.0152310637605524, -1.999999999999978684, 1.702185954127501066 ) ) ;
#14164 = CARTESIAN_POINT ( 'NONE',  ( 15.45310053882616153, -5.000000000000013323, 47.55975312665928811 ) ) ;
#14165 = VECTOR ( 'NONE', #12616, 1000.000000000000000 ) ;
#14166 = DIRECTION ( 'NONE',  ( 1.000000000000000000, -0.000000000000000000, 0.000000000000000000 ) ) ;
#14167 = CARTESIAN_POINT ( 'NONE',  ( 149.7287565553230309, -1.999999999999975353, -33.82050807568879947 ) ) ;
#14168 = CARTESIAN_POINT ( 'NONE',  ( 10.47604570704546845, 16.43372961628045559, -17.33313991065496751 ) ) ;
#14169 = CARTESIAN_POINT ( 'NONE',  ( 35.54859390953724585, -22.18451583373416014, -17.78191007148576475 ) ) ;
#14170 = STYLED_ITEM ( 'NONE', ( #1922 ), #15681 ) ;
#14171 = DIRECTION ( 'NONE',  ( -0.9773680663943724589, -5.871577894680259423E-18, 0.2115458881484709175 ) ) ;
#14172 = CARTESIAN_POINT ( 'NONE',  ( 8.944584683310379702, 16.95159276115599667, -23.00000000000000711 ) ) ;
#14173 = ORIENTED_EDGE ( 'NONE', *, *, #22566, .F. ) ;
#14174 = CARTESIAN_POINT ( 'NONE',  ( 167.2287565553229456, -4.999999999999972466, -20.83012701892220164 ) ) ;
#14175 = CARTESIAN_POINT ( 'NONE',  ( 18.34549112274340033, 0.9605221043122941227, -13.99314825615798341 ) ) ;
#14176 = CARTESIAN_POINT ( 'NONE',  ( 11.27599706080618525, 16.67780739407118062, -16.78460567626121502 ) ) ;
#14177 = FACE_BOUND ( 'NONE', #6892, .T. ) ;
#14178 = ORIENTED_EDGE ( 'NONE', *, *, #10143, .F. ) ;
#14179 = EDGE_LOOP ( 'NONE', ( #5057, #27985, #13745, #4584 ) ) ;
#14180 = CARTESIAN_POINT ( 'NONE',  ( 9.641350829061996919, 17.66889105593114806, -17.91548090047172437 ) ) ;
#14181 = DIRECTION ( 'NONE',  ( -2.698458740408365879E-16, 1.000000000000000000, 0.000000000000000000 ) ) ;
#14182 = CARTESIAN_POINT ( 'NONE',  ( 9.898178882064430084, 16.49104486689975246, -16.51464960819000893 ) ) ;
#14183 = FACE_OUTER_BOUND ( 'NONE', #28031, .T. ) ;
#14184 = LINE ( 'NONE', #27831, #17890 ) ;
#14185 = VERTEX_POINT ( 'NONE', #10788 ) ;
#14186 = DIRECTION ( 'NONE',  ( -2.698458740408365879E-16, 1.000000000000000000, 0.000000000000000000 ) ) ;
#14187 = EDGE_LOOP ( 'NONE', ( #29079, #4627, #8572 ) ) ;
#14188 = CARTESIAN_POINT ( 'NONE',  ( 10.45680941692980959, 16.52194969480735764, -17.34528143170414083 ) ) ;
#14189 = VECTOR ( 'NONE', #3297, 1000.000000000000000 ) ;
#14190 = VERTEX_POINT ( 'NONE', #8036 ) ;
#14192 = CIRCLE ( 'NONE', #10301, 3.000000000000002665 ) ;
#14191 = CARTESIAN_POINT ( 'NONE',  ( 33.21349783521664278, -10.00660656636812007, -19.57461044683394746 ) ) ;
#14193 = CARTESIAN_POINT ( 'NONE',  ( 25.79824969357368047, -12.24460132778619226, -15.92960863319586906 ) ) ;
#14194 = CARTESIAN_POINT ( 'NONE',  ( 23.11440248821028831, -7.346120041196752659, -16.32852059634029018 ) ) ;
#14195 = ORIENTED_EDGE ( 'NONE', *, *, #25974, .T. ) ;
#14196 = ORIENTED_EDGE ( 'NONE', *, *, #5259, .F. ) ;
#14197 = DIRECTION ( 'NONE',  ( 1.000000000000000000, 0.000000000000000000, 0.000000000000000000 ) ) ;
#14198 = CARTESIAN_POINT ( 'NONE',  ( 33.49783966318349115, -10.45910432307822902, -18.51641766868578287 ) ) ;
#14199 = DIRECTION ( 'NONE',  ( -0.9793348277764708509, -0.2022456306178955776, 0.000000000000000000 ) ) ;
#14200 = EDGE_CURVE ( 'NONE', #13154, #4554, #3690, .T. ) ;
#14201 = EDGE_CURVE ( 'NONE', #6491, #184, #20729, .T. ) ;
#14202 = CARTESIAN_POINT ( 'NONE',  ( 19.26077778332419044, 5.765437233969479713, -18.81236659294151892 ) ) ;
#14203 = EDGE_CURVE ( 'NONE', #11438, #22675, #27315, .T. ) ;
#14204 = CARTESIAN_POINT ( 'NONE',  ( 14.93287775521291394, 9.378568215907955974, -14.88591063491414168 ) ) ;
#14205 = EDGE_CURVE ( 'NONE', #24876, #22090, #22550, .T. ) ;
#14206 = ORIENTED_EDGE ( 'NONE', *, *, #3604, .F. ) ;
#14207 = FACE_BOUND ( 'NONE', #1189, .T. ) ;
#14208 = DIRECTION ( 'NONE',  ( 0.9510565162951536422, 0.000000000000000000, -0.3090169943749475623 ) ) ;
#14209 = CARTESIAN_POINT ( 'NONE',  ( 143.6922820468854525, -10.00000000000000355, -32.39392330124607611 ) ) ;
#14210 = DIRECTION ( 'NONE',  ( 0.000000000000000000, 0.000000000000000000, 1.000000000000000000 ) ) ;
#14211 = CARTESIAN_POINT ( 'NONE',  ( 10.75323949831978432, 16.48238454209313630, -15.94078111022350619 ) ) ;
#14212 = DIRECTION ( 'NONE',  ( 1.000000000000000000, 1.280948979423041604E-16, -0.000000000000000000 ) ) ;
#14213 = ORIENTED_EDGE ( 'NONE', *, *, #16792, .F. ) ;
#14214 = LINE ( 'NONE', #14063, #3751 ) ;
#14215 = EDGE_LOOP ( 'NONE', ( #24994, #20536, #1292 ) ) ;
#14216 = CARTESIAN_POINT ( 'NONE',  ( 11.43229926783177497, 9.455373222906182207, -15.87769231223556332 ) ) ;
#14217 = CARTESIAN_POINT ( 'NONE',  ( 10.57561133056755942, 12.06435231892607618, -17.50969232694400546 ) ) ;
#14218 = CARTESIAN_POINT ( 'NONE',  ( 20.59810038911313157, 5.339108984243529754, -18.13170489685289510 ) ) ;
#14219 = CARTESIAN_POINT ( 'NONE',  ( -1.318516776095816523, -3.857556137907101501, -2.449999999999979305 ) ) ;
#14220 = CARTESIAN_POINT ( 'NONE',  ( -24.00000000000017053, 34.64101615137744972, 9.999999999999998224 ) ) ;
#14221 = CARTESIAN_POINT ( 'NONE',  ( 25.90632082398269276, -12.28056132945115841, -15.12647891527467969 ) ) ;
#14222 = DIRECTION ( 'NONE',  ( -0.8090169943749474513, -2.183098979609982436E-16, -0.5877852522924731371 ) ) ;
#14223 = CARTESIAN_POINT ( 'NONE',  ( 11.05541599318665469, 17.68942028772053376, -17.91303167831651422 ) ) ;
#14224 = VERTEX_POINT ( 'NONE', #24380 ) ;
#14225 = CARTESIAN_POINT ( 'NONE',  ( 35.39068211221506743, -20.47510177656754493, -19.23609803736608725 ) ) ;
#14226 = CARTESIAN_POINT ( 'NONE',  ( 9.486764522130870958, -5.000000000000015099, 29.19725899082042986 ) ) ;
#14227 = CARTESIAN_POINT ( 'NONE',  ( 132.2287565553230309, -4.999999999999982236, -20.83012701892220875 ) ) ;
#14228 = VECTOR ( 'NONE', #24393, 1000.000000000000000 ) ;
#14229 = CARTESIAN_POINT ( 'NONE',  ( 29.43474752111978177, -7.508961153211615169, -12.65842848261850229 ) ) ;
#14230 = ORIENTED_EDGE ( 'NONE', *, *, #29888, .T. ) ;
#14231 = LINE ( 'NONE', #21419, #9093 ) ;
#14232 =( LENGTH_UNIT ( ) NAMED_UNIT ( * ) SI_UNIT ( .MILLI., .METRE. ) );
#14233 = CARTESIAN_POINT ( 'NONE',  ( 22.61876936045522513, 2.364863857962155258, -15.74433402521326819 ) ) ;
#14234 = CARTESIAN_POINT ( 'NONE',  ( 16.22630451241072436, 4.170241327582352220, -17.06284370071109535 ) ) ;
#14235 = ADVANCED_FACE ( 'NONE', ( #8344 ), #13371, .F. ) ;
#14236 = EDGE_CURVE ( 'NONE', #4351, #8506, #17645, .T. ) ;
#14237 = ORIENTED_EDGE ( 'NONE', *, *, #26935, .F. ) ;
#14238 = ORIENTED_EDGE ( 'NONE', *, *, #23209, .T. ) ;
#14239 = DIRECTION ( 'NONE',  ( -0.9510565162951536422, -2.566386769018988323E-16, 0.3090169943749475623 ) ) ;
#14240 = VECTOR ( 'NONE', #3529, 1000.000000000000000 ) ;
#14241 = CARTESIAN_POINT ( 'NONE',  ( -2.000000000000026201, -3.464101615137764156, -2.450000000000000622 ) ) ;
#14242 = DIRECTION ( 'NONE',  ( 0.000000000000000000, 0.000000000000000000, -1.000000000000000000 ) ) ;
#14243 = LINE ( 'NONE', #21124, #26770 ) ;
#14244 = DIRECTION ( 'NONE',  ( 0.5877852522924731371, 1.586114251531760728E-16, -0.8090169943749474513 ) ) ;
#14245 = VECTOR ( 'NONE', #26019, 1000.000000000000000 ) ;
#14246 = CARTESIAN_POINT ( 'NONE',  ( 9.641485839925177714, 17.66827187890266160, -17.87200850766020110 ) ) ;
#14247 = CARTESIAN_POINT ( 'NONE',  ( 18.07093408371026300, -2.157424655934858215, -16.53044640867639359 ) ) ;
#14248 = CARTESIAN_POINT ( 'NONE',  ( 18.97628335640213493, 0.9430780577607489334, -14.77698032187241850 ) ) ;
#14250 = ORIENTED_EDGE ( 'NONE', *, *, #22240, .T. ) ;
#14249 = CARTESIAN_POINT ( 'NONE',  ( 36.54859390953724585, -23.18451583373416014, -17.64281456791166391 ) ) ;
#14251 = CARTESIAN_POINT ( 'NONE',  ( 49.00000000000000000, 0.000000000000000000, 0.000000000000000000 ) ) ;
#14252 = LINE ( 'NONE', #9833, #1505 ) ;
#14253 = CARTESIAN_POINT ( 'NONE',  ( 109.5403287000431192, -4.999999999999987566, -79.58570733226751770 ) ) ;
#14254 = CARTESIAN_POINT ( 'NONE',  ( 132.0152310637605524, -4.999999999999982236, -1.465663491281971624E-14 ) ) ;
#14255 = CARTESIAN_POINT ( 'NONE',  ( 18.76632379254337835, 6.868107169226369102, -19.55161205380106892 ) ) ;
#14256 = CARTESIAN_POINT ( 'NONE',  ( 141.1922820468854525, -1.999999999999978462, -19.40354224447947473 ) ) ;
#14257 = CARTESIAN_POINT ( 'NONE',  ( 10.33811689237846743, 18.38618972876440338, -17.91642382710546855 ) ) ;
#14258 = ORIENTED_EDGE ( 'NONE', *, *, #30196, .F. ) ;
#14259 = FACE_OUTER_BOUND ( 'NONE', #27387, .T. ) ;
#14260 = CARTESIAN_POINT ( 'NONE',  ( 154.7287565553229456, -4.999999999999976019, -7.839745962155600267 ) ) ;
#14261 = EDGE_CURVE ( 'NONE', #17616, #14597, #15506, .T. ) ;
#14262 = CARTESIAN_POINT ( 'NONE',  ( 16.09764958744793262, 8.143416238145906760, -19.84970969296679044 ) ) ;
#14263 = ORIENTED_EDGE ( 'NONE', *, *, #9572, .F. ) ;
#14264 = CARTESIAN_POINT ( 'NONE',  ( 12.86846089198198584, 5.826474397738612865, -17.89591831848172276 ) ) ;
#14265 = ORIENTED_EDGE ( 'NONE', *, *, #681, .F. ) ;
#14266 = CARTESIAN_POINT ( 'NONE',  ( 35.12509383387676820, -20.28195432802065312, -20.22992657050740917 ) ) ;
#14267 = CARTESIAN_POINT ( 'NONE',  ( 22.60936069168443652, -2.585520780102871896, -18.46111163327002913 ) ) ;
#14268 = EDGE_CURVE ( 'NONE', #12321, #11833, #6370, .T. ) ;
#14269 = CARTESIAN_POINT ( 'NONE',  ( 22.11273855634006935, 3.201273238686522138, -15.95510540678940181 ) ) ;
#14270 = EDGE_CURVE ( 'NONE', #23525, #26068, #1308, .T. ) ;
#14271 = VECTOR ( 'NONE', #14129, 1000.000000000000000 ) ;
#14272 = EDGE_CURVE ( 'NONE', #16967, #18308, #19630, .T. ) ;
#14273 = EDGE_CURVE ( 'NONE', #17474, #23715, #5763, .T. ) ;
#14274 = CARTESIAN_POINT ( 'NONE',  ( 25.16264305761801268, -10.69278474016982727, -17.18274900023375906 ) ) ;
#14275 = ORIENTED_EDGE ( 'NONE', *, *, #22417, .T. ) ;
#14276 = CARTESIAN_POINT ( 'NONE',  ( 143.6922820468853956, -1.999999999999978462, 2.247092850131519715 ) ) ;
#14278 = ORIENTED_EDGE ( 'NONE', *, *, #14859, .F. ) ;
#14277 = CARTESIAN_POINT ( 'NONE',  ( 152.0152310637604671, -10.00000000000000178, -17.38167787843870826 ) ) ;
#14279 = DIRECTION ( 'NONE',  ( 0.000000000000000000, 0.000000000000000000, -1.000000000000000000 ) ) ;
#14280 = CARTESIAN_POINT ( 'NONE',  ( 149.7287565553229456, -1.999999999999976685, 0.8205080756887930260 ) ) ;
#14281 = CARTESIAN_POINT ( 'NONE',  ( 36.25073006198487491, -19.84637134955221072, -19.45760515208133512 ) ) ;
#14282 = CARTESIAN_POINT ( 'NONE',  ( 12.75684812230466925, 7.626178201396932366, -14.92546252573342258 ) ) ;
#14283 = EDGE_LOOP ( 'NONE', ( #19426, #3230, #20558, #22734 ) ) ;
#14284 = FACE_OUTER_BOUND ( 'NONE', #8119, .T. ) ;
#14285 = CARTESIAN_POINT ( 'NONE',  ( 156.1922820468854241, -1.999999999999974909, -28.06379628232387446 ) ) ;
#14286 = CARTESIAN_POINT ( 'NONE',  ( 12.02817646543008934, 9.315460371489308500, -16.69127922251917795 ) ) ;
#14287 = DIRECTION ( 'NONE',  ( 1.000000000000000000, 2.698458740408365879E-16, -1.110223024625156540E-16 ) ) ;
#14288 = DIRECTION ( 'NONE',  ( -1.000000000000000000, 0.000000000000000000, 0.000000000000000000 ) ) ;
#14289 = EDGE_LOOP ( 'NONE', ( #27883, #14927, #24595, #4582 ) ) ;
#14290 = CARTESIAN_POINT ( 'NONE',  ( 21.01610262522592976, -5.000000000000011546, -64.68091306524351580 ) ) ;
#14291 = EDGE_LOOP ( 'NONE', ( #28463, #3535, #21819, #651 ) ) ;
#14292 = EDGE_LOOP ( 'NONE', ( #9381, #4379 ) ) ;
#14293 = CARTESIAN_POINT ( 'NONE',  ( 164.7287565553228887, -9.999999999999998224, -7.839745962155603820 ) ) ;
#14294 = VERTEX_POINT ( 'NONE', #25133 ) ;
#14295 = EDGE_LOOP ( 'NONE', ( #8641, #28965, #7722, #1577 ) ) ;
#14296 = DIRECTION ( 'NONE',  ( 1.000000000000000000, 2.698458740408365879E-16, 0.000000000000000000 ) ) ;
#14297 = ORIENTED_EDGE ( 'NONE', *, *, #817, .F. ) ;
#14298 = B_SPLINE_CURVE_WITH_KNOTS ( 'NONE', 3,
 ( #14840, #3421, #17294, #28948, #24177, #1138 ),
 .UNSPECIFIED., .F., .F.,
 ( 4, 2, 4 ),
 ( 2.380731629704013595E-07, 0.002336973833157559872, 0.004673709593152148775 ),
 .UNSPECIFIED. ) ;
#14299 = CARTESIAN_POINT ( 'NONE',  ( 9.667670487869566287, 16.22828475907693146, -17.88517164372263579 ) ) ;
#14300 = CARTESIAN_POINT ( 'NONE',  ( 25.68863286643039601, -3.692565893519352827, -17.49701707463368550 ) ) ;
#14301 = CARTESIAN_POINT ( 'NONE',  ( 20.49605984403359216, -1.259233478192978373, -14.44550164344372511 ) ) ;
#14302 = LINE ( 'NONE', #16610, #6270 ) ;
#14303 = DIRECTION ( 'NONE',  ( 0.000000000000000000, 0.000000000000000000, 1.000000000000000000 ) ) ;
#14304 = CARTESIAN_POINT ( 'NONE',  ( 149.5152310637606092, -10.00000000000000178, -28.60870317832789667 ) ) ;
#14305 = ADVANCED_FACE ( 'NONE', ( #15956, #25283, #4521 ), #16256, .T. ) ;
#14306 = CARTESIAN_POINT ( 'NONE',  ( 24.95482030053459965, -6.624749414579512496, -13.76522253407564733 ) ) ;
#14307 = VECTOR ( 'NONE', #5330, 1000.000000000000000 ) ;
#14308 = DIRECTION ( 'NONE',  ( -1.000000000000000000, -4.440892098500622217E-16, 0.000000000000000000 ) ) ;
#14309 = LINE ( 'NONE', #5017, #17180 ) ;
#14310 = PLANE ( 'NONE',  #27296 ) ;
#14311 = DIRECTION ( 'NONE',  ( -0.5877852522924731371, -1.586114251531760728E-16, -0.8090169943749474513 ) ) ;
#14312 = CARTESIAN_POINT ( 'NONE',  ( 172.0152310637604387, -4.999999999999970690, -1.909752701132032978E-14 ) ) ;
#14313 = CARTESIAN_POINT ( 'NONE',  ( 10.47230989469697882, 16.45086252791593751, -17.33468480047602256 ) ) ;
#14314 = DIRECTION ( 'NONE',  ( -2.698458740408365879E-16, 1.000000000000000000, 0.000000000000000000 ) ) ;
#14315 = CARTESIAN_POINT ( 'NONE',  ( 34.54007435814109783, -17.65377171698271752, -20.05309729467257540 ) ) ;
#14316 = ORIENTED_EDGE ( 'NONE', *, *, #20037, .F. ) ;
#14317 = CARTESIAN_POINT ( 'NONE',  ( 8.944589832665828411, 16.95156914555548866, -17.90909639166975609 ) ) ;
#14318 = VERTEX_POINT ( 'NONE', #7109 ) ;
#14319 = DIRECTION ( 'NONE',  ( 1.000000000000000000, 0.000000000000000000, -0.000000000000000000 ) ) ;
#14320 = CARTESIAN_POINT ( 'NONE',  ( 20.24985932600369409, 3.694099309552050237, -20.13309853732883781 ) ) ;
#14321 = CARTESIAN_POINT ( 'NONE',  ( 12.83021228909557010, 9.549978240774745331, -16.14188291223562288 ) ) ;
#14322 = CARTESIAN_POINT ( 'NONE',  ( 175.7287565553229456, -4.999999999999970690, 3.500000000000003109 ) ) ;
#14323 = ORIENTED_EDGE ( 'NONE', *, *, #16704, .F. ) ;
#14324 = EDGE_CURVE ( 'NONE', #22052, #18123, #4223, .T. ) ;
#14325 = EDGE_LOOP ( 'NONE', ( #28357, #15082, #8857, #5206, #14538 ) ) ;
#14326 = CARTESIAN_POINT ( 'NONE',  ( 9.641350810849047548, 17.66889113945805789, -17.92279151347709032 ) ) ;
#14327 = CARTESIAN_POINT ( 'NONE',  ( 0.000000000000000000, 0.000000000000000000, -15.00000000000000000 ) ) ;
#14328 = AXIS2_PLACEMENT_3D ( 'NONE', #29457, #19764, #29289 ) ;
#14329 = CARTESIAN_POINT ( 'NONE',  ( 9.932908820165812003, 16.33176894372950727, -16.49774300651844072 ) ) ;
#14330 = DIRECTION ( 'NONE',  ( -2.698458740408365879E-16, 1.000000000000000000, 0.000000000000000000 ) ) ;
#14331 = ORIENTED_EDGE ( 'NONE', *, *, #16759, .F. ) ;
#14332 = CARTESIAN_POINT ( 'NONE',  ( 8.000000000000003553, 4.618802153517037823, -0.7145311798163362926 ) ) ;
#14333 = ORIENTED_EDGE ( 'NONE', *, *, #15334, .F. ) ;
#14334 = CARTESIAN_POINT ( 'NONE',  ( 10.35900481074863322, 16.97049408594186914, -17.87076805301065363 ) ) ;
#14335 = ORIENTED_EDGE ( 'NONE', *, *, #13962, .T. ) ;
#14336 = CARTESIAN_POINT ( 'NONE',  ( 34.03885009341546208, -11.93819216554969742, -20.85700406890413916 ) ) ;
#14337 = CARTESIAN_POINT ( 'NONE',  ( 24.60501232743784783, -9.531698448777172317, -16.22453333552994792 ) ) ;
#14338 = CARTESIAN_POINT ( 'NONE',  ( 13.73972855572809060, 6.741564148929986011, -15.48174541850189811 ) ) ;
#14339 = ORIENTED_EDGE ( 'NONE', *, *, #21790, .T. ) ;
#14340 = LINE ( 'NONE', #634, #18895 ) ;
#14341 = ADVANCED_FACE ( 'NONE', ( #27910 ), #6969, .T. ) ;
#14342 = CARTESIAN_POINT ( 'NONE',  ( 34.70514358766799745, -13.90287004036446739, -20.03273298744158737 ) ) ;
#14343 = CARTESIAN_POINT ( 'NONE',  ( 18.31728471214517029, 9.901174664208697962, -15.18855771585127634 ) ) ;
#14344 = CARTESIAN_POINT ( 'NONE',  ( 28.95742876386502118, -9.428754790923060014, -17.52548735455339823 ) ) ;
#14345 = EDGE_LOOP ( 'NONE', ( #7192, #736, #4433, #17424 ) ) ;
#14346 = ORIENTED_EDGE ( 'NONE', *, *, #7599, .F. ) ;
#14347 = FACE_BOUND ( 'NONE', #14635, .T. ) ;
#14348 = VECTOR ( 'NONE', #12714, 1000.000000000000000 ) ;
#14349 = ORIENTED_EDGE ( 'NONE', *, *, #19614, .F. ) ;
#14350 = LINE ( 'NONE', #7804, #11573 ) ;
#14351 = LINE ( 'NONE', #14508, #4761 ) ;
#14352 = PLANE ( 'NONE',  #3379 ) ;
#14353 = CARTESIAN_POINT ( 'NONE',  ( 169.7287565553228603, -1.999999999999971356, 0.8205080756887930260 ) ) ;
#14354 = UNCERTAINTY_MEASURE_WITH_UNIT (LENGTH_MEASURE( 1.000000000000000082E-05 ), #8465, 'distance_accuracy_value', 'NONE');
#14355 = CARTESIAN_POINT ( 'NONE',  ( 10.71981169803933120, 16.63568869523268390, -15.95461020916288675 ) ) ;
#14356 = FACE_OUTER_BOUND ( 'NONE', #9603, .T. ) ;
#14357 = EDGE_CURVE ( 'NONE', #25113, #6635, #29925, .T. ) ;
#14358 = EDGE_CURVE ( 'NONE', #11977, #20122, #20385, .T. ) ;
#14359 = EDGE_CURVE ( 'NONE', #27706, #25494, #18827, .T. ) ;
#14360 = CARTESIAN_POINT ( 'NONE',  ( 3.318518101603024295, 7.321656987762882096, -4.304621437946355112E-15 ) ) ;
#14361 = ORIENTED_EDGE ( 'NONE', *, *, #18156, .T. ) ;
#14362 = CARTESIAN_POINT ( 'NONE',  ( 9.916824447075894611, 16.40553392900050156, -16.50439446175997205 ) ) ;
#14363 = EDGE_CURVE ( 'NONE', #24692, #3985, #13673, .T. ) ;
#14364 = VERTEX_POINT ( 'NONE', #2247 ) ;
#14365 = CARTESIAN_POINT ( 'NONE',  ( 9.667864356596815867, 16.22739565238121529, -17.88507765419223716 ) ) ;
#14366 = CARTESIAN_POINT ( 'NONE',  ( 22.85609869791697335, 3.752015377681134467, -15.55886478590537969 ) ) ;
#14367 = DIRECTION ( 'NONE',  ( 0.9510565162951536422, 0.000000000000000000, -0.3090169943749475623 ) ) ;
#14368 = CARTESIAN_POINT ( 'NONE',  ( 27.95388715220626707, -5.541385876428546631, -15.41148221666858831 ) ) ;
#14369 = PLANE ( 'NONE',  #15423 ) ;
#14370 = CARTESIAN_POINT ( 'NONE',  ( 11.27738072919014911, 16.67146171448561276, -16.78403338633166442 ) ) ;
#14371 = EDGE_LOOP ( 'NONE', ( #6934, #10000, #27924, #11905 ) ) ;
#14372 = CARTESIAN_POINT ( 'NONE',  ( 33.80310782676656345, -13.34297147354166135, -18.78800844379110302 ) ) ;
#14373 = CARTESIAN_POINT ( 'NONE',  ( 17.29421355564066332, 9.360779442694735053, -19.18964209290773937 ) ) ;
#14374 = VECTOR ( 'NONE', #27968, 1000.000000000000114 ) ;
#14375 = LINE ( 'NONE', #23712, #13973 ) ;
#14376 = CARTESIAN_POINT ( 'NONE',  ( 9.008298112641352162, 16.65939485267133335, -17.25320607661530303 ) ) ;
#14377 = CARTESIAN_POINT ( 'NONE',  ( 24.24063474714532873, -9.755679120534059834, -13.19378374426895206 ) ) ;
#14378 = ORIENTED_EDGE ( 'NONE', *, *, #20647, .F. ) ;
#14379 = CARTESIAN_POINT ( 'NONE',  ( 172.7287565553229456, -4.999999999999970690, -33.50000000000000000 ) ) ;
#14380 = EDGE_LOOP ( 'NONE', ( #25980, #23154, #1716, #11602 ) ) ;
#14381 = CARTESIAN_POINT ( 'NONE',  ( 16.29141254853644227, 2.771581735061156682, -15.76764191790683611 ) ) ;
#14382 = CARTESIAN_POINT ( 'NONE',  ( 14.03260640687251204, 7.914523597318124715, -15.18742456358547521 ) ) ;
#14383 = DIRECTION ( 'NONE',  ( -0.000000000000000000, -0.000000000000000000, -1.000000000000000000 ) ) ;
#14384 = EDGE_LOOP ( 'NONE', ( #4749, #8832, #7979, #14206 ) ) ;
#14385 = VECTOR ( 'NONE', #247, 1000.000000000000000 ) ;
#14386 = DIRECTION ( 'NONE',  ( -1.110223024625156540E-16, 0.000000000000000000, -1.000000000000000000 ) ) ;
#14387 = CARTESIAN_POINT ( 'NONE',  ( 132.0152310637605524, -1.999999999999981348, -26.04193191628310800 ) ) ;
#14388 = ADVANCED_FACE ( 'NONE', ( #20990 ), #23289, .T. ) ;
#14389 = DIRECTION ( 'NONE',  ( -1.000000000000000000, -4.440892098500622217E-16, 0.000000000000000000 ) ) ;
#14390 = LINE ( 'NONE', #18993, #13578 ) ;
#14391 = AXIS2_PLACEMENT_3D ( 'NONE', #16893, #21475, #26226 ) ;
#14392 = DIRECTION ( 'NONE',  ( -1.000000000000000000, 0.000000000000000000, 0.000000000000000000 ) ) ;
#14393 = AXIS2_PLACEMENT_3D ( 'NONE', #20086, #13060, #15497 ) ;
#14394 = CARTESIAN_POINT ( 'NONE',  ( 9.916336358462064737, 16.40777236560037622, -16.50459729666445696 ) ) ;
#14395 = CARTESIAN_POINT ( 'NONE',  ( 27.79246359028025992, -7.761574269410560944, -18.12988733074048753 ) ) ;
#14396 = CARTESIAN_POINT ( 'NONE',  ( 20.61437924707763258, -4.384239709691692966, -16.09784705243023240 ) ) ;
#14397 = EDGE_CURVE ( 'NONE', #18151, #2772, #18101, .T. ) ;
#14399 = ORIENTED_EDGE ( 'NONE', *, *, #8792, .F. ) ;
#14398 = CARTESIAN_POINT ( 'NONE',  ( 33.26197456417788345, -12.91194637099222575, -20.70907993653955970 ) ) ;
#14400 = DIRECTION ( 'NONE',  ( 0.3090169943749472292, 8.338696094057992503E-17, -0.9510565162951536422 ) ) ;
#14401 = CARTESIAN_POINT ( 'NONE',  ( 12.50906579366657390, 8.574708520419219937, -15.12294941509656354 ) ) ;
#14402 = EDGE_CURVE ( 'NONE', #14895, #2921, #1952, .T. ) ;
#14403 = CARTESIAN_POINT ( 'NONE',  ( 132.0152310637605808, -10.00000000000000711, 1.702185954127501066 ) ) ;
#14404 = LINE ( 'NONE', #17017, #14385 ) ;
#14405 = EDGE_CURVE ( 'NONE', #16007, #18100, #11085, .T. ) ;
#14406 = CARTESIAN_POINT ( 'NONE',  ( 18.47369133221681281, 7.987600538477567014, -15.27093437040897861 ) ) ;
#14407 = VERTEX_POINT ( 'NONE', #20833 ) ;
#14408 = DIRECTION ( 'NONE',  ( 0.000000000000000000, 0.000000000000000000, -1.000000000000000000 ) ) ;
#14409 = CARTESIAN_POINT ( 'NONE',  ( 10.34111691064986438, 18.37243126255838988, -17.67295385331717483 ) ) ;
#14410 = PLANE ( 'NONE',  #11019 ) ;
#14411 = LINE ( 'NONE', #23592, #78 ) ;
#14412 = VECTOR ( 'NONE', #21027, 1000.000000000000000 ) ;
#14413 = CARTESIAN_POINT ( 'NONE',  ( 18.76632379254337835, 6.868107169226369102, -19.55161205380106892 ) ) ;
#14414 = CARTESIAN_POINT ( 'NONE',  ( 15.52843720209238931, 6.760224976758691717, -13.32525641785786696 ) ) ;
#14415 = VERTEX_POINT ( 'NONE', #18709 ) ;
#14416 = CARTESIAN_POINT ( 'NONE',  ( 32.96569147872224903, -11.36116021242123608, -19.12347989294568151 ) ) ;
#14417 = CARTESIAN_POINT ( 'NONE',  ( 23.38119176934044674, -2.968156504308268495, -14.25447959695224043 ) ) ;
#14418 = AXIS2_PLACEMENT_3D ( 'NONE', #5577, #14858, #26965 ) ;
#14419 = CARTESIAN_POINT ( 'NONE',  ( 17.99585798733817299, 1.806717527199089401, -17.78491074480216838 ) ) ;
#14420 = VECTOR ( 'NONE', #26742, 1000.000000000000000 ) ;
#14421 = ORIENTED_EDGE ( 'NONE', *, *, #14816, .T. ) ;
#14422 = CARTESIAN_POINT ( 'NONE',  ( 27.32970014129078962, -12.32490512882196754, -16.69500413328365696 ) ) ;
#14423 = ORIENTED_EDGE ( 'NONE', *, *, #28249, .F. ) ;
#14424 = CARTESIAN_POINT ( 'NONE',  ( 143.6922820468854525, -10.00000000000000355, -32.39392330124607611 ) ) ;
#14426 = EDGE_LOOP ( 'NONE', ( #24173, #28124, #21912 ) ) ;
#14425 = DIRECTION ( 'NONE',  ( -0.5877852522924731371, -1.586114251531760728E-16, -0.8090169943749474513 ) ) ;
#14427 = DIRECTION ( 'NONE',  ( 0.9510565162951535312, 2.566386769018988816E-16, -0.3090169943749475623 ) ) ;
#14428 = VECTOR ( 'NONE', #9685, 1000.000000000000000 ) ;
#14429 = ORIENTED_EDGE ( 'NONE', *, *, #19896, .F. ) ;
#14430 = DIRECTION ( 'NONE',  ( -0.8090169943749474513, -2.183098979609982436E-16, 0.5877852522924731371 ) ) ;
#14431 = CARTESIAN_POINT ( 'NONE',  ( 34.59231264378541937, -12.39598037772099559, -18.95630535174095499 ) ) ;
#14432 = VECTOR ( 'NONE', #29581, 1000.000000000000000 ) ;
#14433 = CARTESIAN_POINT ( 'NONE',  ( 9.641384570184822422, 17.66873631484086715, -17.89388817125738385 ) ) ;
#14434 = ORIENTED_EDGE ( 'NONE', *, *, #28068, .T. ) ;
#14435 = EDGE_CURVE ( 'NONE', #10636, #28125, #8931, .T. ) ;
#14436 = VECTOR ( 'NONE', #7066, 1000.000000000000000 ) ;
#14437 = CARTESIAN_POINT ( 'NONE',  ( 162.0152310637604387, -4.999999999999973355, 1.702185954127501066 ) ) ;
#14438 = DIRECTION ( 'NONE',  ( 0.9510565162951535312, 2.566386769018988816E-16, -0.3090169943749475623 ) ) ;
#14439 = EDGE_CURVE ( 'NONE', #11101, #3398, #28055, .T. ) ;
#14440 = EDGE_CURVE ( 'NONE', #28379, #26554, #29776, .T. ) ;
#14441 = CARTESIAN_POINT ( 'NONE',  ( 12.02799090998256304, 9.316311091778235465, -16.69135597610317134 ) ) ;
#14442 = CARTESIAN_POINT ( 'NONE',  ( 2.500000000000000444, 0.000000000000000000, 0.000000000000000000 ) ) ;
#14443 = EDGE_CURVE ( 'NONE', #1194, #8663, #11378, .T. ) ;
#14444 = DIRECTION ( 'NONE',  ( 0.000000000000000000, 0.000000000000000000, -1.000000000000000000 ) ) ;
#14445 = EDGE_LOOP ( 'NONE', ( #9763, #14275, #9334, #10600, #25809, #21401 ) ) ;
#14446 = DIRECTION ( 'NONE',  ( 0.000000000000000000, 0.000000000000000000, 1.000000000000000000 ) ) ;
#14447 = ORIENTED_EDGE ( 'NONE', *, *, #18518, .F. ) ;
#14448 = DIRECTION ( 'NONE',  ( 1.110223024625156540E-16, 2.995891024602366092E-32, 1.000000000000000000 ) ) ;
#14449 = ORIENTED_EDGE ( 'NONE', *, *, #5603, .T. ) ;
#14450 = PLANE ( 'NONE',  #15946 ) ;
#14451 = ORIENTED_EDGE ( 'NONE', *, *, #22977, .F. ) ;
#14452 = CARTESIAN_POINT ( 'NONE',  ( 12.48979292151040177, 7.561326536588189207, -16.39201226339353212 ) ) ;
#14453 = CARTESIAN_POINT ( 'NONE',  ( 25.85400256215867643, -3.413040292952954413, -16.90843739280879277 ) ) ;
#14454 = CARTESIAN_POINT ( 'NONE',  ( 26.84208138670940968, -2.489200896322508516, -17.35162900556907317 ) ) ;
#14455 = VECTOR ( 'NONE', #6487, 1000.000000000000000 ) ;
#14456 = FACE_OUTER_BOUND ( 'NONE', #19260, .T. ) ;
#14457 = CARTESIAN_POINT ( 'NONE',  ( 152.2287565553229740, -1.999999999999975353, -12.16987298107780369 ) ) ;
#14458 = DIRECTION ( 'NONE',  ( -0.5877852522924731371, 0.000000000000000000, 0.8090169943749474513 ) ) ;
#14459 = CIRCLE ( 'NONE', #18372, 5.999999999999977796 ) ;
#14460 = VECTOR ( 'NONE', #8182, 1000.000000000000000 ) ;
#14461 = EDGE_LOOP ( 'NONE', ( #28248, #17522, #5497, #29077 ) ) ;
#14462 = CARTESIAN_POINT ( 'NONE',  ( 162.0152310637604955, -1.999999999999972244, -26.04193191628311155 ) ) ;
#14463 = FACE_OUTER_BOUND ( 'NONE', #28518, .T. ) ;
#14464 = VECTOR ( 'NONE', #10576, 1000.000000000000000 ) ;
#14465 = ORIENTED_EDGE ( 'NONE', *, *, #27246, .F. ) ;
#14466 = LINE ( 'NONE', #7171, #8304 ) ;
#14467 = CARTESIAN_POINT ( 'NONE',  ( 157.2287565553229172, -1.999999999999974465, -3.509618943233403510 ) ) ;
#14468 = CARTESIAN_POINT ( 'NONE',  ( 10.99070134719017311, 14.07345324724201063, -17.12031169937328201 ) ) ;
#14469 = FACE_OUTER_BOUND ( 'NONE', #28613, .T. ) ;
#14470 = CARTESIAN_POINT ( 'NONE',  ( 32.58918748260075660, -11.04229556371213583, -18.21152344180378080 ) ) ;
#14471 = VERTEX_POINT ( 'NONE', #9078 ) ;
#14472 = CARTESIAN_POINT ( 'NONE',  ( 8.944585005148796952, 16.95159128516397118, -17.91410349795882340 ) ) ;
#14473 = EDGE_CURVE ( 'NONE', #23755, #2694, #18405, .T. ) ;
#14474 = DIRECTION ( 'NONE',  ( -0.5877852522924731371, -1.586114251531760235E-16, 0.8090169943749474513 ) ) ;
#14475 = VECTOR ( 'NONE', #3847, 1000.000000000000000 ) ;
#14476 = CARTESIAN_POINT ( 'NONE',  ( 17.36512755686010934, 0.5347363583120325892, -15.24149349723765390 ) ) ;
#14477 = EDGE_CURVE ( 'NONE', #13095, #9877, #25432, .T. ) ;
#14478 = CARTESIAN_POINT ( 'NONE',  ( 12.83866652039362855, 9.525916288823983891, -16.13726486007240624 ) ) ;
#14479 = CARTESIAN_POINT ( 'NONE',  ( 152.2287565553230309, -4.999999999999976019, -29.49038105676660848 ) ) ;
#14480 = EDGE_CURVE ( 'NONE', #24310, #23025, #22223, .T. ) ;
#14481 = ORIENTED_EDGE ( 'NONE', *, *, #28067, .T. ) ;
#14482 = CIRCLE ( 'NONE', #7683, 4.000000000000003553 ) ;
#14483 = CARTESIAN_POINT ( 'NONE',  ( 11.65548303173490652, 8.849831895876286936, -15.75351705932409985 ) ) ;
#14484 = CARTESIAN_POINT ( 'NONE',  ( 104.1536536346199426, -4.999999999999989342, -75.67205881269151746 ) ) ;
#14485 = CARTESIAN_POINT ( 'NONE',  ( 11.21346931060482000, 10.45895530107994098, -15.96818619734747458 ) ) ;
#14486 = DIRECTION ( 'NONE',  ( 0.3090169943749475623, 8.338696094058001131E-17, 0.9510565162951536422 ) ) ;
#14487 = ORIENTED_EDGE ( 'NONE', *, *, #234, .F. ) ;
#14488 = CARTESIAN_POINT ( 'NONE',  ( -24.99999999999999289, 55.00000000000000711, -30.00000000000000711 ) ) ;
#14489 = ORIENTED_EDGE ( 'NONE', *, *, #25176, .F. ) ;
#14490 = CARTESIAN_POINT ( 'NONE',  ( 12.01798642417223739, 9.362192935812041483, -16.69549318315592856 ) ) ;
#14491 = ORIENTED_EDGE ( 'NONE', *, *, #28246, .F. ) ;
#14492 = CIRCLE ( 'NONE', #28192, 4.188000000000025480 ) ;
#14493 = CARTESIAN_POINT ( 'NONE',  ( 36.54222296954648641, -22.15589457513855010, -18.69601260479128513 ) ) ;
#14494 = CARTESIAN_POINT ( 'NONE',  ( 16.83828815103352028, 11.11029360287396983, -16.41243972054167344 ) ) ;
#14495 = CARTESIAN_POINT ( 'NONE',  ( 29.66490191837812773, -8.365349891895018430, -17.62461620872172574 ) ) ;
#14496 = ORIENTED_EDGE ( 'NONE', *, *, #29567, .F. ) ;
#14497 = LINE ( 'NONE', #12213, #3321 ) ;
#14498 = CARTESIAN_POINT ( 'NONE',  ( 34.27125395597954594, -11.98684039141630819, -19.88226891060491752 ) ) ;
#14499 = APPLICATION_PROTOCOL_DEFINITION ( 'draft international standard', 'automotive_design', 1998, #9279 ) ;
#14500 = CARTESIAN_POINT ( 'NONE',  ( 20.25556019283287768, 3.967930604842117681, -18.44304694949289569 ) ) ;
#14501 = CARTESIAN_POINT ( 'NONE',  ( 28.61166709039449785, -6.781025521995295513, -16.93684798036101213 ) ) ;
#14502 = VECTOR ( 'NONE', #15547, 1000.000000000000000 ) ;
#14503 = CARTESIAN_POINT ( 'NONE',  ( 132.0152310637605808, -10.00000000000000711, -6.958068083716893781 ) ) ;
#14504 = ADVANCED_FACE ( 'NONE', ( #9986 ), #14410, .T. ) ;
#14505 = DIRECTION ( 'NONE',  ( 0.5877852522924731371, 0.000000000000000000, 0.8090169943749474513 ) ) ;
#14506 = VECTOR ( 'NONE', #13603, 1000.000000000000000 ) ;
#14507 = CARTESIAN_POINT ( 'NONE',  ( 166.1922820468853388, -4.999999999999973355, -10.74328820663507678 ) ) ;
#14508 = CARTESIAN_POINT ( 'NONE',  ( 75.37105117200049165, -4.999999999999997335, 54.76027405692665440 ) ) ;
#14509 = CARTESIAN_POINT ( 'NONE',  ( 174.5152310637603819, -1.999999999999970024, -4.391296821672111328 ) ) ;
#14510 = LINE ( 'NONE', #9785, #9496 ) ;
#14511 = CARTESIAN_POINT ( 'NONE',  ( 12.25326555804286421, 9.517817489571868350, -15.32696995758615621 ) ) ;
#14512 = CARTESIAN_POINT ( 'NONE',  ( 141.1922820468854525, -1.999999999999978684, -22.25671179336495697 ) ) ;
#14513 = LINE ( 'NONE', #19108, #24710 ) ;
#14514 = VERTEX_POINT ( 'NONE', #23591 ) ;
#14515 = CARTESIAN_POINT ( 'NONE',  ( 12.50035968906703765, 8.570861208087439564, -15.12988832871674560 ) ) ;
#14516 = EDGE_LOOP ( 'NONE', ( #15151, #28608, #3473, #10425, #21044 ) ) ;
#14517 = AXIS2_PLACEMENT_3D ( 'NONE', #10911, #1933, #20368 ) ;
#14518 = CARTESIAN_POINT ( 'NONE',  ( 18.16797961131436523, 4.950584380424773556, -14.83967967756414730 ) ) ;
#14519 = CARTESIAN_POINT ( 'NONE',  ( 161.1922820468853956, -9.999999999999998224, -30.91696583120936026 ) ) ;
#14520 = LINE ( 'NONE', #12240, #20800 ) ;
#14521 = DIRECTION ( 'NONE',  ( -2.698458740408365879E-16, 1.000000000000000000, 0.000000000000000000 ) ) ;
#14522 = VERTEX_POINT ( 'NONE', #10139 ) ;
#14523 = CARTESIAN_POINT ( 'NONE',  ( 130.7287565553229172, -4.999999999999983125, -33.50000000000000000 ) ) ;
#14524 = CARTESIAN_POINT ( 'NONE',  ( 11.06643561541932463, 17.63888289548684796, -17.56974948598543662 ) ) ;
#14525 = ORIENTED_EDGE ( 'NONE', *, *, #14542, .T. ) ;
#14526 = AXIS2_PLACEMENT_3D ( 'NONE', #1542, #23044, #15554 ) ;
#14527 = CARTESIAN_POINT ( 'NONE',  ( 35.54824714876834690, -21.18295802128256611, -18.40066978570660083 ) ) ;
#14528 = CARTESIAN_POINT ( 'NONE',  ( 18.55171814111300321, 6.637122934506423988, -19.73184648383247364 ) ) ;
#14529 = CARTESIAN_POINT ( 'NONE',  ( 152.2287565553230024, -1.999999999999974909, -20.83012701892220520 ) ) ;
#14530 = CARTESIAN_POINT ( 'NONE',  ( 9.109039160554445402, 16.19738356544468516, -17.05632368146133615 ) ) ;
#14531 = CARTESIAN_POINT ( 'NONE',  ( 28.15806058933612022, -5.108324757233392077, -18.51472486207664758 ) ) ;
#14532 = ORIENTED_EDGE ( 'NONE', *, *, #8919, .T. ) ;
#14533 = AXIS2_PLACEMENT_3D ( 'NONE', #17507, #26861, #8197 ) ;
#14534 = DIRECTION ( 'NONE',  ( 1.000000000000000000, 2.891205793294675861E-16, 0.000000000000000000 ) ) ;
#14535 = CARTESIAN_POINT ( 'NONE',  ( 22.75707610144304383, -3.504958924507949991, -13.40925247317622571 ) ) ;
#14536 = CARTESIAN_POINT ( 'NONE',  ( 16.71823672545656336, 7.456161109308904855, -19.47106720222115683 ) ) ;
#14537 = DIRECTION ( 'NONE',  ( -2.698458740408365879E-16, 1.000000000000000000, 0.000000000000000000 ) ) ;
#14538 = ORIENTED_EDGE ( 'NONE', *, *, #18943, .T. ) ;
#14539 = ORIENTED_EDGE ( 'NONE', *, *, #21862, .F. ) ;
#14540 = EDGE_CURVE ( 'NONE', #1338, #24750, #26347, .T. ) ;
#14541 = CARTESIAN_POINT ( 'NONE',  ( 132.2287565553230024, -1.999999999999981348, -29.49038105676660138 ) ) ;
#14542 = EDGE_CURVE ( 'NONE', #8702, #14190, #850, .T. ) ;
#14543 = DIRECTION ( 'NONE',  ( 0.3090169943749475623, 8.338696094058001131E-17, 0.9510565162951536422 ) ) ;
#14544 = DIRECTION ( 'NONE',  ( 1.000000000000000000, 2.698458740408365879E-16, -1.110223024625156540E-16 ) ) ;
#14545 = PLANE ( 'NONE',  #26280 ) ;
#14546 = DIRECTION ( 'NONE',  ( 3.166185380091481561E-16, -0.7071067811865493491, 0.7071067811865456854 ) ) ;
#14547 = CARTESIAN_POINT ( 'NONE',  ( 11.21346931060482000, 10.45895530107994098, -15.96818619734747458 ) ) ;
#14548 = AXIS2_PLACEMENT_3D ( 'NONE', #26707, #14910, #3638 ) ;
#14549 = CARTESIAN_POINT ( 'NONE',  ( 27.46788175125265141, -10.83975311022233079, -17.61709057740623408 ) ) ;
#14550 = CARTESIAN_POINT ( 'NONE',  ( 23.39789874936200320, -0.01207823811560896493, -14.43595595811700782 ) ) ;
#14552 = ORIENTED_EDGE ( 'NONE', *, *, #14359, .T. ) ;
#14551 = CARTESIAN_POINT ( 'NONE',  ( 32.58918748260075660, -11.04229556371213583, -18.21152344180378080 ) ) ;
#14553 = DIRECTION ( 'NONE',  ( -2.698458740408366372E-16, 1.000000000000000000, 0.000000000000000000 ) ) ;
#14554 = DIRECTION ( 'NONE',  ( -2.698458740408365879E-16, 1.000000000000000000, 0.000000000000000000 ) ) ;
#14555 = CARTESIAN_POINT ( 'NONE',  ( 12.50162201464318557, 8.571418981294288031, -15.12888223836978341 ) ) ;
#14556 = CARTESIAN_POINT ( 'NONE',  ( -4.250000000000000000, -1.366904252225139372E-15, -4.449444346342715129 ) ) ;
#14557 = CARTESIAN_POINT ( 'NONE',  ( 0.000000000000000000, 55.00000000000000711, -23.00000000000000000 ) ) ;
#14558 = CARTESIAN_POINT ( 'NONE',  ( 20.50636976340433293, -0.9757509181830721356, -19.91080244439677571 ) ) ;
#14559 = VERTEX_POINT ( 'NONE', #23911 ) ;
#14560 = FACE_OUTER_BOUND ( 'NONE', #397, .T. ) ;
#14561 = CARTESIAN_POINT ( 'NONE',  ( 10.59516011209494302, 17.20735675775515361, -16.09619895116188815 ) ) ;
#14562 = CARTESIAN_POINT ( 'NONE',  ( -13.00000000000000178, 0.000000000000000000, -15.00000000000000000 ) ) ;
#14563 = LINE ( 'NONE', #28970, #4456 ) ;
#14564 = CARTESIAN_POINT ( 'NONE',  ( 22.86252235622482587, -0.9498377794471745128, -13.29674124224850118 ) ) ;
#14565 = CARTESIAN_POINT ( 'NONE',  ( 17.25718654270123409, 10.07213275844434364, -20.48022200034118612 ) ) ;
#14566 = ORIENTED_EDGE ( 'NONE', *, *, #442, .T. ) ;
#14567 = CARTESIAN_POINT ( 'NONE',  ( 32.58918748260075660, -11.04229556371213583, -18.21152344180378080 ) ) ;
#14568 = VECTOR ( 'NONE', #4762, 1000.000000000000000 ) ;
#14569 = CARTESIAN_POINT ( 'NONE',  ( 24.07691212630517796, -1.086650970500502300, -17.53382830850624785 ) ) ;
#14570 = CARTESIAN_POINT ( 'NONE',  ( 18.48843674521961589, -1.244547778534776938, -16.48413177534300900 ) ) ;
#14571 = VECTOR ( 'NONE', #16584, 1000.000000000000000 ) ;
#14572 = CARTESIAN_POINT ( 'NONE',  ( 25.85465836959373220, -10.01954208144345770, -18.53069695322523103 ) ) ;
#14573 = EDGE_CURVE ( 'NONE', #5728, #19562, #3006, .T. ) ;
#14574 = EDGE_CURVE ( 'NONE', #18591, #23239, #19156, .T. ) ;
#14575 = EDGE_CURVE ( 'NONE', #11550, #6495, #253, .T. ) ;
#14576 = EDGE_LOOP ( 'NONE', ( #14875, #26034, #29638, #16297 ) ) ;
#14577 = EDGE_CURVE ( 'NONE', #17358, #15701, #18853, .T. ) ;
#14578 = CARTESIAN_POINT ( 'NONE',  ( 95.11637572886448311, -4.999999999999991118, 69.10609207675695131 ) ) ;
#14580 = ORIENTED_EDGE ( 'NONE', *, *, #24076, .F. ) ;
#14579 = FILL_AREA_STYLE ('',( #5748 ) ) ;
#14581 = CARTESIAN_POINT ( 'NONE',  ( 130.7287565553229456, -9.999999999999982236, 0.5000000000000052180 ) ) ;
#14582 = FACE_OUTER_BOUND ( 'NONE', #14106, .T. ) ;
#14583 = CARTESIAN_POINT ( 'NONE',  ( 34.28781561389841670, -12.04879923890588422, -19.89451123369701691 ) ) ;
#14584 = CIRCLE ( 'NONE', #18014, 2.041999999999999815 ) ;
#14585 = CARTESIAN_POINT ( 'NONE',  ( 12.76278909782508997, 7.628803627606831839, -14.92072746316176790 ) ) ;
#14586 = DIRECTION ( 'NONE',  ( -0.8090169943749474513, -2.183098979609982436E-16, 0.5877852522924731371 ) ) ;
#14587 = LINE ( 'NONE', #16890, #1237 ) ;
#14589 = CARTESIAN_POINT ( 'NONE',  ( 13.05603179413191839, 8.545058472539723837, -15.96546128479914373 ) ) ;
#14588 = AXIS2_PLACEMENT_3D ( 'NONE', #10835, #20143, #24288 ) ;
#14590 = CARTESIAN_POINT ( 'NONE',  ( 168.6922820468853672, -1.999999999999971800, -23.73366926340167282 ) ) ;
#14591 = EDGE_LOOP ( 'NONE', ( #3744, #15505, #3731, #3170, #23250, #28482, #3189, #17263 ) ) ;
#14592 = DIRECTION ( 'NONE',  ( -0.000000000000000000, -0.000000000000000000, 1.000000000000000000 ) ) ;
#14593 = ORIENTED_EDGE ( 'NONE', *, *, #11617, .T. ) ;
#14594 = CARTESIAN_POINT ( 'NONE',  ( 159.7287565553230024, -9.999999999999998224, -33.82050807568879947 ) ) ;
#14595 = CARTESIAN_POINT ( 'NONE',  ( 147.2287565553229740, -10.00000000000000355, -3.509618943233403510 ) ) ;
#14596 = ORIENTED_EDGE ( 'NONE', *, *, #4323, .T. ) ;
#14597 = VERTEX_POINT ( 'NONE', #17169 ) ;
#14598 = CARTESIAN_POINT ( 'NONE',  ( 11.22518019566232716, 9.085373951847735441, -17.24107067304604257 ) ) ;
#14599 = CARTESIAN_POINT ( 'NONE',  ( 25.27232213581778808, -7.536446408081735271, -18.87890555733638465 ) ) ;
#14600 = CARTESIAN_POINT ( 'NONE',  ( 23.43951749033787735, -6.062008688038916127, -19.28752554440484701 ) ) ;
#14601 = CARTESIAN_POINT ( 'NONE',  ( 0.000000000000000000, 0.000000000000000000, 0.000000000000000000 ) ) ;
#14602 = DIRECTION ( 'NONE',  ( 0.3090169943749475623, 8.338696094058001131E-17, 0.9510565162951536422 ) ) ;
#14603 = VECTOR ( 'NONE', #2708, 1000.000000000000000 ) ;
#14604 = DIRECTION ( 'NONE',  ( -0.8090169943749474513, -2.183098979609982436E-16, -0.5877852522924731371 ) ) ;
#14605 = VECTOR ( 'NONE', #20091, 1000.000000000000000 ) ;
#14606 = EDGE_CURVE ( 'NONE', #29940, #10176, #9049, .T. ) ;
#14607 = AXIS2_PLACEMENT_3D ( 'NONE', #27888, #4946, #4794 ) ;
#14608 = EDGE_CURVE ( 'NONE', #3493, #8851, #6655, .T. ) ;
#14609 = ADVANCED_FACE ( 'NONE', ( #19010 ), #21747, .T. ) ;
#14610 = ORIENTED_EDGE ( 'NONE', *, *, #4327, .T. ) ;
#14611 = AXIS2_PLACEMENT_3D ( 'NONE', #16432, #12299, #21617 ) ;
#14612 = CARTESIAN_POINT ( 'NONE',  ( 15.92573302067464702, -5.000000000000013323, -49.01436633517871400 ) ) ;
#14613 = LINE ( 'NONE', #739, #23537 ) ;
#14614 = CARTESIAN_POINT ( 'NONE',  ( 0.000000000000000000, -2.357898499370430834, 3.469446951953614189E-15 ) ) ;
#14615 = DIRECTION ( 'NONE',  ( -0.8090169943749474513, -2.183098979609982436E-16, -0.5877852522924731371 ) ) ;
#14616 = CARTESIAN_POINT ( 'NONE',  ( 172.0152310637604387, -1.999999999999970468, -6.958068083716895558 ) ) ;
#14617 = VECTOR ( 'NONE', #6857, 1000.000000000000000 ) ;
#14618 = CARTESIAN_POINT ( 'NONE',  ( 12.02817646543008934, 9.315460371489308500, -16.69127922251917795 ) ) ;
#14619 = LINE ( 'NONE', #19927, #30229 ) ;
#14620 = CARTESIAN_POINT ( 'NONE',  ( 151.1922820468853672, -10.00000000000000178, -4.936203717676158398 ) ) ;
#14621 = VERTEX_POINT ( 'NONE', #12429 ) ;
#14622 = VECTOR ( 'NONE', #16521, 1000.000000000000000 ) ;
#14623 = CARTESIAN_POINT ( 'NONE',  ( 13.38776246403941350, 7.629555522264023892, -15.70137656829213491 ) ) ;
#14624 = DIRECTION ( 'NONE',  ( -0.000000000000000000, -0.000000000000000000, 1.000000000000000000 ) ) ;
#14625 = CARTESIAN_POINT ( 'NONE',  ( 24.81358459371387326, -5.676498915796258871, -18.90393244824272756 ) ) ;
#14626 = CARTESIAN_POINT ( 'NONE',  ( 12.81602886594196988, 9.615025227323064527, -16.14774825664093783 ) ) ;
#14627 = CARTESIAN_POINT ( 'NONE',  ( 24.55500000000002103, 0.000000000000000000, 0.000000000000000000 ) ) ;
#14628 = ORIENTED_EDGE ( 'NONE', *, *, #7022, .F. ) ;
#14629 = AXIS2_PLACEMENT_3D ( 'NONE', #23965, #24402, #12637 ) ;
#14630 = ORIENTED_EDGE ( 'NONE', *, *, #10991, .T. ) ;
#14631 = CARTESIAN_POINT ( 'NONE',  ( 11.47327446659168615, 9.267463859335506982, -15.86074700677745852 ) ) ;
#14632 = DIRECTION ( 'NONE',  ( 1.000000000000000000, 0.000000000000000000, 0.000000000000000000 ) ) ;
#14633 = CARTESIAN_POINT ( 'NONE',  ( 9.907423389235603395, 16.44864837861227969, -16.50891839478055090 ) ) ;
#14634 = CARTESIAN_POINT ( 'NONE',  ( 97.60856866274521337, -4.999999999999991118, -70.91677623121574925 ) ) ;
#14635 = EDGE_LOOP ( 'NONE', ( #3124, #20787, #9356, #8743, #11941 ) ) ;
#14636 = PLANE ( 'NONE',  #2320 ) ;
#14637 = VERTEX_POINT ( 'NONE', #7422 ) ;
#14638 = CARTESIAN_POINT ( 'NONE',  ( 12.02799090998256304, 9.316311091778235465, -16.69135597610317134 ) ) ;
#14639 = ORIENTED_EDGE ( 'NONE', *, *, #11755, .F. ) ;
#14640 = CARTESIAN_POINT ( 'NONE',  ( 36.54276536429808431, -23.15833126744076509, -18.75760452913613463 ) ) ;
#14641 = CARTESIAN_POINT ( 'NONE',  ( 26.38113052396219516, -11.59678093645141672, -17.84452879788985769 ) ) ;
#14642 = CARTESIAN_POINT ( 'NONE',  ( 17.06037746458228810, 10.50611453990982191, -19.02300506704843741 ) ) ;
#14643 = FACE_OUTER_BOUND ( 'NONE', #9913, .T. ) ;
#14644 = EDGE_LOOP ( 'NONE', ( #23013, #19826 ) ) ;
#14645 = DIRECTION ( 'NONE',  ( 0.5877852522924731371, 1.586114251531760728E-16, -0.8090169943749474513 ) ) ;
#14646 = ITEM_DEFINED_TRANSFORMATION ( 'NONE', 'NONE', #24883,  #13190 ) ;
#14647 = CARTESIAN_POINT ( 'NONE',  ( 17.84334503882807255, 1.539790780908459000, -16.51430848555953190 ) ) ;
#14648 = AXIS2_PLACEMENT_3D ( 'NONE', #6371, #15507, #15351 ) ;
#14649 = CARTESIAN_POINT ( 'NONE',  ( 16.06572049258021195, 3.735912457719189117, -15.00855390560170477 ) ) ;
#14650 = ADVANCED_FACE ( 'NONE', ( #7713 ), #16569, .T. ) ;
#14651 = EDGE_CURVE ( 'NONE', #4252, #7125, #14714, .T. ) ;
#14652 = EDGE_CURVE ( 'NONE', #17128, #29523, #559, .T. ) ;
#14653 = CARTESIAN_POINT ( 'NONE',  ( 133.6922820468854241, -4.999999999999981348, -15.07341522555727309 ) ) ;
#14654 = ADVANCED_FACE ( 'NONE', ( #14259 ), #24056, .T. ) ;
#14655 = DIRECTION ( 'NONE',  ( -0.8090169943749474513, -2.183098979609982436E-16, -0.5877852522924731371 ) ) ;
#14656 = FACE_OUTER_BOUND ( 'NONE', #14295, .T. ) ;
#14657 = LINE ( 'NONE', #24004, #26240 ) ;
#14658 = DIRECTION ( 'NONE',  ( -2.698458740408365879E-16, 1.000000000000000000, 0.000000000000000000 ) ) ;
#14659 = CARTESIAN_POINT ( 'NONE',  ( 175.7287565553229456, -9.999999999999994671, -10.89389676854971967 ) ) ;
#14660 = CARTESIAN_POINT ( 'NONE',  ( 12.27187887740847039, 9.517710768097034091, -15.31277030567625452 ) ) ;
#14662 = VECTOR ( 'NONE', #26682, 1000.000000000000000 ) ;
#14661 = PLANE ( 'NONE',  #22642 ) ;
#14663 = DIRECTION ( 'NONE',  ( 0.000000000000000000, 0.4999999999999993339, -0.8660254037844390407 ) ) ;
#14664 = ORIENTED_EDGE ( 'NONE', *, *, #20404, .T. ) ;
#14665 = AXIS2_PLACEMENT_3D ( 'NONE', #24645, #29890, #24804 ) ;
#14666 = CARTESIAN_POINT ( 'NONE',  ( 11.92109019680886206, 8.606374460406147620, -15.56934379943068336 ) ) ;
#14667 = ORIENTED_EDGE ( 'NONE', *, *, #30029, .T. ) ;
#14668 = CARTESIAN_POINT ( 'NONE',  ( 20.65939765650831461, 5.541921473274042498, -17.57530766875797568 ) ) ;
#14669 = CYLINDRICAL_SURFACE ( 'NONE', #1525, 4.000000000000000000 ) ;
#14670 = DIRECTION ( 'NONE',  ( -0.5877852522924731371, -1.586114251531760728E-16, -0.8090169943749474513 ) ) ;
#14671 = FACE_OUTER_BOUND ( 'NONE', #26317, .T. ) ;
#14672 = ORIENTED_EDGE ( 'NONE', *, *, #5753, .F. ) ;
#14673 = DIRECTION ( 'NONE',  ( 0.000000000000000000, -2.775557561562890735E-17, 1.000000000000000000 ) ) ;
#14674 = CARTESIAN_POINT ( 'NONE',  ( 12.83224840168406544, 9.540640483216481726, -16.14104089933701758 ) ) ;
#14675 = ADVANCED_FACE ( 'NONE', ( #2555 ), #5275, .T. ) ;
#14676 = ORIENTED_EDGE ( 'NONE', *, *, #18518, .T. ) ;
#14677 = CARTESIAN_POINT ( 'NONE',  ( 35.52138705868412671, -21.06228986472472897, -18.81697501280657647 ) ) ;
#14678 = CARTESIAN_POINT ( 'NONE',  ( 20.52488529563827058, 3.974637744936419637, -19.97762432673833288 ) ) ;
#14679 = ORIENTED_EDGE ( 'NONE', *, *, #28100, .T. ) ;
#14680 = ORIENTED_EDGE ( 'NONE', *, *, #15888, .F. ) ;
#14681 = PLANE ( 'NONE',  #10112 ) ;
#14682 = CARTESIAN_POINT ( 'NONE',  ( 13.93491968177131923, 5.624373287173536795, -18.66784319378200863 ) ) ;
#14683 = ORIENTED_EDGE ( 'NONE', *, *, #25396, .T. ) ;
#14684 = CARTESIAN_POINT ( 'NONE',  ( 172.7287565553229456, -3.999999999999989786, -33.50000000000000000 ) ) ;
#14685 = PRESENTATION_STYLE_ASSIGNMENT (( #26314 ) ) ;
#14686 = CARTESIAN_POINT ( 'NONE',  ( 24.47846259200217034, 0.2319951948203725633, -15.89054235832688278 ) ) ;
#14687 = CARTESIAN_POINT ( 'NONE',  ( 18.77375537285786322, 7.252522315878067616, -16.50763127152984566 ) ) ;
#14688 = DIRECTION ( 'NONE',  ( -2.698458740408365879E-16, 1.000000000000000000, 0.000000000000000000 ) ) ;
#14689 = EDGE_CURVE ( 'NONE', #19491, #14621, #17611, .T. ) ;
#14690 = ORIENTED_EDGE ( 'NONE', *, *, #19238, .T. ) ;
#14692 = ORIENTED_EDGE ( 'NONE', *, *, #24186, .F. ) ;
#14691 = EDGE_CURVE ( 'NONE', #10866, #3794, #1013, .T. ) ;
#14693 = CARTESIAN_POINT ( 'NONE',  ( 142.0152310637605240, -4.999999999999979572, -0.06116980274991495881 ) ) ;
#14694 = DIRECTION ( 'NONE',  ( 0.000000000000000000, 0.000000000000000000, -1.000000000000000000 ) ) ;
#14695 = DIRECTION ( 'NONE',  ( 0.9510565162951535312, 2.566386769018988816E-16, -0.3090169943749475623 ) ) ;
#14696 = CYLINDRICAL_SURFACE ( 'NONE', #17473, 8.000000000000007105 ) ;
#14697 = DIRECTION ( 'NONE',  ( 1.000000000000000000, 0.000000000000000000, 0.000000000000000000 ) ) ;
#14698 = CARTESIAN_POINT ( 'NONE',  ( 9.997747326010761881, 16.03441129093729245, -16.47093000352221637 ) ) ;
#14699 = CARTESIAN_POINT ( 'NONE',  ( 28.63860307613198941, -6.423989724335291918, -15.76775560094196749 ) ) ;
#14700 = CARTESIAN_POINT ( 'NONE',  ( 28.67999647541807207, -5.919990246138143952, -18.25217309140403188 ) ) ;
#14702 = VERTEX_POINT ( 'NONE', #5884 ) ;
#14701 = CARTESIAN_POINT ( 'NONE',  ( 33.35202879388211983, -12.33251541790028760, -19.68467382345759376 ) ) ;
#14703 = CARTESIAN_POINT ( 'NONE',  ( 0.000000000000000000, 0.000000000000000000, -5.000000000000000888 ) ) ;
#14704 = DIRECTION ( 'NONE',  ( -0.5877852522924731371, 0.000000000000000000, 0.8090169943749474513 ) ) ;
#14705 = LINE ( 'NONE', #5873, #13604 ) ;
#14706 = CARTESIAN_POINT ( 'NONE',  ( -5.355005115540915739, -6.145890662064674714, -4.917753204360272967 ) ) ;
#14707 = VECTOR ( 'NONE', #11312, 1000.000000000000000 ) ;
#14708 = LINE ( 'NONE', #10284, #3496 ) ;
#14709 = CARTESIAN_POINT ( 'NONE',  ( 163.6922820468853388, -9.999999999999998224, -17.92658477444275889 ) ) ;
#14710 = CARTESIAN_POINT ( 'NONE',  ( 16.94076125623460527, 0.4124075662712927692, -16.40086227390004936 ) ) ;
#14711 = CARTESIAN_POINT ( 'NONE',  ( 110.6334351267569502, -4.999999999999987566, 80.37989563891109412 ) ) ;
#14712 = CARTESIAN_POINT ( 'NONE',  ( 12.26747700539757346, 9.511763647452495363, -15.31658389161178668 ) ) ;
#14713 = ADVANCED_FACE ( 'NONE', ( #13039 ), #8005, .T. ) ;
#14714 = LINE ( 'NONE', #26197, #28128 ) ;
#14715 = CARTESIAN_POINT ( 'NONE',  ( 136.1922820468854241, -1.999999999999980460, -30.91696583120935671 ) ) ;
#14716 = CARTESIAN_POINT ( 'NONE',  ( 17.33713706444265412, 0.9871066061555996418, -18.79342181739402307 ) ) ;
#14717 = CARTESIAN_POINT ( 'NONE',  ( 12.84881458348222516, 5.748695638350556969, -17.40385974964576477 ) ) ;
#14718 = VERTEX_POINT ( 'NONE', #20201 ) ;
#14719 = CARTESIAN_POINT ( 'NONE',  ( 35.54859390953724585, -22.18451583373416014, -18.19919658220850778 ) ) ;
#14720 = CARTESIAN_POINT ( 'NONE',  ( 22.14981412484149104, -6.473446789742020258, -15.39974742277494713 ) ) ;
#14721 = AXIS2_PLACEMENT_3D ( 'NONE', #11173, #6304, #24931 ) ;
#14722 = CARTESIAN_POINT ( 'NONE',  ( 18.58892183794801056, 4.077935791202882854, -15.09018232067737841 ) ) ;
#14723 = EDGE_LOOP ( 'NONE', ( #5396, #6991, #6815, #17291, #29903, #25657 ) ) ;
#14724 = VECTOR ( 'NONE', #21950, 1000.000000000000000 ) ;
#14725 = LINE ( 'NONE', #24067, #23054 ) ;
#14727 = ORIENTED_EDGE ( 'NONE', *, *, #16415, .F. ) ;
#14726 = DIRECTION ( 'NONE',  ( -0.5877852522924731371, -1.586114251531760235E-16, 0.8090169943749474513 ) ) ;
#14728 = DIRECTION ( 'NONE',  ( -2.698458740408365879E-16, 1.000000000000000000, 0.000000000000000000 ) ) ;
#14729 = CARTESIAN_POINT ( 'NONE',  ( 5.000000000000006217, 2.832769448823991583E-15, -4.974599999999998801 ) ) ;
#14730 = DIRECTION ( 'NONE',  ( 0.5877852522924731371, 1.586114251531760728E-16, 0.8090169943749474513 ) ) ;
#14731 = CARTESIAN_POINT ( 'NONE',  ( 36.54859390953724585, -22.18451583373416014, -17.78191007148576475 ) ) ;
#14732 = CARTESIAN_POINT ( 'NONE',  ( 9.917205744531459644, 16.40378525026516243, -16.50423678068149869 ) ) ;
#14733 = VECTOR ( 'NONE', #19350, 1000.000000000000000 ) ;
#14734 = DIRECTION ( 'NONE',  ( -2.908569913943826047E-16, 1.000000000000000000, 6.826925868028084813E-18 ) ) ;
#14735 = CYLINDRICAL_SURFACE ( 'NONE', #29560, 2.749999999999999112 ) ;
#14736 = CARTESIAN_POINT ( 'NONE',  ( 12.11773132146483789, 9.045882004348337446, -16.64348121447567053 ) ) ;
#14737 = DIRECTION ( 'NONE',  ( 0.9510565162951536422, 0.000000000000000000, -0.3090169943749475623 ) ) ;
#14738 = EDGE_LOOP ( 'NONE', ( #16585, #21418, #20698, #15448 ) ) ;
#14739 = PLANE ( 'NONE',  #23680 ) ;
#14740 = EDGE_CURVE ( 'NONE', #22282, #11673, #13191, .T. ) ;
#14741 = ADVANCED_FACE ( 'NONE', ( #15164 ), #24500, .T. ) ;
#14742 = ORIENTED_EDGE ( 'NONE', *, *, #16372, .T. ) ;
#14743 = LINE ( 'NONE', #883, #2739 ) ;
#14744 = CARTESIAN_POINT ( 'NONE',  ( -3.345653888883662663, 2.687187980154698064, -2.310849780464865333 ) ) ;
#14745 = ADVANCED_FACE ( 'NONE', ( #29583 ), #10891, .T. ) ;
#14746 = CARTESIAN_POINT ( 'NONE',  ( -4.000000000000003553, -6.938893903907228378E-15, 8.673617379884035472E-16 ) ) ;
#14748 = ORIENTED_EDGE ( 'NONE', *, *, #11958, .T. ) ;
#14747 = AXIS2_PLACEMENT_3D ( 'NONE', #14424, #28527, #7577 ) ;
#14749 = EDGE_CURVE ( 'NONE', #4536, #18131, #24803, .T. ) ;
#14750 = ORIENTED_EDGE ( 'NONE', *, *, #9235, .T. ) ;
#14751 = ORIENTED_EDGE ( 'NONE', *, *, #3825, .F. ) ;
#14752 = CARTESIAN_POINT ( 'NONE',  ( 11.20778676255656059, 9.165115204199564047, -17.24826554773256149 ) ) ;
#14753 = CARTESIAN_POINT ( 'NONE',  ( 25.32913879335529472, -12.33208189297920221, -17.76794973357399243 ) ) ;
#14754 = CARTESIAN_POINT ( 'NONE',  ( 22.16683763302808430, -0.5050174593055701822, -13.96310542101677044 ) ) ;
#14755 = CARTESIAN_POINT ( 'NONE',  ( 162.0152310637604671, -4.999999999999974243, -6.958068083716895558 ) ) ;
#14756 = DIRECTION ( 'NONE',  ( 0.9510565162951536422, 0.000000000000000000, -0.3090169943749475623 ) ) ;
#14757 = PLANE ( 'NONE',  #12295 ) ;
#14758 = CARTESIAN_POINT ( 'NONE',  ( 154.5152310637604955, -10.00000000000000000, -13.05155085951651195 ) ) ;
#14759 = PLANE ( 'NONE',  #21604 ) ;
#14760 = FACE_OUTER_BOUND ( 'NONE', #3417, .T. ) ;
#14761 = PLANE ( 'NONE',  #7360 ) ;
#14762 = DIRECTION ( 'NONE',  ( 0.5877852522924731371, 1.586114251531760728E-16, 0.8090169943749474513 ) ) ;
#14763 = VECTOR ( 'NONE', #24474, 1000.000000000000114 ) ;
#14764 = CARTESIAN_POINT ( 'NONE',  ( 10.48212431696843439, 16.40585233633115436, -17.33062619162406293 ) ) ;
#14765 = CARTESIAN_POINT ( 'NONE',  ( 35.54859215833182873, -22.18450796649496226, -18.40462262104107083 ) ) ;
#14766 = ORIENTED_EDGE ( 'NONE', *, *, #4909, .F. ) ;
#14767 = CARTESIAN_POINT ( 'NONE',  ( 8.944584683310379702, 16.95159276115599667, -17.91664992932185996 ) ) ;
#14768 = CARTESIAN_POINT ( 'NONE',  ( 26.80628776457338347, -3.176708023846821494, -16.02594779711905559 ) ) ;
#14769 = CARTESIAN_POINT ( 'NONE',  ( 12.18385343395297049, 12.51426234204957844, -16.40917503585457737 ) ) ;
#14770 = FACE_BOUND ( 'NONE', #10886, .T. ) ;
#14771 = ORIENTED_EDGE ( 'NONE', *, *, #5974, .T. ) ;
#14772 = EDGE_CURVE ( 'NONE', #23292, #21455, #29270, .T. ) ;
#14773 = ORIENTED_EDGE ( 'NONE', *, *, #4063, .T. ) ;
#14774 = CARTESIAN_POINT ( 'NONE',  ( 11.47464782381437587, 9.261287281732329291, -15.86016978468419936 ) ) ;
#14775 = CARTESIAN_POINT ( 'NONE',  ( 132.0152310637605808, -10.00000000000000711, -24.27857615940569147 ) ) ;
#14776 = ADVANCED_FACE ( 'NONE', ( #19746 ), #23720, .T. ) ;
#14777 = ADVANCED_FACE ( 'NONE', ( #1460 ), #18876, .F. ) ;
#14778 = CARTESIAN_POINT ( 'NONE',  ( 11.47327446659168615, 9.267463859335506982, -15.86074700677745852 ) ) ;
#14779 = DIRECTION ( 'NONE',  ( 0.3090169943749472292, 8.338696094057992503E-17, -0.9510565162951536422 ) ) ;
#14780 = ADVANCED_FACE ( 'NONE', ( #26659 ), #1466, .T. ) ;
#14781 = EDGE_LOOP ( 'NONE', ( #3808, #29382, #6375, #19189 ) ) ;
#14782 = DIRECTION ( 'NONE',  ( -0.8090169943749474513, -2.183098979609982436E-16, 0.5877852522924731371 ) ) ;
#14783 = EDGE_LOOP ( 'NONE', ( #2399, #25641, #10454, #24943, #23616 ) ) ;
#14784 = CARTESIAN_POINT ( 'NONE',  ( 11.76876341733043141, 10.50516141373230106, -16.79855566342228101 ) ) ;
#14785 = ORIENTED_EDGE ( 'NONE', *, *, #13693, .F. ) ;
#14786 = CARTESIAN_POINT ( 'NONE',  ( 35.26378566547066384, -17.41255297500571331, -21.24391863398521352 ) ) ;
#14787 = CARTESIAN_POINT ( 'NONE',  ( 29.72799312938100513, -7.689056491358781997, -15.42978383025728384 ) ) ;
#14788 = CARTESIAN_POINT ( 'NONE',  ( 14.47211339546095488, 7.927559549074161716, -19.99378091926031686 ) ) ;
#14789 = DIRECTION ( 'NONE',  ( -2.698458740408365879E-16, 1.000000000000000000, 0.000000000000000000 ) ) ;
#14790 = VECTOR ( 'NONE', #2303, 1000.000000000000114 ) ;
#14791 = VERTEX_POINT ( 'NONE', #1163 ) ;
#14792 = EDGE_LOOP ( 'NONE', ( #9666, #19533, #28770 ) ) ;
#14793 = LINE ( 'NONE', #12666, #21539 ) ;
#14794 = VERTEX_POINT ( 'NONE', #24351 ) ;
#14795 = CARTESIAN_POINT ( 'NONE',  ( 18.10666546173949953, 1.615696121519054618, -15.79491705146812563 ) ) ;
#14796 = CARTESIAN_POINT ( 'NONE',  ( 14.17177033308128031, 6.273687421093853800, -17.36430109743762173 ) ) ;
#14797 = VERTEX_POINT ( 'NONE', #1313 ) ;
#14798 = VERTEX_POINT ( 'NONE', #29439 ) ;
#14799 = FACE_BOUND ( 'NONE', #11913, .T. ) ;
#14800 = DIRECTION ( 'NONE',  ( 1.000000000000000000, 4.440892098500622217E-16, 0.000000000000000000 ) ) ;
#14801 = CARTESIAN_POINT ( 'NONE',  ( 146.1922820468854241, -4.999999999999978684, -10.74328820663507678 ) ) ;
#14802 = DIRECTION ( 'NONE',  ( 0.000000000000000000, -1.000000000000000000, 1.287488025362403787E-15 ) ) ;
#14803 = LINE ( 'NONE', #16808, #749 ) ;
#14804 = AXIS2_PLACEMENT_3D ( 'NONE', #22981, #235, #16090 ) ;
#14805 = CARTESIAN_POINT ( 'NONE',  ( 12.27693567009463393, 9.494519571701449223, -15.31067915168583582 ) ) ;
#14806 = CARTESIAN_POINT ( 'NONE',  ( 25.00000000000001066, 55.00000000000000711, 24.99999999999998579 ) ) ;
#14807 = DIRECTION ( 'NONE',  ( -2.698458740408365879E-16, 1.000000000000000000, 0.000000000000000000 ) ) ;
#14808 = ORIENTED_EDGE ( 'NONE', *, *, #4059, .T. ) ;
#14809 = CARTESIAN_POINT ( 'NONE',  ( 11.51951884677450266, 9.108496074915260365, -15.83757232928968683 ) ) ;
#14810 = VERTEX_POINT ( 'NONE', #15021 ) ;
#14811 = EDGE_CURVE ( 'NONE', #7033, #17358, #8462, .T. ) ;
#14812 = CARTESIAN_POINT ( 'NONE',  ( 16.84217415841480303, 1.412180072802544872, -16.35713574856416841 ) ) ;
#14813 = DIRECTION ( 'NONE',  ( 0.5877852522924731371, 1.586114251531760728E-16, 0.8090169943749474513 ) ) ;
#14814 = DIRECTION ( 'NONE',  ( -2.698458740408365879E-16, 1.000000000000000000, 0.000000000000000000 ) ) ;
#14815 = ADVANCED_FACE ( 'NONE', ( #13197 ), #3595, .T. ) ;
#14816 = EDGE_CURVE ( 'NONE', #14597, #25113, #8312, .T. ) ;
#14817 = ORIENTED_EDGE ( 'NONE', *, *, #17209, .T. ) ;
#14818 = FACE_OUTER_BOUND ( 'NONE', #9535, .T. ) ;
#14819 = B_SPLINE_CURVE_WITH_KNOTS ( 'NONE', 3,
 ( #2479, #2328, #7485, #25650, #18478, #474 ),
 .UNSPECIFIED., .F., .F.,
 ( 4, 2, 4 ),
 ( 0.002336974151641603697, 0.003500975885716479247, 0.004664977619791355230 ),
 .UNSPECIFIED. ) ;
#14820 = ORIENTED_EDGE ( 'NONE', *, *, #16054, .T. ) ;
#14821 = LINE ( 'NONE', #965, #29624 ) ;
#14822 = EDGE_CURVE ( 'NONE', #26115, #24045, #21749, .T. ) ;
#14823 = ORIENTED_EDGE ( 'NONE', *, *, #11814, .F. ) ;
#14824 = CARTESIAN_POINT ( 'NONE',  ( 12.83280428553913666, 9.538383548424125280, -16.14078871935966220 ) ) ;
#14825 = CARTESIAN_POINT ( 'NONE',  ( 34.85979932414094407, -13.59765634092047470, -19.03716015824713281 ) ) ;
#14826 = CARTESIAN_POINT ( 'NONE',  ( 15.46244301724551740, 3.702889819443702990, -17.82701508041758842 ) ) ;
#14827 = ORIENTED_EDGE ( 'NONE', *, *, #13891, .T. ) ;
#14828 = FACE_OUTER_BOUND ( 'NONE', #20774, .T. ) ;
#14829 = CARTESIAN_POINT ( 'NONE',  ( 17.78134717446047119, 9.288666448780150020, -20.14505390916605521 ) ) ;
#14830 = ORIENTED_EDGE ( 'NONE', *, *, #13069, .F. ) ;
#14831 = DIRECTION ( 'NONE',  ( 0.000000000000000000, 0.000000000000000000, -1.000000000000000000 ) ) ;
#14832 = CARTESIAN_POINT ( 'NONE',  ( 26.68716238812262631, -2.792712658874448639, -18.04699283665395981 ) ) ;
#14833 = CARTESIAN_POINT ( 'NONE',  ( 20.19814137509539975, 5.716210941879356078, -15.87681946797394517 ) ) ;
#14834 = CIRCLE ( 'NONE', #21682, 5.000000000000000000 ) ;
#14835 = ORIENTED_EDGE ( 'NONE', *, *, #12144, .F. ) ;
#14836 = VERTEX_POINT ( 'NONE', #10757 ) ;
#14837 = DIRECTION ( 'NONE',  ( -0.8090169943749474513, -2.183098979609982436E-16, -0.5877852522924731371 ) ) ;
#14838 = CARTESIAN_POINT ( 'NONE',  ( 10.00000000000007816, 17.32050807568872486, -23.00000000000000711 ) ) ;
#14839 = ORIENTED_EDGE ( 'NONE', *, *, #9058, .T. ) ;
#14840 = CARTESIAN_POINT ( 'NONE',  ( -8.000000000000000000, 4.618802153517028941, -4.285468820183664818 ) ) ;
#14841 = CARTESIAN_POINT ( 'NONE',  ( 0.000000000000000000, 0.000000000000000000, 4.000000000000000000 ) ) ;
#14842 = PLANE ( 'NONE',  #25098 ) ;
#14843 = CARTESIAN_POINT ( 'NONE',  ( 11.69419402147360110, 8.800013620902292999, -15.72776802682527730 ) ) ;
#14844 = CARTESIAN_POINT ( 'NONE',  ( 28.03106068525412908, -6.431813172927290267, -14.41205174211060402 ) ) ;
#14845 = CARTESIAN_POINT ( 'NONE',  ( 27.71186802668094273, -7.007055141436442369, -19.33373627201896383 ) ) ;
#14846 = CARTESIAN_POINT ( 'NONE',  ( 35.41344336761681433, -22.57735604011907071, -20.16400759377322061 ) ) ;
#14847 = DIRECTION ( 'NONE',  ( -0.9510565162951536422, 0.000000000000000000, -0.3090169943749472292 ) ) ;
#14848 = LINE ( 'NONE', #1147, #25785 ) ;
#14849 = DIRECTION ( 'NONE',  ( -2.698458740408365879E-16, 1.000000000000000000, 0.000000000000000000 ) ) ;
#14850 = CARTESIAN_POINT ( 'NONE',  ( -5.690023276062409430, -5.952467836904174803, -4.869346954796176519 ) ) ;
#14851 = EDGE_CURVE ( 'NONE', #9311, #9725, #11994, .T. ) ;
#14852 = VECTOR ( 'NONE', #20742, 1000.000000000000000 ) ;
#14853 = DIRECTION ( 'NONE',  ( -1.000000000000000000, -2.698458740408365879E-16, 1.779203565104417375E-16 ) ) ;
#14854 = DIRECTION ( 'NONE',  ( 0.9510565162951536422, 2.566386769018988816E-16, 0.3090169943749472292 ) ) ;
#14855 = EDGE_CURVE ( 'NONE', #3793, #7383, #4045, .T. ) ;
#14856 = CARTESIAN_POINT ( 'NONE',  ( 22.29983652437130814, 0.6627547066652448304, -20.09853802436992964 ) ) ;
#14857 = VERTEX_POINT ( 'NONE', #3745 ) ;
#14858 = DIRECTION ( 'NONE',  ( -0.000000000000000000, -0.000000000000000000, -1.000000000000000000 ) ) ;
#14859 = EDGE_CURVE ( 'NONE', #6140, #10971, #22363, .T. ) ;
#14860 = CARTESIAN_POINT ( 'NONE',  ( 12.27491818236995691, 9.503772128122387031, -15.31151344616081822 ) ) ;
#14861 = ORIENTED_EDGE ( 'NONE', *, *, #86, .F. ) ;
#14862 = CARTESIAN_POINT ( 'NONE',  ( 32.54305136433941215, -11.03529315477374517, -18.08112484791816499 ) ) ;
#14863 = CARTESIAN_POINT ( 'NONE',  ( 7.975443363961738363, -5.000000000000015987, 24.54589074293864925 ) ) ;
#14864 = CARTESIAN_POINT ( 'NONE',  ( 25.55230692589818631, -0.5649882819070038975, -17.32853901032857280 ) ) ;
#14865 = CARTESIAN_POINT ( 'NONE',  ( 19.50094987086785636, 1.087406662839465632, -19.92270839898774781 ) ) ;
#14866 = VERTEX_POINT ( 'NONE', #19605 ) ;
#14867 = CARTESIAN_POINT ( 'NONE',  ( 35.09336438560361415, -20.13941072448723801, -20.22035334018532637 ) ) ;
#14868 = VECTOR ( 'NONE', #23469, 1000.000000000000000 ) ;
#14869 = CARTESIAN_POINT ( 'NONE',  ( 23.53678897557974281, -9.624609092408482169, -17.82855203159936863 ) ) ;
#14870 = CARTESIAN_POINT ( 'NONE',  ( 20.29686952095399377, -4.285349973794369660, -18.75376381207850329 ) ) ;
#14871 = CARTESIAN_POINT ( 'NONE',  ( 24.36497833745277930, -6.082191617938494055, -18.74521747929614435 ) ) ;
#14872 = AXIS2_PLACEMENT_3D ( 'NONE', #2679, #88, #27898 ) ;
#14873 = CARTESIAN_POINT ( 'NONE',  ( 144.5152310637606092, -10.00000000000000178, -28.60870317832789311 ) ) ;
#14874 = EDGE_CURVE ( 'NONE', #24756, #19707, #21283, .T. ) ;
#14875 = ORIENTED_EDGE ( 'NONE', *, *, #6785, .F. ) ;
#14876 = LINE ( 'NONE', #21916, #9131 ) ;
#14877 = CARTESIAN_POINT ( 'NONE',  ( 172.0152310637605240, -9.999999999999994671, -32.93883019725009120 ) ) ;
#14878 = CARTESIAN_POINT ( 'NONE',  ( 16.96387855261641775, 8.441957738943033362, -20.67322241009641814 ) ) ;
#14879 = VECTOR ( 'NONE', #24680, 1000.000000000000000 ) ;
#14880 = CARTESIAN_POINT ( 'NONE',  ( 35.91774987194125401, -19.35046774019819438, -20.39927477693754554 ) ) ;
#14881 = CARTESIAN_POINT ( 'NONE',  ( 9.826288910175632552, 16.82074144182198694, -16.60662094963572244 ) ) ;
#14882 = CARTESIAN_POINT ( 'NONE',  ( -2.000000000000008882, 3.464101615137750390, -2.450000000000000622 ) ) ;
#14883 = CARTESIAN_POINT ( 'NONE',  ( 0.6543471694412491546, 8.859816792613669278, -4.503584543331193402 ) ) ;
#14884 = CARTESIAN_POINT ( 'NONE',  ( 12.02835731808789355, 9.314632867394664117, -16.69120428796748357 ) ) ;
#14885 = FACE_OUTER_BOUND ( 'NONE', #7301, .T. ) ;
#14886 = ORIENTED_EDGE ( 'NONE', *, *, #17750, .T. ) ;
#14887 = DIRECTION ( 'NONE',  ( -2.698458740408365879E-16, 1.000000000000000000, 0.000000000000000000 ) ) ;
#14888 = ORIENTED_EDGE ( 'NONE', *, *, #10141, .F. ) ;
#14889 = VECTOR ( 'NONE', #23908, 1000.000000000000000 ) ;
#14890 = CARTESIAN_POINT ( 'NONE',  ( 152.0152310637604671, -4.999999999999976907, -1.687708096207001986E-14 ) ) ;
#14891 = DIRECTION ( 'NONE',  ( 0.000000000000000000, 0.000000000000000000, -1.000000000000000000 ) ) ;
#14892 = ORIENTED_EDGE ( 'NONE', *, *, #11109, .F. ) ;
#14893 = VECTOR ( 'NONE', #18152, 1000.000000000000114 ) ;
#14894 = CARTESIAN_POINT ( 'NONE',  ( 166.1922820468853672, -1.999999999999972689, -19.40354224447947473 ) ) ;
#14895 = VERTEX_POINT ( 'NONE', #27286 ) ;
#14896 = ORIENTED_EDGE ( 'NONE', *, *, #5897, .T. ) ;
#14897 = CARTESIAN_POINT ( 'NONE',  ( 11.60705119439842292, 8.210639978236427439, -17.01629833992986462 ) ) ;
#14898 = VECTOR ( 'NONE', #19134, 1000.000000000000000 ) ;
#14899 = CARTESIAN_POINT ( 'NONE',  ( 32.75486304968715245, -9.956179044816899193, -14.71053347703266212 ) ) ;
#14900 = CARTESIAN_POINT ( 'NONE',  ( 19.87821071931953298, -1.530402839103173651, -15.12151443550766494 ) ) ;
#14901 = CARTESIAN_POINT ( 'NONE',  ( 168.6922820468853672, -1.999999999999970468, -23.73366926340167637 ) ) ;
#14902 = DIRECTION ( 'NONE',  ( 1.110223024625156540E-16, 2.995891024602366092E-32, 1.000000000000000000 ) ) ;
#14903 = LINE ( 'NONE', #17356, #1127 ) ;
#14904 = VECTOR ( 'NONE', #17907, 1000.000000000000000 ) ;
#14905 = VERTEX_POINT ( 'NONE', #6336 ) ;
#14906 = CARTESIAN_POINT ( 'NONE',  ( 130.7287565553229456, -10.00000000000000888, -4.785595155761466657 ) ) ;
#14907 = EDGE_CURVE ( 'NONE', #4252, #12812, #15632, .T. ) ;
#14908 = CARTESIAN_POINT ( 'NONE',  ( 32.20428705557502269, -10.20872362009771095, -14.89176492545819919 ) ) ;
#14909 = EDGE_CURVE ( 'NONE', #20491, #22518, #5738, .T. ) ;
#14910 = DIRECTION ( 'NONE',  ( 0.3331260486002958765, -0.05059491534325381845, -0.9415238660200613285 ) ) ;
#14911 = VECTOR ( 'NONE', #2207, 1000.000000000000000 ) ;
#14912 = EDGE_CURVE ( 'NONE', #6973, #27863, #6178, .T. ) ;
#14913 = CARTESIAN_POINT ( 'NONE',  ( 108.2065456726138848, -4.999999999999987566, 78.61665723970844510 ) ) ;
#14915 = DIRECTION ( 'NONE',  ( -2.698458740408365879E-16, 1.000000000000000000, 0.000000000000000000 ) ) ;
#14914 = VECTOR ( 'NONE', #13419, 1000.000000000000000 ) ;
#14916 = CARTESIAN_POINT ( 'NONE',  ( 12.03206445085756116, 9.298183410334813104, -16.68962916345529024 ) ) ;
#14917 = CARTESIAN_POINT ( 'NONE',  ( 35.22227017426903473, -20.71851614966110233, -20.19360243392694088 ) ) ;
#14918 = EDGE_LOOP ( 'NONE', ( #20268, #28719, #16782, #27836 ) ) ;
#14919 = CARTESIAN_POINT ( 'NONE',  ( 8.944716491630211763, 16.95098827139963049, -17.88239910762268181 ) ) ;
#14920 = PRODUCT ( 'double end studs bm=1.5d_am_AM A M10X60-N', 'double end studs bm=1.5d_am_AM A M10X60-N', '', ( #12667 ) ) ;
#14921 = CARTESIAN_POINT ( 'NONE',  ( 26.58455406938135468, -5.910422570377376950, -13.89432871846328688 ) ) ;
#14922 = CARTESIAN_POINT ( 'NONE',  ( 12.83280428553913666, 9.538383548424125280, -16.14078871935966220 ) ) ;
#14923 = FACE_BOUND ( 'NONE', #17165, .T. ) ;
#14924 = ORIENTED_EDGE ( 'NONE', *, *, #6229, .T. ) ;
#14925 = ORIENTED_EDGE ( 'NONE', *, *, #26222, .F. ) ;
#14926 = ORIENTED_EDGE ( 'NONE', *, *, #9429, .T. ) ;
#14927 = ORIENTED_EDGE ( 'NONE', *, *, #17365, .F. ) ;
#14928 = CARTESIAN_POINT ( 'NONE',  ( 19.98223898111942276, -5.000000000000012434, -61.49900794809289550 ) ) ;
#14929 = ORIENTED_EDGE ( 'NONE', *, *, #16143, .T. ) ;
#14930 = AXIS2_PLACEMENT_3D ( 'NONE', #23876, #12398, #2819 ) ;
#14931 = CARTESIAN_POINT ( 'NONE',  ( 12.07641845611955489, 8.540206757827041528, -15.45582622123028216 ) ) ;
#14932 = CARTESIAN_POINT ( 'NONE',  ( -3.149999999999998135, -1.149807694518792937E-15, 2.550000000000000266 ) ) ;
#14933 = ORIENTED_EDGE ( 'NONE', *, *, #22628, .T. ) ;
#14934 = CARTESIAN_POINT ( 'NONE',  ( 164.7287565553229456, -9.999999999999998224, -25.16025403784440329 ) ) ;
#14935 = EDGE_LOOP ( 'NONE', ( #2076, #4036, #22124, #3523 ) ) ;
#14936 = CARTESIAN_POINT ( 'NONE',  ( 12.02558468657594659, 9.327346335875439820, -16.69235103436730938 ) ) ;
#14937 = VERTEX_POINT ( 'NONE', #17468 ) ;
#14938 = VECTOR ( 'NONE', #18742, 1000.000000000000000 ) ;
#14939 = CARTESIAN_POINT ( 'NONE',  ( 16.89391627328321732, 8.154734282165337689, -13.86877251323280014 ) ) ;
#14940 = CARTESIAN_POINT ( 'NONE',  ( 27.26129135193747999, -10.77754955263135095, -18.64424489656416739 ) ) ;
#14941 = LINE ( 'NONE', #24276, #20348 ) ;
#14942 = ORIENTED_EDGE ( 'NONE', *, *, #15410, .F. ) ;
#14943 = DIRECTION ( 'NONE',  ( 0.000000000000000000, 0.000000000000000000, 1.000000000000000000 ) ) ;
#14944 = PRODUCT_CONTEXT ( 'NONE', #12001, 'mechanical' ) ;
#14945 = CARTESIAN_POINT ( 'NONE',  ( 18.96452888794134495, 2.710274068595869057, -18.82741851907772457 ) ) ;
#14946 = CARTESIAN_POINT ( 'NONE',  ( 17.63704213852533442, 9.806822523219006271, -18.50018230520716145 ) ) ;
#14947 = DIRECTION ( 'NONE',  ( -2.698458740408365879E-16, 1.000000000000000000, 0.000000000000000000 ) ) ;
#14948 = CARTESIAN_POINT ( 'NONE',  ( 133.6922820468854241, -4.999999999999982236, -6.413161187712875133 ) ) ;
#14949 = EDGE_CURVE ( 'NONE', #28404, #11106, #26816, .T. ) ;
#14950 = EDGE_CURVE ( 'NONE', #20965, #7377, #15172, .T. ) ;
#14951 = VECTOR ( 'NONE', #15119, 1000.000000000000000 ) ;
#14952 = EDGE_CURVE ( 'NONE', #23002, #1908, #18369, .T. ) ;
#14953 = CARTESIAN_POINT ( 'NONE',  ( 149.7287565553230309, -10.00000000000000178, -25.16025403784440329 ) ) ;
#14954 = DIRECTION ( 'NONE',  ( -2.698458740408365879E-16, 1.000000000000000000, 0.000000000000000000 ) ) ;
#14955 = CARTESIAN_POINT ( 'NONE',  ( 2.500000000000000444, -1.178949249685215417, -2.041999999999998483 ) ) ;
#14956 = VECTOR ( 'NONE', #2285, 1000.000000000000000 ) ;
#14957 = ORIENTED_EDGE ( 'NONE', *, *, #23837, .T. ) ;
#14958 = DIRECTION ( 'NONE',  ( 0.000000000000000000, 0.000000000000000000, 1.000000000000000000 ) ) ;
#14959 = CARTESIAN_POINT ( 'NONE',  ( 12.27289197906229745, 9.513064554772155290, -15.31235135250446078 ) ) ;
#14960 = CARTESIAN_POINT ( 'NONE',  ( 19.99999999999998934, 60.00000000000000711, -30.00000000000000000 ) ) ;
#14961 = DIRECTION ( 'NONE',  ( -0.9510565162951536422, -2.566386769018988323E-16, 0.3090169943749475623 ) ) ;
#14962 = VERTEX_POINT ( 'NONE', #15776 ) ;
#14963 = CARTESIAN_POINT ( 'NONE',  ( 12.37169234869624646, 8.529253869913038244, -15.23127513898213081 ) ) ;
#14964 = VERTEX_POINT ( 'NONE', #13640 ) ;
#14965 = CARTESIAN_POINT ( 'NONE',  ( 10.66844579733420062, 9.045745945026473223, -16.41129889692150812 ) ) ;
#14966 = DIRECTION ( 'NONE',  ( 0.000000000000000000, 0.000000000000000000, 1.000000000000000000 ) ) ;
#14967 = LINE ( 'NONE', #22307, #5725 ) ;
#14968 = CARTESIAN_POINT ( 'NONE',  ( 172.7287565553229456, -1.999999999999970468, 0.5000000000000029976 ) ) ;
#14969 = DIRECTION ( 'NONE',  ( 0.9510565162951536422, 2.566386769018988816E-16, 0.3090169943749472292 ) ) ;
#14970 = VERTEX_POINT ( 'NONE', #11489 ) ;
#14971 = CARTESIAN_POINT ( 'NONE',  ( 12.31353044564305499, 11.91954703646417713, -16.35554902986205761 ) ) ;
#14972 = CARTESIAN_POINT ( 'NONE',  ( 34.00275312277798889, -11.14511497259480244, -17.96532559481354596 ) ) ;
#14973 = CARTESIAN_POINT ( 'NONE',  ( 19.20291185354690811, 8.143073066566493878, -16.32372945079811188 ) ) ;
#14974 = EDGE_LOOP ( 'NONE', ( #17939, #5762, #28895, #19400 ) ) ;
#14975 = ORIENTED_EDGE ( 'NONE', *, *, #26050, .F. ) ;
#14976 = VECTOR ( 'NONE', #23664, 999.9999999999998863 ) ;
#14977 = DIRECTION ( 'NONE',  ( 0.000000000000000000, 0.000000000000000000, -1.000000000000000000 ) ) ;
#14978 = CARTESIAN_POINT ( 'NONE',  ( 32.82164812444874968, -10.95096414870911161, -14.63344683186480211 ) ) ;
#14979 = DIRECTION ( 'NONE',  ( -1.000000000000000000, 0.000000000000000000, 0.000000000000000000 ) ) ;
#14980 = DIRECTION ( 'NONE',  ( 0.000000000000000000, 0.000000000000000000, 1.000000000000000000 ) ) ;
#14981 = FILL_AREA_STYLE_COLOUR ( '', #28864 ) ;
#14982 = CARTESIAN_POINT ( 'NONE',  ( 24.30592326428028827, -5.273034306582022879, -19.67074064463221106 ) ) ;
#14983 = VECTOR ( 'NONE', #19831, 1000.000000000000000 ) ;
#14984 = CARTESIAN_POINT ( 'NONE',  ( 20.09928279393940898, 2.810699353624661168, -13.58730878818371401 ) ) ;
#14985 = ORIENTED_EDGE ( 'NONE', *, *, #29649, .T. ) ;
#14986 = VERTEX_POINT ( 'NONE', #23261 ) ;
#14987 = CARTESIAN_POINT ( 'NONE',  ( 161.1922820468853672, -4.999999999999973355, -19.40354224447947828 ) ) ;
#14988 = EDGE_CURVE ( 'NONE', #15011, #6983, #25545, .T. ) ;
#14989 = ADVANCED_FACE ( 'NONE', ( #13785 ), #70, .T. ) ;
#14990 = EDGE_CURVE ( 'NONE', #15438, #5490, #7465, .T. ) ;
#14991 = DIRECTION ( 'NONE',  ( -0.5877852522924731371, 0.000000000000000000, 0.8090169943749474513 ) ) ;
#14992 = ADVANCED_FACE ( 'NONE', ( #2372 ), #20654, .T. ) ;
#14993 = CARTESIAN_POINT ( 'NONE',  ( 162.0152310637604955, -1.999999999999972689, -15.61832212156129707 ) ) ;
#14994 = LINE ( 'NONE', #24329, #15045 ) ;
#14995 = CARTESIAN_POINT ( 'NONE',  ( 172.7287565553229456, -3.999999999999989786, 8.500000000000003553 ) ) ;
#14996 = VECTOR ( 'NONE', #2228, 999.9999999999998863 ) ;
#14997 = VERTEX_POINT ( 'NONE', #11645 ) ;
#14998 = CARTESIAN_POINT ( 'NONE',  ( 11.47155695691762212, 9.275332456566969697, -15.86145787682774078 ) ) ;
#14999 = CARTESIAN_POINT ( 'NONE',  ( 29.00298259868716499, -8.617193473538632631, -14.90553363820342092 ) ) ;
#15000 = CARTESIAN_POINT ( 'NONE',  ( 27.85014272824177795, -5.137623357037004013, -13.74226875356335320 ) ) ;
#15001 = ORIENTED_EDGE ( 'NONE', *, *, #20326, .F. ) ;
#15002 = CARTESIAN_POINT ( 'NONE',  ( 0.000000000000000000, 0.000000000000000000, 0.000000000000000000 ) ) ;
#15003 = CIRCLE ( 'NONE', #9653, 5.000000000000005329 ) ;
#15004 = CARTESIAN_POINT ( 'NONE',  ( 167.0152310637605240, -9.999999999999996447, -34.70218595412750773 ) ) ;
#15005 = DIRECTION ( 'NONE',  ( 0.3090169943749472292, 8.338696094057992503E-17, -0.9510565162951536422 ) ) ;
#15006 = CARTESIAN_POINT ( 'NONE',  ( -4.339467034331215167, -6.732211846623414431, -4.999999999999988454 ) ) ;
#15007 = CARTESIAN_POINT ( 'NONE',  ( 143.6922820468854241, -10.00000000000000355, -6.413161187712876909 ) ) ;
#15008 =( LENGTH_UNIT ( ) NAMED_UNIT ( * ) SI_UNIT ( .MILLI., .METRE. ) );
#15010 = VERTEX_POINT ( 'NONE', #23409 ) ;
#15009 = CARTESIAN_POINT ( 'NONE',  ( 18.97268594440662426, -2.511067197207834667, -17.06021009607598415 ) ) ;
#15011 = VERTEX_POINT ( 'NONE', #13490 ) ;
#15012 = CARTESIAN_POINT ( 'NONE',  ( 0.8120000000000002771, 0.000000000000000000, 0.000000000000000000 ) ) ;
#15013 = CARTESIAN_POINT ( 'NONE',  ( 12.27693567009463393, 9.494519571701449223, -15.31067915168583582 ) ) ;
#15014 = AXIS2_PLACEMENT_3D ( 'NONE', #12076, #12369, #28915 ) ;
#15015 = CARTESIAN_POINT ( 'NONE',  ( 134.7287565553230024, -10.00000000000000711, 0.8205080756887930260 ) ) ;
#15016 = CARTESIAN_POINT ( 'NONE',  ( 130.7287565553229456, -4.999999999999983125, 3.500000000000003109 ) ) ;
#15017 = CARTESIAN_POINT ( 'NONE',  ( 20.50636976340433293, -0.9757509181830721356, -19.91080244439677571 ) ) ;
#15018 = DIRECTION ( 'NONE',  ( 0.000000000000000000, 0.000000000000000000, 1.000000000000000000 ) ) ;
#15019 = CARTESIAN_POINT ( 'NONE',  ( 19.21851095677833499, -0.002285697959038230937, -14.55609667925758544 ) ) ;
#15020 = VERTEX_POINT ( 'NONE', #9353 ) ;
#15021 = CARTESIAN_POINT ( 'NONE',  ( 13.87499999999999822, 7.328119615409992624E-16, -4.756499999999999062 ) ) ;
#15022 = CARTESIAN_POINT ( 'NONE',  ( 28.04121823296437199, -4.154284946049297211, -14.96295611916008994 ) ) ;
#15023 = CARTESIAN_POINT ( 'NONE',  ( 19.06759106800826586, -1.100202736525451641, -14.71838255749352165 ) ) ;
#15024 = VERTEX_POINT ( 'NONE', #15924 ) ;
#15025 = CARTESIAN_POINT ( 'NONE',  ( 31.59793210864275537, -10.01186915388335485, -14.42687813506083039 ) ) ;
#15026 = AXIS2_PLACEMENT_3D ( 'NONE', #12420, #19736, #3430 ) ;
#15027 = ADVANCED_FACE ( 'NONE', ( #4192 ), #25403, .T. ) ;
#15028 = EDGE_CURVE ( 'NONE', #19562, #1114, #22817, .T. ) ;
#15029 = LINE ( 'NONE', #26827, #22594 ) ;
#15030 = EDGE_CURVE ( 'NONE', #17600, #28689, #6788, .T. ) ;
#15031 = AXIS2_PLACEMENT_3D ( 'NONE', #9061, #15942, #29761 ) ;
#15032 = ORIENTED_EDGE ( 'NONE', *, *, #24524, .T. ) ;
#15033 = PRESENTATION_STYLE_ASSIGNMENT (( #10156 ) ) ;
#15034 = DIRECTION ( 'NONE',  ( 0.7071067811865460184, -0.7071067811865490160, -5.772398745160920240E-16 ) ) ;
#15035 = LINE ( 'NONE', #21616, #1691 ) ;
#15036 = CARTESIAN_POINT ( 'NONE',  ( 14.06424326207706699, 5.752694757912038881, -19.02294901845717945 ) ) ;
#15037 = CARTESIAN_POINT ( 'NONE',  ( 36.07559364978101968, -20.05957622185551870, -20.44697815928661200 ) ) ;
#15038 = CARTESIAN_POINT ( 'NONE',  ( 11.45256130090833935, 9.362448956408465861, -15.86931324879919991 ) ) ;
#15039 = FACE_OUTER_BOUND ( 'NONE', #1448, .T. ) ;
#15040 = DIRECTION ( 'NONE',  ( -2.698458740408365879E-16, 1.000000000000000000, 0.000000000000000000 ) ) ;
#15041 = CARTESIAN_POINT ( 'NONE',  ( 13.15785925275590529, 8.585986940276173485, -15.88461348575242305 ) ) ;
#15042 = DIRECTION ( 'NONE',  ( -0.9510565162951536422, -2.566386769018988323E-16, 0.3090169943749475623 ) ) ;
#15043 = DIRECTION ( 'NONE',  ( 0.9510565162951535312, 2.566386769018988816E-16, -0.3090169943749475623 ) ) ;
#15044 = ORIENTED_EDGE ( 'NONE', *, *, #1553, .F. ) ;
#15045 = VECTOR ( 'NONE', #3422, 1000.000000000000000 ) ;
#15046 = CARTESIAN_POINT ( 'NONE',  ( 420.0000000000002274, 43.64101615137744972, 12.00000000000000178 ) ) ;
#15047 = CARTESIAN_POINT ( 'NONE',  ( 166.1922820468853672, -9.999999999999998224, -19.40354224447947828 ) ) ;
#15048 = PLANE ( 'NONE',  #7352 ) ;
#15049 = EDGE_LOOP ( 'NONE', ( #1846, #1610 ) ) ;
#15050 = VECTOR ( 'NONE', #8144, 1000.000000000000000 ) ;
#15051 = VERTEX_POINT ( 'NONE', #23112 ) ;
#15052 = CARTESIAN_POINT ( 'NONE',  ( 11.21589157578718421, 9.127945497600544300, -17.24491392235805876 ) ) ;
#15053 = CARTESIAN_POINT ( 'NONE',  ( 28.86700826148938859, -9.048814421258168039, -19.66053155205330683 ) ) ;
#15054 = CARTESIAN_POINT ( 'NONE',  ( 29.00434111665888182, -5.389956126880047549, -17.18324766788818181 ) ) ;
#15055 = DIRECTION ( 'NONE',  ( 0.9510565162951535312, 2.566386769018988816E-16, -0.3090169943749475623 ) ) ;
#15056 = CARTESIAN_POINT ( 'NONE',  ( 163.6922820468853104, -1.999999999999973133, -9.266330736598359152 ) ) ;
#15057 = PLANE ( 'NONE',  #20106 ) ;
#15058 = ORIENTED_EDGE ( 'NONE', *, *, #4572, .F. ) ;
#15059 = DIRECTION ( 'NONE',  ( -0.9510565162951536422, -2.566386769018988816E-16, -0.3090169943749472292 ) ) ;
#15060 = EDGE_CURVE ( 'NONE', #4331, #705, #8753, .T. ) ;
#15061 = VECTOR ( 'NONE', #4730, 1000.000000000000000 ) ;
#15063 = VERTEX_POINT ( 'NONE', #1921 ) ;
#15062 = DIRECTION ( 'NONE',  ( -1.000000000000000000, 0.000000000000000000, -0.000000000000000000 ) ) ;
#15064 = ORIENTED_EDGE ( 'NONE', *, *, #22835, .F. ) ;
#15065 = DIRECTION ( 'NONE',  ( -0.5877852522924731371, 0.000000000000000000, 0.8090169943749474513 ) ) ;
#15066 = DIRECTION ( 'NONE',  ( -2.698458740408365879E-16, 1.000000000000000000, 0.000000000000000000 ) ) ;
#15067 = VECTOR ( 'NONE', #2264, 1000.000000000000000 ) ;
#15068 = CARTESIAN_POINT ( 'NONE',  ( 12.07790154976966868, 9.144051220271959934, -16.66639656463015839 ) ) ;
#15069 = CARTESIAN_POINT ( 'NONE',  ( 35.54859390953724585, -22.18451583373416014, -16.11276402859391865 ) ) ;
#15070 = ORIENTED_EDGE ( 'NONE', *, *, #26191, .T. ) ;
#15071 = CARTESIAN_POINT ( 'NONE',  ( 9.122709158550120989, 16.13469121211704049, -17.05051537109504523 ) ) ;
#15072 = CARTESIAN_POINT ( 'NONE',  ( 22.97938783112199701, -3.359759438970757017, -19.62490732200095067 ) ) ;
#15073 = CARTESIAN_POINT ( 'NONE',  ( 10.35864918915110877, 16.97212501191939538, -21.33333333332589277 ) ) ;
#15074 = FACE_BOUND ( 'NONE', #19968, .T. ) ;
#15075 = ORIENTED_EDGE ( 'NONE', *, *, #16998, .T. ) ;
#15076 = ORIENTED_EDGE ( 'NONE', *, *, #12756, .T. ) ;
#15077 = CARTESIAN_POINT ( 'NONE',  ( 99.54732812125345731, -4.999999999999990230, 72.32536742939463181 ) ) ;
#15078 = CARTESIAN_POINT ( 'NONE',  ( 12.49899259368311988, 8.570259324921714494, -15.13097775544467005 ) ) ;
#15079 = CARTESIAN_POINT ( 'NONE',  ( 138.6922820468854241, -1.999999999999980016, -32.39392330124607611 ) ) ;
#15080 = ORIENTED_EDGE ( 'NONE', *, *, #647, .F. ) ;
#15081 = DIRECTION ( 'NONE',  ( -2.698458740408365879E-16, 1.000000000000000000, 0.000000000000000000 ) ) ;
#15082 = ORIENTED_EDGE ( 'NONE', *, *, #19893, .T. ) ;
#15083 = PRESENTATION_LAYER_ASSIGNMENT (  '', '', ( #13160 ) ) ;
#15084 = CARTESIAN_POINT ( 'NONE',  ( 12.98644063677341798, 8.526496012441747041, -16.01999686492960961 ) ) ;
#15085 = EDGE_CURVE ( 'NONE', #8261, #7790, #11200, .T. ) ;
#15086 = ORIENTED_EDGE ( 'NONE', *, *, #10100, .T. ) ;
#15087 = ADVANCED_FACE ( 'NONE', ( #18220 ), #27576, .T. ) ;
#15088 = VECTOR ( 'NONE', #15042, 999.9999999999998863 ) ;
#15089 = CARTESIAN_POINT ( 'NONE',  ( 20.44279466453895822, 5.363259340322034774, -13.44374883282906552 ) ) ;
#15090 = CARTESIAN_POINT ( 'NONE',  ( 22.66942224714451370, 5.529188492372526298, -17.57712505567429773 ) ) ;
#15091 = PRODUCT_DEFINITION ( 'UNKNOWN', '', #27823, #15569 ) ;
#15092 = CARTESIAN_POINT ( 'NONE',  ( 164.5152310637604671, -4.999999999999973355, -11.28819510263909542 ) ) ;
#15093 = EDGE_LOOP ( 'NONE', ( #5953, #7311, #20966 ) ) ;
#15094 = VECTOR ( 'NONE', #23463, 1000.000000000000000 ) ;
#15095 = VECTOR ( 'NONE', #6645, 1000.000000000000000 ) ;
#15096 = CARTESIAN_POINT ( 'NONE',  ( 36.48591233058812833, -21.90292070287360460, -19.44112467175505898 ) ) ;
#15097 = APPLICATION_PROTOCOL_DEFINITION ( 'draft international standard', 'automotive_design', 1998, #13390 ) ;
#15098 = EDGE_LOOP ( 'NONE', ( #3832, #25447, #16541, #9481 ) ) ;
#15099 = CARTESIAN_POINT ( 'NONE',  ( 18.47369133221681281, 7.987600538477567014, -15.27093437040897861 ) ) ;
#15100 = DIRECTION ( 'NONE',  ( 0.000000000000000000, 0.000000000000000000, 1.000000000000000000 ) ) ;
#15101 = AXIS2_PLACEMENT_3D ( 'NONE', #30103, #25464, #1839 ) ;
#15102 = FACE_BOUND ( 'NONE', #30231, .T. ) ;
#15103 = COLOUR_RGB ( '', 0.40784314, 0.44705882, 0.49803922) ;
#15104 = AXIS2_PLACEMENT_3D ( 'NONE', #29576, #15618, #8593 ) ;
#15105 = DIRECTION ( 'NONE',  ( -2.698458740408365879E-16, 1.000000000000000000, 0.000000000000000000 ) ) ;
#15106 = CARTESIAN_POINT ( 'NONE',  ( 33.68411698100747032, -13.80840863474736935, -19.79436191385186916 ) ) ;
#15107 = PRESENTATION_LAYER_ASSIGNMENT (  '', '', ( #20979 ) ) ;
#15108 = CARTESIAN_POINT ( 'NONE',  ( 129.5152310637605808, -10.00000000000000888, -28.60870317832789311 ) ) ;
#15109 = ORIENTED_EDGE ( 'NONE', *, *, #1975, .F. ) ;
#15110 = CARTESIAN_POINT ( 'NONE',  ( 13.00000000000000178, 1.592040838891559293E-15, -15.00000000000000000 ) ) ;
#15111 = CARTESIAN_POINT ( 'NONE',  ( 11.04501277462238029, 15.14427510452705583, -15.82012259674246657 ) ) ;
#15112 = CARTESIAN_POINT ( 'NONE',  ( 157.0152310637604955, -10.00000000000000000, -6.958068083716895558 ) ) ;
#15113 = ORIENTED_EDGE ( 'NONE', *, *, #15375, .F. ) ;
#15114 = FACE_OUTER_BOUND ( 'NONE', #21522, .T. ) ;
#15115 = ORIENTED_EDGE ( 'NONE', *, *, #15916, .F. ) ;
#15116 = CARTESIAN_POINT ( 'NONE',  ( 11.47748818427356987, 9.248962635895034978, -15.85894168489154765 ) ) ;
#15117 = CARTESIAN_POINT ( 'NONE',  ( 12.69188586677704400, 7.599409645471840058, -14.97709067247704340 ) ) ;
#15118 = CARTESIAN_POINT ( 'NONE',  ( 16.00000000000017053, 34.64101615137744972, 14.00000000000000178 ) ) ;
#15119 = DIRECTION ( 'NONE',  ( 0.5877852522924731371, 1.586114251531760728E-16, -0.8090169943749474513 ) ) ;
#15120 = EDGE_LOOP ( 'NONE', ( #20808, #2956, #22147, #16435 ) ) ;
#15121 = DIRECTION ( 'NONE',  ( -0.9510565162951536422, 0.000000000000000000, -0.3090169943749472292 ) ) ;
#15122 = ORIENTED_EDGE ( 'NONE', *, *, #23050, .T. ) ;
#15123 = CARTESIAN_POINT ( 'NONE',  ( 12.50804596317817463, 11.02747407808666580, -16.27511002087113567 ) ) ;
#15124 = VECTOR ( 'NONE', #29312, 1000.000000000000000 ) ;
#15125 = EDGE_CURVE ( 'NONE', #5854, #27422, #18527, .T. ) ;
#15126 = ADVANCED_FACE ( 'NONE', ( #29746 ), #27882, .T. ) ;
#15128 = AXIS2_PLACEMENT_3D ( 'NONE', #25205, #18318, #7188 ) ;
#15127 = CARTESIAN_POINT ( 'NONE',  ( 35.54859390953723164, -21.18451583373416014, -14.99999999999999822 ) ) ;
#15129 = CARTESIAN_POINT ( 'NONE',  ( 18.50902107916489570, 2.085137940960992697, -20.06823964296112450 ) ) ;
#15130 = EDGE_CURVE ( 'NONE', #5157, #15686, #2788, .T. ) ;
#15131 = DIRECTION ( 'NONE',  ( 1.000000000000000000, 0.000000000000000000, 0.000000000000000000 ) ) ;
#15132 = ADVANCED_FACE ( 'NONE', ( #12103 ), #22267, .F. ) ;
#15133 = CARTESIAN_POINT ( 'NONE',  ( 18.04976943019953239, 10.79320383120880145, -15.74583687248850161 ) ) ;
#15134 = DIRECTION ( 'NONE',  ( -0.7071067811865306973, 0.000000000000000000, 0.7071067811865643371 ) ) ;
#15135 = DIRECTION ( 'NONE',  ( -0.000000000000000000, 0.000000000000000000, 1.000000000000000000 ) ) ;
#15136 = MECHANICAL_DESIGN_GEOMETRIC_PRESENTATION_REPRESENTATION (  '', ( #21489 ), #29347 ) ;
#15137 = CARTESIAN_POINT ( 'NONE',  ( 22.45293885382703536, -0.3771200753331621081, -14.01028023225368635 ) ) ;
#15138 = CARTESIAN_POINT ( 'NONE',  ( 23.64629180402988951, 0.1506760071912668364, -12.95843554106259710 ) ) ;
#15139 = VERTEX_POINT ( 'NONE', #24029 ) ;
#15140 = DIRECTION ( 'NONE',  ( 0.5000000000000029976, -0.8660254037844370423, 0.000000000000000000 ) ) ;
#15141 = CARTESIAN_POINT ( 'NONE',  ( 164.7287565553229740, -4.999999999999973355, -25.16025403784441394 ) ) ;
#15142 = FACE_OUTER_BOUND ( 'NONE', #3775, .T. ) ;
#15143 = AXIS2_PLACEMENT_3D ( 'NONE', #27748, #16559, #18845 ) ;
#15144 = CARTESIAN_POINT ( 'NONE',  ( 180.7287565553229456, -3.999999999999995559, -33.50000000000000000 ) ) ;
#15145 = CARTESIAN_POINT ( 'NONE',  ( 172.7287565553229456, -3.999999999999989786, -41.50000000000000711 ) ) ;
#15146 = AXIS2_PLACEMENT_3D ( 'NONE', #22056, #5580, #10292 ) ;
#15147 = LINE ( 'NONE', #22036, #8505 ) ;
#15148 = CARTESIAN_POINT ( 'NONE',  ( 11.14863080475985591, 10.75631295387255548, -15.99499920034263489 ) ) ;
#15149 = CARTESIAN_POINT ( 'NONE',  ( 16.06572049258021195, 3.735912457719189117, -15.00855390560170477 ) ) ;
#15150 = CARTESIAN_POINT ( 'NONE',  ( 26.78588127033857091, -2.187643107580064861, -16.18476928258297676 ) ) ;
#15151 = ORIENTED_EDGE ( 'NONE', *, *, #27551, .T. ) ;
#15152 = DIRECTION ( 'NONE',  ( 0.5877852522924731371, 1.586114251531760728E-16, -0.8090169943749474513 ) ) ;
#15153 = LINE ( 'NONE', #17302, #27293 ) ;
#15154 = FACE_OUTER_BOUND ( 'NONE', #25326, .T. ) ;
#15155 = DIRECTION ( 'NONE',  ( -1.110223024625156540E-16, 0.000000000000000000, -1.000000000000000000 ) ) ;
#15156 = LINE ( 'NONE', #20495, #518 ) ;
#15157 = PLANE ( 'NONE',  #36 ) ;
#15159 = ORIENTED_EDGE ( 'NONE', *, *, #7980, .T. ) ;
#15158 = CARTESIAN_POINT ( 'NONE',  ( 20.14386580841007657, 1.771853782379294140, -13.30505882909219295 ) ) ;
#15160 = VERTEX_POINT ( 'NONE', #2976 ) ;
#15161 = CARTESIAN_POINT ( 'NONE',  ( 143.6922820468854525, -10.00000000000000355, -23.73366926340167282 ) ) ;
#15162 = CARTESIAN_POINT ( 'NONE',  ( 10.88291651000981730, 15.88766923650820928, -15.88715510423204513 ) ) ;
#15163 = EDGE_CURVE ( 'NONE', #16411, #8141, #7393, .T. ) ;
#15164 = FACE_OUTER_BOUND ( 'NONE', #8, .T. ) ;
#15165 = PLANE ( 'NONE',  #15146 ) ;
#15166 = EDGE_CURVE ( 'NONE', #13813, #14224, #527, .T. ) ;
#15167 = CARTESIAN_POINT ( 'NONE',  ( 20.99533150354982070, 4.487273811465053441, -19.54336078777620500 ) ) ;
#15168 = CARTESIAN_POINT ( 'NONE',  ( 169.5152310637604387, -9.999999999999996447, -2.627941064794695691 ) ) ;
#15169 = ADVANCED_FACE ( 'NONE', ( #16537 ), #668, .T. ) ;
#15170 = CARTESIAN_POINT ( 'NONE',  ( 19.77504133826384347, 1.335633644655777053, -20.04176789066487530 ) ) ;
#15171 = ORIENTED_EDGE ( 'NONE', *, *, #16448, .T. ) ;
#15172 = LINE ( 'NONE', #25257, #18364 ) ;
#15173 = CARTESIAN_POINT ( 'NONE',  ( 26.42637521690935998, -6.951663299830703302, -19.91275981816901464 ) ) ;
#15174 = VECTOR ( 'NONE', #7704, 1000.000000000000000 ) ;
#15175 = CARTESIAN_POINT ( 'NONE',  ( 27.77130384954419995, -2.130748013457071099, -15.99611347415175366 ) ) ;
#15176 = ORIENTED_EDGE ( 'NONE', *, *, #6530, .F. ) ;
#15177 = DIRECTION ( 'NONE',  ( -0.9510565162951536422, -2.566386769018988816E-16, -0.3090169943749472292 ) ) ;
#15178 = PRODUCT_DEFINITION_SHAPE ( 'NONE', 'NONE',  #30273 ) ;
#15179 = PLANE ( 'NONE',  #21611 ) ;
#15180 = ORIENTED_EDGE ( 'NONE', *, *, #13347, .F. ) ;
#15181 = VERTEX_POINT ( 'NONE', #814 ) ;
#15182 = CARTESIAN_POINT ( 'NONE',  ( 0.000000000000000000, 0.000000000000000000, -18.00000000000000000 ) ) ;
#15183 = PLANE ( 'NONE',  #29675 ) ;
#15184 = LINE ( 'NONE', #27299, #9957 ) ;
#15185 = AXIS2_PLACEMENT_3D ( 'NONE', #18604, #14002, #447 ) ;
#15186 = CARTESIAN_POINT ( 'NONE',  ( 8.000000000000000000, -4.618802153517027165, -0.7145311798163362926 ) ) ;
#15187 = CARTESIAN_POINT ( 'NONE',  ( 26.57181397551241275, -7.970695015363167713, -12.68872038106934852 ) ) ;
#15188 = LINE ( 'NONE', #8478, #13579 ) ;
#15189 = CARTESIAN_POINT ( 'NONE',  ( 34.27125395597954594, -11.98684039141630819, -19.88226891060491752 ) ) ;
#15190 = CARTESIAN_POINT ( 'NONE',  ( 132.0152310637605808, -4.999999999999982236, -32.93883019725009120 ) ) ;
#15191 = CARTESIAN_POINT ( 'NONE',  ( 10.24089172292967298, 14.91932009296530559, -16.37038124228770997 ) ) ;
#15192 = CARTESIAN_POINT ( 'NONE',  ( 22.52742378339506502, -5.000000000000011546, -69.33228131312529285 ) ) ;
#15193 = DIRECTION ( 'NONE',  ( -1.000000000000000000, -4.440892098500622217E-16, 0.000000000000000000 ) ) ;
#15194 = CARTESIAN_POINT ( 'NONE',  ( 13.13233772467555660, 8.574708520419219937, -15.90495459411799395 ) ) ;
#15195 = CARTESIAN_POINT ( 'NONE',  ( 175.7287565553229456, -9.999999999999994671, -19.55415080639412650 ) ) ;
#15196 = EDGE_LOOP ( 'NONE', ( #10966, #20164, #21630, #12920 ) ) ;
#15197 = CARTESIAN_POINT ( 'NONE',  ( 142.0152310637605808, -10.00000000000000355, -26.04193191628310800 ) ) ;
#15198 = ORIENTED_EDGE ( 'NONE', *, *, #7872, .T. ) ;
#15199 = DIRECTION ( 'NONE',  ( 2.908569913943825554E-16, -1.000000000000000000, 0.000000000000000000 ) ) ;
#15200 = CARTESIAN_POINT ( 'NONE',  ( 156.1922820468853672, -1.999999999999974909, -10.74328820663507678 ) ) ;
#15201 = EDGE_CURVE ( 'NONE', #29523, #24484, #12253, .T. ) ;
#15202 = EDGE_CURVE ( 'NONE', #6861, #25565, #14231, .T. ) ;
#15203 = LINE ( 'NONE', #3187, #19507 ) ;
#15204 = ORIENTED_EDGE ( 'NONE', *, *, #15932, .F. ) ;
#15205 = ORIENTED_EDGE ( 'NONE', *, *, #19721, .T. ) ;
#15206 = EDGE_CURVE ( 'NONE', #25233, #25802, #19421, .T. ) ;
#15207 = ORIENTED_EDGE ( 'NONE', *, *, #8413, .T. ) ;
#15208 = ADVANCED_FACE ( 'NONE', ( #7832 ), #5552, .F. ) ;
#15209 = CARTESIAN_POINT ( 'NONE',  ( 8.944584683310379702, 16.95159276115599667, -17.94384837343789130 ) ) ;
#15210 = CARTESIAN_POINT ( 'NONE',  ( 26.36605488913174611, -12.34709378291890758, -12.75955235896099005 ) ) ;
#15211 = CARTESIAN_POINT ( 'NONE',  ( 26.42570577731286718, -9.588051360687080305, -12.79080846482418643 ) ) ;
#15212 = CARTESIAN_POINT ( 'NONE',  ( 139.5152310637605524, -4.999999999999980460, -1.548930218128858365E-14 ) ) ;
#15213 = PLANE ( 'NONE',  #21867 ) ;
#15214 = AXIS2_PLACEMENT_3D ( 'NONE', #15556, #6418, #13573 ) ;
#15215 = LINE ( 'NONE', #8355, #19122 ) ;
#15216 = EDGE_LOOP ( 'NONE', ( #19184, #23787, #22273, #7297, #16378 ) ) ;
#15217 = LINE ( 'NONE', #5933, #19165 ) ;
#15218 = PLANE ( 'NONE',  #15560 ) ;
#15219 = VECTOR ( 'NONE', #7307, 1000.000000000000000 ) ;
#15220 = FACE_BOUND ( 'NONE', #26144, .T. ) ;
#15221 = DIRECTION ( 'NONE',  ( -2.698458740408365879E-16, 1.000000000000000000, 0.000000000000000000 ) ) ;
#15222 = CARTESIAN_POINT ( 'NONE',  ( 13.12723341905928898, 8.572452836447732594, -15.90902281579132449 ) ) ;
#15223 = CARTESIAN_POINT ( 'NONE',  ( 33.14486676600987636, -11.77651092997264293, -17.78036478212233717 ) ) ;
#15224 = ORIENTED_EDGE ( 'NONE', *, *, #2234, .T. ) ;
#15225 = CARTESIAN_POINT ( 'NONE',  ( 10.53902527060216343, 9.639284983934057749, -16.46481883690060144 ) ) ;
#15226 = ORIENTED_EDGE ( 'NONE', *, *, #1975, .T. ) ;
#15227 = VECTOR ( 'NONE', #21636, 1000.000000000000000 ) ;
#15228 = CARTESIAN_POINT ( 'NONE',  ( 25.04992766293576878, -3.547109489677171101, -13.67097983722207033 ) ) ;
#15229 = CARTESIAN_POINT ( 'NONE',  ( 12.86851577213266928, 9.516150637207879015, -16.11522534726903899 ) ) ;
#15230 = FACE_BOUND ( 'NONE', #26357, .T. ) ;
#15231 = ORIENTED_EDGE ( 'NONE', *, *, #12592, .T. ) ;
#15232 = ORIENTED_EDGE ( 'NONE', *, *, #3117, .T. ) ;
#15233 = ORIENTED_EDGE ( 'NONE', *, *, #21384, .T. ) ;
#15234 = CARTESIAN_POINT ( 'NONE',  ( 137.0152310637605808, -10.00000000000000533, -8.721423840594312082 ) ) ;
#15235 = EDGE_CURVE ( 'NONE', #18145, #22282, #7627, .T. ) ;
#15236 = CARTESIAN_POINT ( 'NONE',  ( 11.47372892693763902, 9.265404009280679531, -15.86055721330185619 ) ) ;
#15237 = LINE ( 'NONE', #3366, #22798 ) ;
#15238 = EDGE_LOOP ( 'NONE', ( #17385, #23432, #2170, #21993, #11330, #11389 ) ) ;
#15239 = VERTEX_POINT ( 'NONE', #18983 ) ;
#15240 = EDGE_CURVE ( 'NONE', #27929, #7222, #26188, .T. ) ;
#15241 = DIRECTION ( 'NONE',  ( 0.3090169943749475623, 8.338696094058001131E-17, 0.9510565162951536422 ) ) ;
#15242 = ORIENTED_EDGE ( 'NONE', *, *, #3408, .T. ) ;
#15243 = ADVANCED_FACE ( 'NONE', ( #11798 ), #19126, .T. ) ;
#15244 = CARTESIAN_POINT ( 'NONE',  ( 9.661883060892410668, 16.25482663691947849, -17.91599866193395485 ) ) ;
#15245 = ORIENTED_EDGE ( 'NONE', *, *, #2495, .T. ) ;
#15246 = CARTESIAN_POINT ( 'NONE',  ( 15.30633068984937317, 3.801504677414661693, -19.72534293519717608 ) ) ;
#15247 = CARTESIAN_POINT ( 'NONE',  ( 14.66608887309643272, 3.149405488550426568, -18.09902814372540192 ) ) ;
#15248 = ORIENTED_EDGE ( 'NONE', *, *, #9714, .T. ) ;
#15249 = DIRECTION ( 'NONE',  ( 2.698458740408365879E-16, -1.000000000000000000, 0.000000000000000000 ) ) ;
#15250 = ORIENTED_EDGE ( 'NONE', *, *, #20854, .T. ) ;
#15251 = DIRECTION ( 'NONE',  ( -0.5877852522924731371, -1.586114251531760728E-16, -0.8090169943749474513 ) ) ;
#15252 = CARTESIAN_POINT ( 'NONE',  ( 18.69974902744413470, 8.051839821468062652, -15.50866580261103955 ) ) ;
#15253 = VECTOR ( 'NONE', #8616, 1000.000000000000000 ) ;
#15254 = CARTESIAN_POINT ( 'NONE',  ( 167.0152310637604103, -4.999999999999972466, -1.854241549900774836E-14 ) ) ;
#15255 = FACE_BOUND ( 'NONE', #29221, .T. ) ;
#15256 = ORIENTED_EDGE ( 'NONE', *, *, #9505, .F. ) ;
#15257 = EDGE_CURVE ( 'NONE', #2706, #29352, #21261, .T. ) ;
#15258 = DIRECTION ( 'NONE',  ( 1.000000000000000000, 4.440892098500622217E-16, 0.000000000000000000 ) ) ;
#15259 = CARTESIAN_POINT ( 'NONE',  ( 33.27037009343090546, -12.05169513820189309, -19.60996450177851713 ) ) ;
#15260 = PLANE ( 'NONE',  #5324 ) ;
#15261 = DIRECTION ( 'NONE',  ( -1.000000000000000000, 0.000000000000000000, 0.000000000000000000 ) ) ;
#15262 = CARTESIAN_POINT ( 'NONE',  ( 11.05541573950045375, 17.68942145115775944, -17.91357985325011626 ) ) ;
#15263 = VERTEX_POINT ( 'NONE', #26165 ) ;
#15264 = CARTESIAN_POINT ( 'NONE',  ( 175.7287565553229456, -4.999999999999970690, -19.55415080639412295 ) ) ;
#15265 = EDGE_LOOP ( 'NONE', ( #12343, #17079, #26064, #24107, #8077 ) ) ;
#15266 = CARTESIAN_POINT ( 'NONE',  ( 0.000000000000000000, 0.000000000000000000, -5.000000000000000888 ) ) ;
#15267 = ORIENTED_EDGE ( 'NONE', *, *, #16094, .F. ) ;
#15268 = AXIS2_PLACEMENT_3D ( 'NONE', #3282, #14543, #24035 ) ;
#15269 = CARTESIAN_POINT ( 'NONE',  ( 12.74324588813389170, 7.620242904383297322, -14.93629796730785486 ) ) ;
#15270 = PLANE ( 'NONE',  #26381 ) ;
#15271 = DIRECTION ( 'NONE',  ( 1.000000000000000000, 4.440892098500622217E-16, 0.000000000000000000 ) ) ;
#15272 = DIRECTION ( 'NONE',  ( -0.000000000000000000, -0.000000000000000000, 1.000000000000000000 ) ) ;
#15273 = ORIENTED_EDGE ( 'NONE', *, *, #27360, .F. ) ;
#15274 = CARTESIAN_POINT ( 'NONE',  ( 11.43821061673542872, 15.93387534916056758, -16.71752457030684980 ) ) ;
#15275 = CARTESIAN_POINT ( 'NONE',  ( 35.92974604556026463, -18.40436019371391652, -19.36057938427370217 ) ) ;
#15276 = CARTESIAN_POINT ( 'NONE',  ( 19.50856600871340873, -1.908691058934758100, -18.90332006808282728 ) ) ;
#15277 = VERTEX_POINT ( 'NONE', #28181 ) ;
#15278 = ORIENTED_EDGE ( 'NONE', *, *, #1667, .F. ) ;
#15279 = CARTESIAN_POINT ( 'NONE',  ( 154.5152310637604671, -4.999999999999976019, -1.715463671822630899E-14 ) ) ;
#15280 = CARTESIAN_POINT ( 'NONE',  ( 28.15263004948277725, -12.62334012340276779, -12.05588540746726345 ) ) ;
#15281 = CARTESIAN_POINT ( 'NONE',  ( 134.5152310637605524, -4.999999999999981348, -4.391296821672111328 ) ) ;
#15282 = DIRECTION ( 'NONE',  ( -1.000000000000000000, -3.216245299353269257E-16, 0.000000000000000000 ) ) ;
#15283 = SURFACE_STYLE_USAGE ( .BOTH. , #20624 ) ;
#15284 = CARTESIAN_POINT ( 'NONE',  ( 26.42570577731286718, -9.588051360687080305, -12.79080846482418643 ) ) ;
#15285 = CARTESIAN_POINT ( 'NONE',  ( 17.37750100583229340, 1.587821987789380440, -15.03969266580305764 ) ) ;
#15286 = ORIENTED_EDGE ( 'NONE', *, *, #2681, .T. ) ;
#15287 = LINE ( 'NONE', #15449, #18609 ) ;
#15288 = CARTESIAN_POINT ( 'NONE',  ( 158.6922820468853672, -10.00000000000000000, -15.07341522555727664 ) ) ;
#15289 = VECTOR ( 'NONE', #8205, 1000.000000000000000 ) ;
#15290 = LINE ( 'NONE', #5860, #27990 ) ;
#15291 = EDGE_CURVE ( 'NONE', #590, #22963, #16689, .T. ) ;
#15292 = CARTESIAN_POINT ( 'NONE',  ( 156.1922820468853388, -1.999999999999974909, -2.083034168790677043 ) ) ;
#15293 = PLANE ( 'NONE',  #20412 ) ;
#15294 = EDGE_CURVE ( 'NONE', #2741, #23064, #1325, .T. ) ;
#15295 = DIRECTION ( 'NONE',  ( -2.698458740408365879E-16, 1.000000000000000000, 0.000000000000000000 ) ) ;
#15296 = CARTESIAN_POINT ( 'NONE',  ( 10.70528834225764392, 11.46963701334067842, -17.45606632095149280 ) ) ;
#15297 = CARTESIAN_POINT ( 'NONE',  ( 10.33811693838771717, 18.38618951776012267, -19.66666666666843000 ) ) ;
#15298 = CARTESIAN_POINT ( 'NONE',  ( 28.12627659338356878, -5.062120396530918498, -14.05642262879015369 ) ) ;
#15299 = ORIENTED_EDGE ( 'NONE', *, *, #29241, .F. ) ;
#15300 = CARTESIAN_POINT ( 'NONE',  ( 20.00000000000017053, 41.64101615137744972, 10.00000000000000178 ) ) ;
#15301 = CARTESIAN_POINT ( 'NONE',  ( 146.1922820468854525, -4.999999999999977796, -19.40354224447947828 ) ) ;
#15302 = EDGE_LOOP ( 'NONE', ( #18975, #26758, #1388, #5132 ) ) ;
#15303 = LINE ( 'NONE', #19738, #25431 ) ;
#15304 = FACE_OUTER_BOUND ( 'NONE', #8893, .T. ) ;
#15305 = DIRECTION ( 'NONE',  ( -2.698458740408365879E-16, 1.000000000000000000, 0.000000000000000000 ) ) ;
#15307 = ORIENTED_EDGE ( 'NONE', *, *, #22137, .T. ) ;
#15306 = CARTESIAN_POINT ( 'NONE',  ( 26.61709978538234012, -3.831456866606135492, -17.85214630790261836 ) ) ;
#15308 = ORIENTED_EDGE ( 'NONE', *, *, #13141, .F. ) ;
#15309 = CARTESIAN_POINT ( 'NONE',  ( 31.49119590023542870, -10.87553819600004701, -15.10823507476435523 ) ) ;
#15310 = CARTESIAN_POINT ( 'NONE',  ( 10.76134431155039373, 16.44521483549405971, -15.93742948484896615 ) ) ;
#15311 = DIRECTION ( 'NONE',  ( 0.000000000000000000, -0.000000000000000000, 1.000000000000000000 ) ) ;
#15312 = DIRECTION ( 'NONE',  ( -2.698458740408365879E-16, 1.000000000000000000, 0.000000000000000000 ) ) ;
#15313 = ORIENTED_EDGE ( 'NONE', *, *, #1278, .T. ) ;
#15314 = CARTESIAN_POINT ( 'NONE',  ( 28.16462234717350199, -5.661059359726887230, -16.30864077692347536 ) ) ;
#15315 = VECTOR ( 'NONE', #8621, 1000.000000000000000 ) ;
#15316 = DIRECTION ( 'NONE',  ( 6.938893903907227392E-16, -0.000000000000000000, 1.000000000000000000 ) ) ;
#15317 = CARTESIAN_POINT ( 'NONE',  ( 15.25645860304719292, 2.347722246533389789, -18.19294613283020112 ) ) ;
#15318 = EDGE_LOOP ( 'NONE', ( #93, #18025, #9689, #25954 ) ) ;
#15319 = CARTESIAN_POINT ( 'NONE',  ( 152.0152310637604671, -10.00000000000000178, -0.06116980274991495881 ) ) ;
#15320 = ORIENTED_EDGE ( 'NONE', *, *, #18557, .T. ) ;
#15321 = B_SPLINE_CURVE_WITH_KNOTS ( 'NONE', 3,
 ( #20360, #18683, #15935, #9357, #4201, #22975 ),
 .UNSPECIFIED., .F., .F.,
 ( 4, 2, 4 ),
 ( 0.002336974151641586783, 0.003500975885716471007, 0.004664977619791355230 ),
 .UNSPECIFIED. ) ;
#15322 = CARTESIAN_POINT ( 'NONE',  ( 25.80045869113294543, -2.244538201703065283, -16.37342509101419807 ) ) ;
#15323 = CARTESIAN_POINT ( 'NONE',  ( 20.46682838619579670, -4.770343855991169058, -14.23415315410508342 ) ) ;
#15324 = ORIENTED_EDGE ( 'NONE', *, *, #2925, .T. ) ;
#15325 = CARTESIAN_POINT ( 'NONE',  ( 28.06689949639850212, -8.111051215268487269, -13.49421662364394514 ) ) ;
#15326 = LINE ( 'NONE', #24666, #5530 ) ;
#15327 = ORIENTED_EDGE ( 'NONE', *, *, #26221, .T. ) ;
#15328 = ADVANCED_FACE ( 'NONE', ( #5241 ), #5092, .F. ) ;
#15329 = CARTESIAN_POINT ( 'NONE',  ( 138.6922820468854525, -1.999999999999979572, -26.58683881228715506 ) ) ;
#15330 = CARTESIAN_POINT ( 'NONE',  ( -19.99999999999998934, 60.00000000000000711, 24.99999999999998934 ) ) ;
#15331 = EDGE_CURVE ( 'NONE', #29853, #4723, #1274, .T. ) ;
#15332 = CARTESIAN_POINT ( 'NONE',  ( 171.1922820468853388, -9.999999999999996447, -19.40354224447947828 ) ) ;
#15333 = VECTOR ( 'NONE', #11621, 1000.000000000000000 ) ;
#15334 = EDGE_CURVE ( 'NONE', #19629, #23150, #12493, .T. ) ;
#15335 = CARTESIAN_POINT ( 'NONE',  ( 8.000000000000014211, -0.7805016046290984555, -7.137099613564734657E-15 ) ) ;
#15336 = CARTESIAN_POINT ( 'NONE',  ( 25.35799213500633442, -5.391047399292974163, -13.97031313328441726 ) ) ;
#15337 = CARTESIAN_POINT ( 'NONE',  ( 17.25677449038176547, 8.733363079223632752, -20.54546673180767158 ) ) ;
#15338 = CARTESIAN_POINT ( 'NONE',  ( 36.54859390953724585, -22.18451583373416014, -16.11276402859391865 ) ) ;
#15339 = CARTESIAN_POINT ( 'NONE',  ( 169.7287565553229456, -4.999999999999971578, -25.16025403784439973 ) ) ;
#15340 = CARTESIAN_POINT ( 'NONE',  ( 9.907423389235603395, 16.44864837861227969, -16.50891839478055090 ) ) ;
#15341 = DIRECTION ( 'NONE',  ( 0.000000000000000000, 0.000000000000000000, 1.000000000000000000 ) ) ;
#15342 = CARTESIAN_POINT ( 'NONE',  ( 149.5152310637605808, -10.00000000000000178, -30.37205893520531319 ) ) ;
#15343 = CARTESIAN_POINT ( 'NONE',  ( 9.661883061612440926, 16.25482663361732705, -17.97192418671890835 ) ) ;
#15344 = DIRECTION ( 'NONE',  ( -0.8090169943749474513, -2.183098979609982436E-16, -0.5877852522924731371 ) ) ;
#15345 = EDGE_LOOP ( 'NONE', ( #8317, #5279, #26692, #20305 ) ) ;
#15346 = CARTESIAN_POINT ( 'NONE',  ( 8.000000000000000000, 9.797174393178825657E-16, 9.999999999999998224 ) ) ;
#15347 = CARTESIAN_POINT ( 'NONE',  ( 11.46269231744662420, 9.315986823159681407, -15.86512371708112212 ) ) ;
#15348 = VECTOR ( 'NONE', #7887, 1000.000000000000000 ) ;
#15349 = VERTEX_POINT ( 'NONE', #17726 ) ;
#15350 = DIRECTION ( 'NONE',  ( 0.5877852522924731371, 0.000000000000000000, 0.8090169943749474513 ) ) ;
#15351 = DIRECTION ( 'NONE',  ( 0.9510565162951536422, 0.000000000000000000, -0.3090169943749475623 ) ) ;
#15352 = FACE_OUTER_BOUND ( 'NONE', #8876, .T. ) ;
#15353 = ORIENTED_EDGE ( 'NONE', *, *, #30232, .F. ) ;
#15354 = CARTESIAN_POINT ( 'NONE',  ( 13.43370121458407418, 7.649856678006609734, -15.66476257323406784 ) ) ;
#15355 = CARTESIAN_POINT ( 'NONE',  ( 34.30083361619418980, -13.08651950748960680, -20.95284133056243192 ) ) ;
#15356 = CARTESIAN_POINT ( 'NONE',  ( 25.85217995398321378, -12.57279400931185620, -13.36530271656463320 ) ) ;
#15357 = CARTESIAN_POINT ( 'NONE',  ( 29.30807694892355286, -8.357723062633453992, -13.20244061823602522 ) ) ;
#15358 = CARTESIAN_POINT ( 'NONE',  ( 167.0152310637605240, -9.999999999999996447, -24.27857615940569502 ) ) ;
#15359 = FACE_OUTER_BOUND ( 'NONE', #15302, .T. ) ;
#15360 = AXIS2_PLACEMENT_3D ( 'NONE', #1248, #29057, #17703 ) ;
#15361 = B_SPLINE_CURVE_WITH_KNOTS ( 'NONE', 3,
 ( #1482, #3911, #22832, #1634, #8624, #18085 ),
 .UNSPECIFIED., .F., .F.,
 ( 4, 2, 4 ),
 ( 2.380731629606037294E-07, 0.002336973833157549030, 0.004673709593152137499 ),
 .UNSPECIFIED. ) ;
#15362 = CARTESIAN_POINT ( 'NONE',  ( 157.0152310637605808, -1.999999999999973133, -32.93883019725009120 ) ) ;
#15363 = EDGE_CURVE ( 'NONE', #3275, #4291, #3271, .T. ) ;
#15364 = VERTEX_POINT ( 'NONE', #20026 ) ;
#15365 = FACE_OUTER_BOUND ( 'NONE', #29837, .T. ) ;
#15366 = AXIS2_PLACEMENT_3D ( 'NONE', #22225, #24831, #12758 ) ;
#15367 = EDGE_CURVE ( 'NONE', #19109, #15010, #21868, .T. ) ;
#15369 = ORIENTED_EDGE ( 'NONE', *, *, #26053, .F. ) ;
#15368 = DIRECTION ( 'NONE',  ( -2.698458740408365879E-16, 1.000000000000000000, 0.000000000000000000 ) ) ;
#15370 = ORIENTED_EDGE ( 'NONE', *, *, #6087, .T. ) ;
#15371 = ADVANCED_FACE ( 'NONE', ( #12852 ), #27245, .T. ) ;
#15372 = LINE ( 'NONE', #13541, #18543 ) ;
#15373 = DIRECTION ( 'NONE',  ( 0.000000000000000000, 0.000000000000000000, -1.000000000000000000 ) ) ;
#15374 = VECTOR ( 'NONE', #27637, 1000.000000000000000 ) ;
#15375 = EDGE_CURVE ( 'NONE', #7486, #12010, #29086, .T. ) ;
#15376 = EDGE_CURVE ( 'NONE', #9938, #19084, #16402, .T. ) ;
#15377 = ADVANCED_FACE ( 'NONE', ( #8424 ), #27084, .T. ) ;
#15378 = CARTESIAN_POINT ( 'NONE',  ( 13.15785925275590529, 8.585986940276173485, -15.88461348575242305 ) ) ;
#15379 = CARTESIAN_POINT ( 'NONE',  ( 33.61574637963836665, -12.50126044309498496, -18.73137083807847958 ) ) ;
#15380 = ORIENTED_EDGE ( 'NONE', *, *, #28071, .F. ) ;
#15381 = VECTOR ( 'NONE', #20938, 1000.000000000000000 ) ;
#15382 = CARTESIAN_POINT ( 'NONE',  ( 9.105507159292685060, 16.21358177345661389, -17.05825009255364932 ) ) ;
#15383 = EDGE_LOOP ( 'NONE', ( #6938, #19439, #12720, #25476 ) ) ;
#15384 = VECTOR ( 'NONE', #838, 1000.000000000000000 ) ;
#15385 = CARTESIAN_POINT ( 'NONE',  ( 26.48263329513011755, -12.06126822337667903, -13.95730679897583038 ) ) ;
#15386 = CARTESIAN_POINT ( 'NONE',  ( 10.35864918915110877, 16.97212501191939538, -23.00000000000000711 ) ) ;
#15387 = FACE_BOUND ( 'NONE', #8347, .T. ) ;
#15388 = VECTOR ( 'NONE', #30048, 999.9999999999998863 ) ;
#15389 = ORIENTED_EDGE ( 'NONE', *, *, #11572, .F. ) ;
#15390 = DIRECTION ( 'NONE',  ( 0.5877852522924731371, 1.586114251531760728E-16, 0.8090169943749474513 ) ) ;
#15391 = CARTESIAN_POINT ( 'NONE',  ( 11.47079713067724782, 9.278817116560638567, -15.86177209170659275 ) ) ;
#15392 = DIRECTION ( 'NONE',  ( -1.000000000000000000, -4.440892098500622217E-16, 0.000000000000000000 ) ) ;
#15393 = DIRECTION ( 'NONE',  ( -0.9510565162951536422, 0.000000000000000000, -0.3090169943749472292 ) ) ;
#15394 = ORIENTED_EDGE ( 'NONE', *, *, #10653, .T. ) ;
#15395 = CARTESIAN_POINT ( 'NONE',  ( 13.13063628947021755, 8.573956625762026107, -15.90631066800904669 ) ) ;
#15396 = VERTEX_POINT ( 'NONE', #6145 ) ;
#15397 = CARTESIAN_POINT ( 'NONE',  ( 13.40325769311605164, 6.909072298322937122, -18.40730773563142719 ) ) ;
#15398 = CARTESIAN_POINT ( 'NONE',  ( 22.08592964957147586, 4.518037853963432049, -19.67680751601638889 ) ) ;
#15399 = VECTOR ( 'NONE', #26042, 1000.000000000000000 ) ;
#15400 = CARTESIAN_POINT ( 'NONE',  ( 168.6922820468852819, -9.999999999999998224, 2.247092850131519715 ) ) ;
#15401 = VERTEX_POINT ( 'NONE', #24771 ) ;
#15402 = LINE ( 'NONE', #22444, #9350 ) ;
#15403 = AXIS2_PLACEMENT_3D ( 'NONE', #3588, #24342, #21896 ) ;
#15404 = CARTESIAN_POINT ( 'NONE',  ( 25.21413058671614849, -1.115224416820481457, -18.44856734933592080 ) ) ;
#15405 = VECTOR ( 'NONE', #24000, 1000.000000000000000 ) ;
#15406 = DIRECTION ( 'NONE',  ( 0.9510565162951535312, 2.566386769018988816E-16, -0.3090169943749475623 ) ) ;
#15407 = FACE_BOUND ( 'NONE', #17471, .T. ) ;
#15408 = EDGE_CURVE ( 'NONE', #21374, #2754, #24464, .T. ) ;
#15409 = ORIENTED_EDGE ( 'NONE', *, *, #5813, .T. ) ;
#15410 = EDGE_CURVE ( 'NONE', #8506, #12251, #11049, .T. ) ;
#15411 = EDGE_CURVE ( 'NONE', #23025, #24310, #28154, .T. ) ;
#15412 = CARTESIAN_POINT ( 'NONE',  ( -2.099999999999999645, -6.754115128641864009E-16, -2.144516984716112518 ) ) ;
#15413 = CARTESIAN_POINT ( 'NONE',  ( 35.07504771885155037, -20.05712364337910714, -20.21480690768607857 ) ) ;
#15414 = DIRECTION ( 'NONE',  ( 0.8660254037844353769, -0.5000000000000055511, 0.000000000000000000 ) ) ;
#15415 = EDGE_LOOP ( 'NONE', ( #4443, #20541, #24917, #26120 ) ) ;
#15416 = EDGE_LOOP ( 'NONE', ( #4181, #23361, #23477, #12663, #16504 ) ) ;
#15417 = FACE_OUTER_BOUND ( 'NONE', #20006, .T. ) ;
#15418 = AXIS2_PLACEMENT_3D ( 'NONE', #14379, #23716, #14534 ) ;
#15419 = CARTESIAN_POINT ( 'NONE',  ( 15.36220012886423447, 10.89358938796158149, -12.84895098869522201 ) ) ;
#15420 = CARTESIAN_POINT ( 'NONE',  ( 35.54859390953724585, -23.18451583373416014, -17.64281456791166391 ) ) ;
#15421 = CARTESIAN_POINT ( 'NONE',  ( 141.1922820468854525, -10.00000000000000533, -28.06379628232387446 ) ) ;
#15422 = VERTEX_POINT ( 'NONE', #19571 ) ;
#15423 = AXIS2_PLACEMENT_3D ( 'NONE', #25537, #28326, #660 ) ;
#15424 = DIRECTION ( 'NONE',  ( 0.000000000000000000, -0.000000000000000000, -1.000000000000000000 ) ) ;
#15425 = ORIENTED_EDGE ( 'NONE', *, *, #5333, .T. ) ;
#15426 = CIRCLE ( 'NONE', #2297, 13.00000000000000178 ) ;
#15427 = CARTESIAN_POINT ( 'NONE',  ( 10.71071464234916348, 8.878904022500222482, -16.39175934796422851 ) ) ;
#15428 = CARTESIAN_POINT ( 'NONE',  ( -1.310841663519413114, -1.387778780781445429E-16, 5.000000000000000000 ) ) ;
#15429 =( LENGTH_UNIT ( ) NAMED_UNIT ( * ) SI_UNIT ( .MILLI., .METRE. ) );
#15430 = ORIENTED_EDGE ( 'NONE', *, *, #22704, .F. ) ;
#15431 = DIRECTION ( 'NONE',  ( -1.000000000000000000, -4.440892098500622217E-16, 0.000000000000000000 ) ) ;
#15432 = ORIENTED_EDGE ( 'NONE', *, *, #4609, .F. ) ;
#15433 = CARTESIAN_POINT ( 'NONE',  ( 13.30397322184224329, 9.708587077508630259, -15.76815807330931030 ) ) ;
#15434 = CARTESIAN_POINT ( 'NONE',  ( 36.32827445255054499, -20.19473721995742821, -19.46526261299151983 ) ) ;
#15435 = CARTESIAN_POINT ( 'NONE',  ( 25.45462155318426767, -0.2439708902934435431, -15.99927030562601438 ) ) ;
#15436 = ORIENTED_EDGE ( 'NONE', *, *, #25290, .T. ) ;
#15437 = PRODUCT_DEFINITION_SHAPE ( 'NONE', 'NONE',  #30263 ) ;
#15438 = VERTEX_POINT ( 'NONE', #12546 ) ;
#15439 = LINE ( 'NONE', #19712, #23299 ) ;
#15440 = DIRECTION ( 'NONE',  ( -2.698458740408365879E-16, 1.000000000000000000, 0.000000000000000000 ) ) ;
#15441 = DIRECTION ( 'NONE',  ( 2.207829878515935943E-16, -1.000000000000000000, 0.000000000000000000 ) ) ;
#15442 = EDGE_CURVE ( 'NONE', #16324, #20167, #29236, .T. ) ;
#15443 = CARTESIAN_POINT ( 'NONE',  ( 23.87675077653036126, -6.787291307973906562, -13.16608595595566733 ) ) ;
#15444 = CARTESIAN_POINT ( 'NONE',  ( 19.75347561433959953, 2.650395817966514578, -13.58229691592852184 ) ) ;
#15445 = MECHANICAL_DESIGN_GEOMETRIC_PRESENTATION_REPRESENTATION (  '', ( #24242 ), #8622 ) ;
#15446 = ORIENTED_EDGE ( 'NONE', *, *, #18382, .F. ) ;
#15447 = ORIENTED_EDGE ( 'NONE', *, *, #101, .F. ) ;
#15448 = ORIENTED_EDGE ( 'NONE', *, *, #194, .F. ) ;
#15449 = CARTESIAN_POINT ( 'NONE',  ( 85.18867862981259975, -4.999999999999993783, 61.89319792914030671 ) ) ;
#15450 = VECTOR ( 'NONE', #19823, 1000.000000000000000 ) ;
#15451 = SURFACE_STYLE_FILL_AREA ( #6154 ) ;
#15452 = CARTESIAN_POINT ( 'NONE',  ( 167.2287565553228887, -4.999999999999972466, -3.509618943233414168 ) ) ;
#15453 = CARTESIAN_POINT ( 'NONE',  ( 167.0152310637605240, -9.999999999999996447, -34.70218595412750773 ) ) ;
#15454 = CARTESIAN_POINT ( 'NONE',  ( -7.999999999999996447, -3.867591403079198020, -4.502324684675412136 ) ) ;
#15455 = DIRECTION ( 'NONE',  ( -2.698458740408365879E-16, 1.000000000000000000, 0.000000000000000000 ) ) ;
#15456 = CARTESIAN_POINT ( 'NONE',  ( 11.23377902493292879, 9.047655202846097922, -17.23738383348171865 ) ) ;
#15457 = CARTESIAN_POINT ( 'NONE',  ( 12.49664108868010182, 8.569232744350554043, -15.13285098609708790 ) ) ;
#15458 = LINE ( 'NONE', #8587, #15576 ) ;
#15459 = LINE ( 'NONE', #24944, #7612 ) ;
#15460 = CARTESIAN_POINT ( 'NONE',  ( 0.000000000000000000, 55.00000000000000711, 0.000000000000000000 ) ) ;
#15461 = EDGE_LOOP ( 'NONE', ( #3525, #6017, #23635, #18962, #18226, #24542 ) ) ;
#15462 = CARTESIAN_POINT ( 'NONE',  ( 167.0152310637604955, -1.999999999999970912, -26.04193191628311155 ) ) ;
#15463 = CARTESIAN_POINT ( 'NONE',  ( -4.000000000000003553, -1.933795701539605227, -2.201162342337703137 ) ) ;
#15464 = LINE ( 'NONE', #10431, #12673 ) ;
#15466 = ORIENTED_EDGE ( 'NONE', *, *, #26745, .T. ) ;
#15465 = CARTESIAN_POINT ( 'NONE',  ( 24.79644250101478065, -1.608028467720058918, -19.02763285027648976 ) ) ;
#15467 = ORIENTED_EDGE ( 'NONE', *, *, #28149, .T. ) ;
#15468 = CARTESIAN_POINT ( 'NONE',  ( 152.0152310637604671, -4.999999999999976907, -1.687708096207001986E-14 ) ) ;
#15469 = CARTESIAN_POINT ( 'NONE',  ( 11.05541531668977662, 17.68942339022145305, -17.95086732675816776 ) ) ;
#15470 = AXIS2_PLACEMENT_3D ( 'NONE', #5735, #15018, #24348 ) ;
#15471 = DIRECTION ( 'NONE',  ( -0.8090169943749474513, -2.183098979609982436E-16, 0.5877852522924731371 ) ) ;
#15472 = CARTESIAN_POINT ( 'NONE',  ( 5.000000000000000888, 4.250000000000003553, 0.000000000000000000 ) ) ;
#15473 = EDGE_LOOP ( 'NONE', ( #26878, #19257, #8189, #25216 ) ) ;
#15474 = CARTESIAN_POINT ( 'NONE',  ( 24.43075134246613800, -6.859861339260811874, -14.00379227226492951 ) ) ;
#15475 = CARTESIAN_POINT ( 'NONE',  ( 118.9351296419579995, -4.999999999999985789, -86.41142975871350984 ) ) ;
#15476 = CARTESIAN_POINT ( 'NONE',  ( 21.70429774405079115, -3.429840324723197664, -17.59459576866303365 ) ) ;
#15477 = ORIENTED_EDGE ( 'NONE', *, *, #11476, .F. ) ;
#15478 = CARTESIAN_POINT ( 'NONE',  ( 35.54859390953724585, -22.18451583373416014, -17.78191007148576475 ) ) ;
#15479 = EDGE_CURVE ( 'NONE', #21374, #24767, #8270, .T. ) ;
#15480 = ORIENTED_EDGE ( 'NONE', *, *, #5290, .F. ) ;
#15481 =( NAMED_UNIT ( * ) PLANE_ANGLE_UNIT ( ) SI_UNIT ( $, .RADIAN. ) );
#15482 = CARTESIAN_POINT ( 'NONE',  ( 27.18523481531828168, -13.05407500640787077, -12.66260957699712186 ) ) ;
#15483 = CARTESIAN_POINT ( 'NONE',  ( 21.21264933382939333, -0.1440395243212932441, -13.28659446924270959 ) ) ;
#15484 = ORIENTED_EDGE ( 'NONE', *, *, #9162, .F. ) ;
#15485 = CARTESIAN_POINT ( 'NONE',  ( 31.22280883588763700, -10.09333740185288875, -13.86128061636125786 ) ) ;
#15486 = AXIS2_PLACEMENT_3D ( 'NONE', #21208, #4886, #14181 ) ;
#15487 = DIRECTION ( 'NONE',  ( 0.9510565162951536422, 0.000000000000000000, -0.3090169943749475623 ) ) ;
#15488 = VERTEX_POINT ( 'NONE', #26619 ) ;
#15489 = DIRECTION ( 'NONE',  ( -0.9510565162951536422, -2.566386769018988816E-16, -0.3090169943749472292 ) ) ;
#15490 = AXIS2_PLACEMENT_3D ( 'NONE', #9007, #13449, #2180 ) ;
#15491 = LINE ( 'NONE', #6351, #20361 ) ;
#15492 = DIRECTION ( 'NONE',  ( 0.5877852522924731371, 1.586114251531760728E-16, 0.8090169943749474513 ) ) ;
#15493 = DIRECTION ( 'NONE',  ( 0.000000000000000000, -2.775557561562890735E-17, 1.000000000000000000 ) ) ;
#15494 = CARTESIAN_POINT ( 'NONE',  ( 27.00779440489029071, -4.779404007149373079, -14.88408750732950914 ) ) ;
#15495 = CARTESIAN_POINT ( 'NONE',  ( 16.22940209442605308, 10.22534693890197133, -14.12725775589269084 ) ) ;
#15496 = CARTESIAN_POINT ( 'NONE',  ( 35.76309413546784555, -19.65568143964299352, -21.39484760613106573 ) ) ;
#15497 = DIRECTION ( 'NONE',  ( -0.9510565162951536422, 0.000000000000000000, -0.3090169943749472292 ) ) ;
#15498 = CARTESIAN_POINT ( 'NONE',  ( 11.55687758731922798, 9.016417257711555777, -15.81607864292198329 ) ) ;
#15499 = CARTESIAN_POINT ( 'NONE',  ( 141.1922820468854525, -10.00000000000000533, -22.25671179336495697 ) ) ;
#15500 = CARTESIAN_POINT ( 'NONE',  ( 13.15390973649967599, 8.859676595473322536, -14.60899741038990562 ) ) ;
#15501 = CARTESIAN_POINT ( 'NONE',  ( 13.23272240178861381, 8.619070305187777947, -15.82494623455082916 ) ) ;
#15502 = CARTESIAN_POINT ( 'NONE',  ( 1.310872448937984602, -8.480771745766441327, -4.682649155111321626 ) ) ;
#15503 = CARTESIAN_POINT ( 'NONE',  ( 154.5152310637605808, -4.999999999999976019, -28.60870317832789667 ) ) ;
#15504 = CARTESIAN_POINT ( 'NONE',  ( 11.47181023233108021, 9.274170903235749108, -15.86135313853478657 ) ) ;
#15505 = ORIENTED_EDGE ( 'NONE', *, *, #18265, .F. ) ;
#15506 = LINE ( 'NONE', #27002, #22719 ) ;
#15507 = DIRECTION ( 'NONE',  ( 0.3090169943749475623, 8.338696094058001131E-17, 0.9510565162951536422 ) ) ;
#15508 = ORIENTED_EDGE ( 'NONE', *, *, #15201, .F. ) ;
#15509 = AXIS2_PLACEMENT_3D ( 'NONE', #21515, #21657, #21816 ) ;
#15510 = CARTESIAN_POINT ( 'NONE',  ( 31.88113401528661939, -11.03952345999570994, -14.96145667752709763 ) ) ;
#15511 = ORIENTED_EDGE ( 'NONE', *, *, #7240, .F. ) ;
#15512 = CARTESIAN_POINT ( 'NONE',  ( 8.944585970659694851, 16.95158685720792846, -17.91243444582771005 ) ) ;
#15513 = CARTESIAN_POINT ( 'NONE',  ( 36.06101586692013683, -20.99408596552883566, -21.31372499146719690 ) ) ;
#15514 = ADVANCED_FACE ( 'NONE', ( #5699 ), #12702, .T. ) ;
#15515 = ADVANCED_FACE ( 'NONE', ( #26777 ), #1428, .T. ) ;
#15516 = CIRCLE ( 'NONE', #2380, 4.187999999999997947 ) ;
#15517 = CARTESIAN_POINT ( 'NONE',  ( 21.96101381878726500, 3.467707295883769802, -19.37612211972275844 ) ) ;
#15518 = EDGE_CURVE ( 'NONE', #23642, #12834, #22023, .T. ) ;
#15519 = CARTESIAN_POINT ( 'NONE',  ( 30.07542022419311678, -8.155067017681195907, -14.09159111155252120 ) ) ;
#15520 = DIRECTION ( 'NONE',  ( -2.698458740408365879E-16, 1.000000000000000000, 0.000000000000000000 ) ) ;
#15521 = DIRECTION ( 'NONE',  ( -0.8090169943749474513, -2.183098979609982436E-16, 0.5877852522924731371 ) ) ;
#15522 = EDGE_CURVE ( 'NONE', #15063, #17767, #17429, .T. ) ;
#15523 = VECTOR ( 'NONE', #18749, 999.9999999999998863 ) ;
#15524 = CARTESIAN_POINT ( 'NONE',  ( 5.637851296924623057E-15, 9.237604307034036566, -4.285468820183664818 ) ) ;
#15525 = CARTESIAN_POINT ( 'NONE',  ( 22.41093758190154972, 3.143874582428516806, -16.84310506638757943 ) ) ;
#15526 = ORIENTED_EDGE ( 'NONE', *, *, #3036, .T. ) ;
#15527 = ORIENTED_EDGE ( 'NONE', *, *, #8149, .T. ) ;
#15528 = DIRECTION ( 'NONE',  ( 0.000000000000000000, -2.775557561562890735E-17, 1.000000000000000000 ) ) ;
#15529 = DIRECTION ( 'NONE',  ( -1.000000000000000000, 0.000000000000000000, 0.000000000000000000 ) ) ;
#15530 = APPLICATION_CONTEXT ( 'automotive_design' ) ;
#15531 =( NAMED_UNIT ( * ) SI_UNIT ( $, .STERADIAN. ) SOLID_ANGLE_UNIT ( ) );
#15532 = FACE_OUTER_BOUND ( 'NONE', #10016, .T. ) ;
#15533 = CARTESIAN_POINT ( 'NONE',  ( 12.35422140817580683, 8.720385185214494683, -16.48779044034850116 ) ) ;
#15534 = CARTESIAN_POINT ( 'NONE',  ( 35.52138705868412671, -21.06228986472472897, -18.81697501280657647 ) ) ;
#15535 = VECTOR ( 'NONE', #17801, 1000.000000000000000 ) ;
#15536 = ORIENTED_EDGE ( 'NONE', *, *, #11037, .F. ) ;
#15537 = CARTESIAN_POINT ( 'NONE',  ( 9.111161770198492604, 16.18764900704733378, -17.05531488649033633 ) ) ;
#15538 = ORIENTED_EDGE ( 'NONE', *, *, #8168, .F. ) ;
#15539 = CARTESIAN_POINT ( 'NONE',  ( 24.62590367393082502, -9.567571807129121808, -15.85044010117769098 ) ) ;
#15540 = CARTESIAN_POINT ( 'NONE',  ( 10.35864918915110877, 16.97212501191939538, -17.93331994345748370 ) ) ;
#15541 = LINE ( 'NONE', #2280, #23887 ) ;
#15542 = VECTOR ( 'NONE', #4576, 1000.000000000000000 ) ;
#15543 = VECTOR ( 'NONE', #17579, 1000.000000000000000 ) ;
#15544 = ORIENTED_EDGE ( 'NONE', *, *, #9058, .F. ) ;
#15545 = CARTESIAN_POINT ( 'NONE',  ( 134.7287565553230024, -1.999999999999980460, -33.82050807568879947 ) ) ;
#15546 = DIRECTION ( 'NONE',  ( -1.000000000000000000, 0.000000000000000000, -0.000000000000000000 ) ) ;
#15547 = DIRECTION ( 'NONE',  ( -1.110223024625156540E-16, 0.000000000000000000, -1.000000000000000000 ) ) ;
#15548 = FACE_OUTER_BOUND ( 'NONE', #28778, .T. ) ;
#15549 = EDGE_LOOP ( 'NONE', ( #13308, #11638, #28700, #26377, #10701, #15563 ) ) ;
#15550 = CARTESIAN_POINT ( 'NONE',  ( 9.661883061612440926, 16.25482663361732705, -17.92454625180715411 ) ) ;
#15551 = CARTESIAN_POINT ( 'NONE',  ( 16.54285080251403173, 3.669380853427548939, -13.47387114519368012 ) ) ;
#15552 = CARTESIAN_POINT ( 'NONE',  ( 18.76724195421386554, 7.045283186750163296, -20.62625128596355495 ) ) ;
#15553 = EDGE_CURVE ( 'NONE', #14407, #20918, #13605, .T. ) ;
#15554 = DIRECTION ( 'NONE',  ( 0.5877852522924731371, 0.000000000000000000, 0.8090169943749474513 ) ) ;
#15555 = ADVANCED_FACE ( 'NONE', ( #8717 ), #6450, .F. ) ;
#15556 = CARTESIAN_POINT ( 'NONE',  ( 172.0152310637604955, -9.999999999999994671, -24.27857615940569502 ) ) ;
#15557 = VECTOR ( 'NONE', #18192, 1000.000000000000000 ) ;
#15558 = CARTESIAN_POINT ( 'NONE',  ( 21.79935899731381710, -1.430375723040585356, -13.25318265510616733 ) ) ;
#15559 = EDGE_CURVE ( 'NONE', #8863, #2025, #4605, .T. ) ;
#15560 = AXIS2_PLACEMENT_3D ( 'NONE', #12937, #1209, #3497 ) ;
#15561 = CARTESIAN_POINT ( 'NONE',  ( 153.6922820468854525, -10.00000000000000000, -35.24709285013155835 ) ) ;
#15562 = DIRECTION ( 'NONE',  ( -2.698458740408365879E-16, 1.000000000000000000, 0.000000000000000000 ) ) ;
#15563 = ORIENTED_EDGE ( 'NONE', *, *, #29485, .F. ) ;
#15564 = CARTESIAN_POINT ( 'NONE',  ( 166.1922820468853672, -9.999999999999996447, -28.06379628232387802 ) ) ;
#15565 = CARTESIAN_POINT ( 'NONE',  ( 33.40713826534622655, -12.56408340279653757, -19.71064172033093698 ) ) ;
#15566 = DIRECTION ( 'NONE',  ( 0.3090169943749472292, 8.338696094057992503E-17, -0.9510565162951536422 ) ) ;
#15567 = ORIENTED_EDGE ( 'NONE', *, *, #548, .F. ) ;
#15568 = DIRECTION ( 'NONE',  ( 0.5877852522924731371, 0.000000000000000000, 0.8090169943749474513 ) ) ;
#15569 = PRODUCT_DEFINITION_CONTEXT ( 'detailed design', #18251, 'design' ) ;
#15570 = CARTESIAN_POINT ( 'NONE',  ( 12.24552273913795730, 9.516269270964150095, -15.33299823368393078 ) ) ;
#15571 = CARTESIAN_POINT ( 'NONE',  ( 33.29928106196997817, -12.14339677642331772, -19.64090527578606427 ) ) ;
#15572 = VECTOR ( 'NONE', #19363, 1000.000000000000000 ) ;
#15573 =( BOUNDED_SURFACE ( )  B_SPLINE_SURFACE ( 3, 3, ( 
 ( #1564, #29381, #20152, #20301, #29690, #4142, #4591, #5035, #18926, #6734, #14326, #2321, #25955, #20750, #9303, #7035, #18473, #14180, #321, #25804, #9449, #23356, #21207, #30139, #4444, #11890, #6893, #18773, #7185, #13739, #28280, #28126, #23066, #9145, #9607, #4885, #7337, #23507, #27827, #2617, #15, #16478, #16636, #23661, #16026, #2165, #18628, #16327, #16183, #27976, #2765, #12049, #29987, #25643, #8997, #18315, #11439, #25502, #13880, #169, #20904, #27673, #23203, #2472, #11591, #4735, #25351, #14028, #11746, #21064, #21656, #10785, #27150, #1340, #3774, #10629, #20093, #29470, #7776, #22391, #28572, #23820, #16931, #6213, #16783, #2917, #8488, #12199, #7625, #26262, #27000, #22229, #5344, #21514, #469, #9756, #19076, #6061, #17791, #15347, #19939, #28428, #17643, #620, #26412, #757, #15504, #12344, #9905, #21362, #24835, #19214, #29307, #5491, #10053, #8341, #17087, #14631, #3926, #24684, #7480, #14774, #13068, #23978, #3070, #19368, #28730, #24116, #1496, #26111, #3214, #12914, #5186, #14483, #13671, #11082, #11232, #22848, #27602, #18402, #6662, #2098, #15804, #4075, #8636, #17938, #1949, #25429, #30064, #9075, #27754, #6814, #27908, #24993, #22996, #22693, #29773, #8929, #15954, #16108, #13369, #20383, #11375, #8783, #1794, #22548, #1646, #10925, #4519, #20831, #13807, #20679, #20233, #23135, #18098, #18247, #20535, #18551, #4221, #27462, #13226, #30214, #6514, #2244, #25281, #13518 ),
 ( #4370, #11517, #25131, #29922, #9223, #15660, #6966, #16254, #25567, #29622, #27312, #6366, #23441, #5116, #2553, #2689, #14257, #19008, #9843, #28366, #23749, #7264, #25732, #95, #9380, #23589, #16863, #21447, #558, #19155, #28512, #19300, #16409, #14409, #14108, #21140, #399, #7421, #7561, #4814, #11824, #14561, #26195, #23909, #5274, #251, #3004, #4967, #12132, #12282, #21601, #20988, #28053, #11970, #21289, #9527, #9683, #698, #9985, #2846, #16721, #28659, #7712, #18706, #7107, #18850, #17021, #25889, #4660, #28211, #26041, #16566, #13955, #23287, #2398, #11672, #24200, #26651, #15310, #1459, #5881, #8303, #15162, #24643, #3738, #12732, #26966, #3302, #28821, #21897, #10749, #21746, #7859, #13036, #17168, #12577, #1011, #1303, #10290, #26497, #5578, #19903, #22353, #19598, #14860, #5426, #28967, #26809, #8003, #24343, #5730, #10435, #10593, #19744, #24498, #17311, #15013, #848, #10138, #3439, #17610, #12879, #22193, #29269, #6027, #20057, #22054, #3589, #1156, #29113, #8154, #17460, #29431, #8450, #26345, #14712, #24055, #3155, #12428, #19452, #20644, #18062, #25244, #9038, #16069, #3890, #10888, #27425, #25093, #6328, #15769, #11340, #30030, #27568, #4183, #13777, #20797, #22512, #20199, #1612, #18211, #8745, #18361, #15624, #11192, #29582, #8599, #30182, #13477, #25395, #24958, #6480, #6776, #23105, #6623, #27718, #15915, #4486, #2208, #22808, #11482, #4038, #17898, #13332, #17758, #13189 ),
 ( #4333, #22656, #27279, #27114, #6175, #15469, #22959, #24800, #2061, #13629, #1756, #11046, #20347, #1914, #20501, #29738, #29887, #8896, #9191, #16823, #61, #9651, #14223, #213, #18971, #25853, #4783, #23867, #7385, #2966, #23554, #23708, #9345, #14073, #2656, #18815, #14524, #9491, #18672, #18516, #26157, #28017, #28328, #11932, #28173, #16680, #4932, #23402, #12244, #26003, #21562, #21254, #2810, #7076, #2519, #11787, #11637, #20950, #12093, #5231, #21107, #16371, #27876, #25692, #5079, #7230, #16530, #365, #14370, #21410, #514, #9805, #19117, #28473, #4630, #13922, #7521, #6931, #16224, #25538, #23253, #2365, #15274, #12390, #1123, #10097, #17131, #26609, #14971, #15123, #807, #7823, #10552, #5839, #19862, #24456, #19411, #3551, #967, #8115, #22155, #29225, #16979, #24018, #10248, #7966, #28781, #28930, #12843, #1265, #10401, #17275, #26925, #3697, #5388, #3118, #14674, #19708, #21855, #8262, #26458, #24306, #21702, #5539, #12999, #5692, #17571, #14824, #19563, #5985, #24606, #29072, #661, #17420, #9946, #19259, #3401, #28615, #24159, #3263, #12538, #7672, #26305, #12694, #22015, #26768, #29542, #8560, #27536, #22773, #17862, #13149, #1419, #10709, #20018, #6590, #29999, #15879, #1879, #29388, #18178, #22473, #4301, #27078, #11308, #8412, #25210, #20611, #27681, #27391, #13600, #17719, #27237, #11159, #15734, #9003, #6135, #18323, #16033, #6287, #20465, #15433, #22928, #24763, #2028, #6741 ),
 ( #29697, #10850, #20308, #25359, #4452, #29854, #8710, #22311, #3851, #1571, #20159, #15584, #8860, #13299, #24918, #4000, #25061, #22618, #1717, #11003, #18026, #6445, #4148, #13442, #2773, #19083, #23515, #25962, #2625, #12056, #21369, #179, #14334, #20912, #16191, #9312, #28435, #9153, #25509, #476, #4599, #25, #18638, #18934, #14188, #27984, #13887, #23074, #2173, #11449, #28289, #9766, #7344, #11900, #20757, #9614, #23214, #18782, #23364, #7487, #4745, #2330, #13746, #16791, #11599, #21216, #28135, #14036, #330, #9458, #7044, #26118, #16643, #30146, #7193, #5042, #16335, #25652, #2481, #11754, #21072, #23669, #18480, #16488, #25812, #27837, #4894, #6900, #3082, #3221, #14784, #19527, #10366, #28898, #24272, #7784, #26270, #627, #23828, #14490, #19671, #12811, #29036, #14936, #2924, #1089, #5351, #10214, #24124, #10512, #26419, #14638, #5196, #22125, #23985, #5654, #7929, #5498, #3370, #21822, #765, #19825, #12657, #29189, #17240, #8075, #12351, #10061, #19375, #7633, #16940, #17384, #1228, #28739, #21664, #12206, #17094, #21976, #12499, #923, #26571, #26729, #5802, #15084, #24423, #3518, #8226, #9912, #19223, #17535, #21525, #28579, #22737, #13411, #1848, #11274, #8380, #27356, #6101, #13111, #22586, #10967, #11128, #27046, #3817, #6554, #20429, #15845, #29820, #15395, #8828, #27203, #4116, #18142, #25175, #12959, #19983, #6255, #3970, #24729, #24884, #27503, #4266, #6413, #13269, #22892 ),
 ( #13567, #22436, #20277, #1384, #10675, #8970, #1686, #1994, #1538, #15550, #20578, #29964, #15702, #26891, #25031, #5956, #15244, #29663, #24576, #10821, #29355, #20130, #3664, #22274, #17687, #29510, #8531, #17832, #8678, #17984, #18744, #25469, #9115, #27643, #18597, #25773, #9571, #16606, #4419, #11415, #27948, #25605, #6863, #16293, #11865, #21177, #28090, #4703, #14299, #21330, #23038, #20720, #2140, #7151, #9268, #289, #16151, #11714, #30107, #18447, #437, #13995, #25928, #4560, #7005, #7302, #23633, #16451, #18893, #4852, #5009, #2731, #23324, #28252, #13848, #27797, #23175, #12015, #13713, #2287, #18286, #11557, #20874, #30256, #23480, #14153, #2438, #21033, #6709, #15999, #25328, #2589, #139, #9419, #19493, #7456, #5617, #9878, #14752, #19338, #15052, #728, #19190, #9724, #17349, #593, #10181, #24090, #10024, #28863, #26387, #5314, #24385, #7899, #3484, #3190, #24239, #28545, #14598, #23950, #12169, #21488, #3339, #26695, #3043, #7597, #19047, #16903, #17208, #26233, #7750, #28702, #12467, #14897, #21789, #26537, #12315, #21631, #5162, #14452, #17059, #21939, #12620, #1052, #10330, #19637, #12775, #5464, #29003, #889, #8042, #5770, #22092, #28402, #16758, #26081, #23790, #2886, #20390, #15667, #19947, #4083, #13376, #10637, #6068, #22700, #1807, #11089, #10476, #29314, #29781, #25000, #8498, #13235, #8789, #15354, #6522, #18106, #8192, #15812, #3780, #27468, #22238, #10793, #17797, #8348 ),
 ( #1349, #5923, #25137, #17650, #10932, #8642, #15209, #4228, #20243, #24541, #27012, #24693, #13529, #3629, #6219, #12922, #1196, #13077, #19787, #17503, #29152, #26854, #22400, #15512, #6376, #1503, #20100, #29630, #24846, #29478, #27159, #3932, #22556, #1654, #17945, #27320, #2816, #8938, #12099, #14376, #23713, #2973, #21416, #28336, #18254, #19123, #27760, #13678, #6672, #14530, #2253, #20838, #23873, #22854, #26009, #522, #25436, #1956, #9810, #370, #9085, #15961, #30073, #11238, #18410, #4527, #7390, #6827, #23004, #9657, #16115, #28480, #5238, #20687, #13815, #7526, #11383, #18978, #25291, #20542, #23143, #29931, #11526, #16686, #27609, #4380, #5088, #16832, #26162, #2106, #12838, #3394, #21849, #959, #10241, #17714, #20154, #27072, #10395, #22150, #1565, #17858, #22305, #24759, #1411, #10845, #29536, #29218, #13138, #19703, #14965, #8106, #27231, #7959, #24299, #8554, #12687, #29067, #6281, #3691, #22467, #1258, #22009, #19556, #28924, #17268, #6130, #15577, #15427, #10704, #26598, #8407, #1116, #17565, #10545, #24909, #3544, #17414, #12531, #5685, #26761, #12993, #26918, #19853, #20013, #8255, #5831, #15117, #29383, #24450, #5980, #3845, #15269, #24600, #8854, #6437, #15728, #27829, #20906, #27530, #22767, #13293, #1874, #4445, #11154, #2021, #13595, #18317, #9146, #27675, #23068, #6584, #25057, #29691, #8704, #22921, #16184, #20752, #30140, #18474, #6894, #18630, #4143, #13740, #13437, #20457 ),
 ( #18169, #2167, #10996, #25503, #18018, #4593, #13881, #23206, #16329, #2323, #11441, #27384, #11593, #15873, #29848, #25204, #27978, #29990, #6735, #7038, #3994, #18, #9306, #4295, #22612, #1710, #8998, #11302, #20605, #16028, #20303, #25352, #28283, #7482, #7339, #16933, #3075, #23509, #25957, #622, #4888, #9759, #171, #759, #9609, #10056, #14182, #11893, #14633, #7778, #16638, #16786, #19078, #9452, #12346, #2475, #9907, #2619, #21209, #12051, #2919, #25646, #28574, #324, #18928, #26265, #5346, #23980, #4738, #5037, #21659, #19217, #2768, #26113, #7628, #14329, #19370, #28732, #11748, #14030, #23663, #23358, #16481, #21364, #471, #28430, #21066, #18775, #21518, #5189, #14485, #28129, #25806, #7187, #23822, #12201, #26886, #24571, #917, #6096, #5950, #21817, #17235, #24267, #15391, #19522, #22120, #28893, #29350, #10206, #24725, #3216, #1377, #3812, #22431, #1222, #22268, #14778, #3365, #15236, #10506, #13105, #7924, #1534, #10816, #21970, #3659, #24119, #10670, #26565, #19977, #12954, #8374, #29506, #17682, #17529, #5649, #20126, #29031, #14931, #12651, #17089, #12806, #19819, #26414, #5493, #27039, #12494, #17379, #1084, #10361, #29184, #19665, #8069, #26724, #5797, #15078, #24418, #8221, #3512, #10963, #22886, #1989, #13709, #11269, #27638, #11123, #29659, #3966, #13263, #18134, #20715, #25321, #4414, #23034, #2136, #23171, #20271, #8965, #17979, #25026, #4260, #20572, #11410, #8674, #15696 ) ),
 .UNSPECIFIED., .T., .F., .F. ) 
 B_SPLINE_SURFACE_WITH_KNOTS ( ( 4, 3, 4 ),
 ( 4, 2, 2, 2, 2, 2, 2, 2, 2, 2, 2, 2, 2, 2, 2, 2, 2, 2, 2, 2, 2, 2, 2, 2, 2, 2, 2, 2, 2, 2, 2, 2, 2, 2, 2, 2, 2, 2, 2, 2, 2, 2, 2, 2, 2, 2, 2, 2, 2, 2, 2, 2, 2, 2, 2, 2, 2, 2, 2, 2, 2, 2, 2, 2, 2, 2, 2, 2, 2, 2, 2, 2, 2, 2, 2, 2, 2, 2, 2, 2, 2, 2, 2, 2, 2, 2, 2, 2, 2, 2, 2, 2, 4 ),
 ( 0.000000000000000000, 0.5000000000000000000, 1.000000000000000000 ),
 ( 0.000000000000000000, 0.2329478137359916323, 0.2349098735327962983, 0.2358909034311986175, 0.2363814183803997770, 0.2366266758550003568, 0.2367493045923006467, 0.2368106189609507917, 0.2368719333296009644, 0.2369056680493116240, 0.2369394027690223115, 0.2370068722084436863, 0.2371418110872863805, 0.2374116888449718243, 0.2379514443603427121, 0.2390309553910844875, 0.2411899774525679829, 0.2455080215755349737, 0.2541441098214689553, 0.2714162863133369186, 0.2886884628052048818, 0.2973245510511388634, 0.3016425951741058542, 0.3038016172355893496, 0.3048811282663310696, 0.3054208837817019573, 0.3056907615393874011, 0.3058257004182300953, 0.3058931698576514702, 0.3059269045773621576, 0.3059606392970728450, 0.3060023410584322145, 0.3060440428197915841, 0.3061274463425103787, 0.3062942533879479123, 0.3066278674788229797, 0.3072950956605731143, 0.3086295520240733836, 0.3112984647510739222, 0.3166362902050750550, 0.3273119411130772649, 0.3486632429290816293, 0.3913658465610904136, 0.4767710538251080377, 0.5621762610891256617, 0.6048788647211345015, 0.6262301665371388104, 0.6369058174451409648, 0.6422436428991420421, 0.6449125556261425807, 0.6462470119896428500, 0.6469142401713929846, 0.6472478542622681630, 0.6474146613077056411, 0.6474980648304244912, 0.6475397665917839163, 0.6475814683531432303, 0.6476196945210073164, 0.6476579206888715134, 0.6477343730245996856, 0.6478872776960560298, 0.6481930870389687183, 0.6488047057247940952, 0.6500279430964450711, 0.6524744178397468009, 0.6573673673263502604, 0.6671532662995571794, 0.6769391652727642095, 0.6867250642459712395, 0.6965109632191782696, 0.7062968621923852997, 0.7160827611655922187, 0.7209757106521956782, 0.7234221853954974080, 0.7246454227671483839, 0.7252570414529737608, 0.7255628507958864493, 0.7257157554673427935, 0.7257922078030709656, 0.7258304339709351627, 0.7258686601387992487, 0.7259088784260310234, 0.7259490967132626871, 0.7260295332877260144, 0.7261904064366526690, 0.7265121527345062002, 0.7271556453302130407, 0.7284426305216267217, 0.7310166009044543056, 0.7361645416701092515, 0.7464604232014193652, 0.7670521862640395927, 1.000000000000000000 ),
 .UNSPECIFIED. ) 
 GEOMETRIC_REPRESENTATION_ITEM ( )  RATIONAL_B_SPLINE_SURFACE ( (
 ( 1.000000000000000000, 1.000000000000000000, 1.000000000000000000, 1.000000000000000000, 1.000000000000000000, 1.000000000000000000, 1.000000000000000000, 1.000000000000000000, 1.000000000000000000, 1.000000000000000000, 1.000000000000000000, 1.000000000000000000, 1.000000000000000000, 1.000000000000000000, 1.000000000000000000, 1.000000000000000000, 1.000000000000000000, 1.000000000000000000, 1.000000000000000000, 1.000000000000000000, 1.000000000000000000, 1.000000000000000000, 1.000000000000000000, 1.000000000000000000, 1.000000000000000000, 1.000000000000000000, 1.000000000000000000, 1.000000000000000000, 1.000000000000000000, 1.000000000000000000, 1.000000000000000000, 1.000000000000000000, 1.000000000000000000, 1.000000000000000000, 1.000000000000000000, 1.000000000000000000, 1.000000000000000000, 1.000000000000000000, 1.000000000000000000, 1.000000000000000000, 1.000000000000000000, 1.000000000000000000, 1.000000000000000000, 1.000000000000000000, 1.000000000000000000, 1.000000000000000000, 1.000000000000000000, 1.000000000000000000, 1.000000000000000000, 1.000000000000000000, 1.000000000000000000, 1.000000000000000000, 1.000000000000000000, 1.000000000000000000, 1.000000000000000000, 1.000000000000000000, 1.000000000000000000, 1.000000000000000000, 1.000000000000000000, 1.000000000000000000, 1.000000000000000000, 1.000000000000000000, 1.000000000000000000, 1.000000000000000000, 1.000000000000000000, 1.000000000000000000, 1.000000000000000000, 1.000000000000000000, 1.000000000000000000, 1.000000000000000000, 1.000000000000000000, 1.000000000000000000, 1.000000000000000000, 1.000000000000000000, 1.000000000000000000, 1.000000000000000000, 1.000000000000000000, 1.000000000000000000, 1.000000000000000000, 1.000000000000000000, 1.000000000000000000, 1.000000000000000000, 1.000000000000000000, 1.000000000000000000, 1.000000000000000000, 1.000000000000000000, 1.000000000000000000, 1.000000000000000000, 1.000000000000000000, 1.000000000000000000, 1.000000000000000000, 1.000000000000000000, 1.000000000000000000, 1.000000000000000000, 1.000000000000000000, 1.000000000000000000, 1.000000000000000000, 1.000000000000000000, 1.000000000000000000, 1.000000000000000000, 1.000000000000000000, 1.000000000000000000, 1.000000000000000000, 1.000000000000000000, 1.000000000000000000, 1.000000000000000000, 1.000000000000000000, 1.000000000000000000, 1.000000000000000000, 1.000000000000000000, 1.000000000000000000, 1.000000000000000000, 1.000000000000000000, 1.000000000000000000, 1.000000000000000000, 1.000000000000000000, 1.000000000000000000, 1.000000000000000000, 1.000000000000000000, 1.000000000000000000, 1.000000000000000000, 1.000000000000000000, 1.000000000000000000, 1.000000000000000000, 1.000000000000000000, 1.000000000000000000, 1.000000000000000000, 1.000000000000000000, 1.000000000000000000, 1.000000000000000000, 1.000000000000000000, 1.000000000000000000, 1.000000000000000000, 1.000000000000000000, 1.000000000000000000, 1.000000000000000000, 1.000000000000000000, 1.000000000000000000, 1.000000000000000000, 1.000000000000000000, 1.000000000000000000, 1.000000000000000000, 1.000000000000000000, 1.000000000000000000, 1.000000000000000000, 1.000000000000000000, 1.000000000000000000, 1.000000000000000000, 1.000000000000000000, 1.000000000000000000, 1.000000000000000000, 1.000000000000000000, 1.000000000000000000, 1.000000000000000000, 1.000000000000000000, 1.000000000000000000, 1.000000000000000000, 1.000000000000000000, 1.000000000000000000, 1.000000000000000000, 1.000000000000000000, 1.000000000000000000, 1.000000000000000000, 1.000000000000000000, 1.000000000000000000, 1.000000000000000000, 1.000000000000000000, 1.000000000000000000, 1.000000000000000000, 1.000000000000000000, 1.000000000000000000, 1.000000000000000000, 1.000000000000000000, 1.000000000000000000, 1.000000000000000000, 1.000000000000000000, 1.000000000000000000, 1.000000000000000000, 1.000000000000000000, 1.000000000000000000, 1.000000000000000000, 1.000000000000000000, 1.000000000000000000, 1.000000000000000000, 1.000000000000000000, 1.000000000000000000),
 ( 0.3333333333333333703, 0.3333333333333333703, 0.3333333333333333703, 0.3333333333333333703, 0.3333333333333333703, 0.3333333333333333703, 0.3333333333333333703, 0.3333333333333333703, 0.3333333333333333703, 0.3333333333333333703, 0.3333333333333333703, 0.3333333333333333703, 0.3333333333333333703, 0.3333333333333333703, 0.3333333333333333703, 0.3333333333333333703, 0.3333333333333333703, 0.3333333333333333703, 0.3333333333333333703, 0.3333333333333333703, 0.3333333333333333703, 0.3333333333333333703, 0.3333333333333333703, 0.3333333333333333703, 0.3333333333333333703, 0.3333333333333333703, 0.3333333333333333703, 0.3333333333333333703, 0.3333333333333333703, 0.3333333333333333703, 0.3333333333333333703, 0.3333333333333333703, 0.3333333333333333703, 0.3333333333333333703, 0.3333333333333333703, 0.3333333333333333703, 0.3333333333333333703, 0.3333333333333333703, 0.3333333333333333703, 0.3333333333333333703, 0.3333333333333333703, 0.3333333333333333703, 0.3333333333333333703, 0.3333333333333333703, 0.3333333333333333703, 0.3333333333333333703, 0.3333333333333333703, 0.3333333333333333703, 0.3333333333333333703, 0.3333333333333333703, 0.3333333333333333703, 0.3333333333333333703, 0.3333333333333333703, 0.3333333333333333703, 0.3333333333333333703, 0.3333333333333333703, 0.3333333333333333703, 0.3333333333333333703, 0.3333333333333333703, 0.3333333333333333703, 0.3333333333333333703, 0.3333333333333333703, 0.3333333333333333703, 0.3333333333333333703, 0.3333333333333333703, 0.3333333333333333703, 0.3333333333333333703, 0.3333333333333333703, 0.3333333333333333703, 0.3333333333333333703, 0.3333333333333333703, 0.3333333333333333703, 0.3333333333333333703, 0.3333333333333333703, 0.3333333333333333703, 0.3333333333333333703, 0.3333333333333333703, 0.3333333333333333703, 0.3333333333333333703, 0.3333333333333333703, 0.3333333333333333703, 0.3333333333333333703, 0.3333333333333333703, 0.3333333333333333703, 0.3333333333333333703, 0.3333333333333333703, 0.3333333333333333703, 0.3333333333333333703, 0.3333333333333333703, 0.3333333333333333703, 0.3333333333333333703, 0.3333333333333333703, 0.3333333333333333703, 0.3333333333333333703, 0.3333333333333333703, 0.3333333333333333703, 0.3333333333333333703, 0.3333333333333333703, 0.3333333333333333703, 0.3333333333333333703, 0.3333333333333333703, 0.3333333333333333703, 0.3333333333333333703, 0.3333333333333333703, 0.3333333333333333703, 0.3333333333333333703, 0.3333333333333333703, 0.3333333333333333703, 0.3333333333333333703, 0.3333333333333333703, 0.3333333333333333703, 0.3333333333333333703, 0.3333333333333333703, 0.3333333333333333703, 0.3333333333333333703, 0.3333333333333333703, 0.3333333333333333703, 0.3333333333333333703, 0.3333333333333333703, 0.3333333333333333703, 0.3333333333333333703, 0.3333333333333333703, 0.3333333333333333703, 0.3333333333333333703, 0.3333333333333333703, 0.3333333333333333703, 0.3333333333333333703, 0.3333333333333333703, 0.3333333333333333703, 0.3333333333333333703, 0.3333333333333333703, 0.3333333333333333703, 0.3333333333333333703, 0.3333333333333333703, 0.3333333333333333703, 0.3333333333333333703, 0.3333333333333333703, 0.3333333333333333703, 0.3333333333333333703, 0.3333333333333333703, 0.3333333333333333703, 0.3333333333333333703, 0.3333333333333333703, 0.3333333333333333703, 0.3333333333333333703, 0.3333333333333333703, 0.3333333333333333703, 0.3333333333333333703, 0.3333333333333333703, 0.3333333333333333703, 0.3333333333333333703, 0.3333333333333333703, 0.3333333333333333703, 0.3333333333333333703, 0.3333333333333333703, 0.3333333333333333703, 0.3333333333333333703, 0.3333333333333333703, 0.3333333333333333703, 0.3333333333333333703, 0.3333333333333333703, 0.3333333333333333703, 0.3333333333333333703, 0.3333333333333333703, 0.3333333333333333703, 0.3333333333333333703, 0.3333333333333333703, 0.3333333333333333703, 0.3333333333333333703, 0.3333333333333333703, 0.3333333333333333703, 0.3333333333333333703, 0.3333333333333333703, 0.3333333333333333703, 0.3333333333333333703, 0.3333333333333333703, 0.3333333333333333703, 0.3333333333333333703, 0.3333333333333333703, 0.3333333333333333703, 0.3333333333333333703, 0.3333333333333333703, 0.3333333333333333703, 0.3333333333333333703, 0.3333333333333333703, 0.3333333333333333703),
 ( 0.3333333333333333703, 0.3333333333333333703, 0.3333333333333333703, 0.3333333333333333703, 0.3333333333333333703, 0.3333333333333333703, 0.3333333333333333703, 0.3333333333333333703, 0.3333333333333333703, 0.3333333333333333703, 0.3333333333333333703, 0.3333333333333333703, 0.3333333333333333703, 0.3333333333333333703, 0.3333333333333333703, 0.3333333333333333703, 0.3333333333333333703, 0.3333333333333333703, 0.3333333333333333703, 0.3333333333333333703, 0.3333333333333333703, 0.3333333333333333703, 0.3333333333333333703, 0.3333333333333333703, 0.3333333333333333703, 0.3333333333333333703, 0.3333333333333333703, 0.3333333333333333703, 0.3333333333333333703, 0.3333333333333333703, 0.3333333333333333703, 0.3333333333333333703, 0.3333333333333333703, 0.3333333333333333703, 0.3333333333333333703, 0.3333333333333333703, 0.3333333333333333703, 0.3333333333333333703, 0.3333333333333333703, 0.3333333333333333703, 0.3333333333333333703, 0.3333333333333333703, 0.3333333333333333703, 0.3333333333333333703, 0.3333333333333333703, 0.3333333333333333703, 0.3333333333333333703, 0.3333333333333333703, 0.3333333333333333703, 0.3333333333333333703, 0.3333333333333333703, 0.3333333333333333703, 0.3333333333333333703, 0.3333333333333333703, 0.3333333333333333703, 0.3333333333333333703, 0.3333333333333333703, 0.3333333333333333703, 0.3333333333333333703, 0.3333333333333333703, 0.3333333333333333703, 0.3333333333333333703, 0.3333333333333333703, 0.3333333333333333703, 0.3333333333333333703, 0.3333333333333333703, 0.3333333333333333703, 0.3333333333333333703, 0.3333333333333333703, 0.3333333333333333703, 0.3333333333333333703, 0.3333333333333333703, 0.3333333333333333703, 0.3333333333333333703, 0.3333333333333333703, 0.3333333333333333703, 0.3333333333333333703, 0.3333333333333333703, 0.3333333333333333703, 0.3333333333333333703, 0.3333333333333333703, 0.3333333333333333703, 0.3333333333333333703, 0.3333333333333333703, 0.3333333333333333703, 0.3333333333333333703, 0.3333333333333333703, 0.3333333333333333703, 0.3333333333333333703, 0.3333333333333333703, 0.3333333333333333703, 0.3333333333333333703, 0.3333333333333333703, 0.3333333333333333703, 0.3333333333333333703, 0.3333333333333333703, 0.3333333333333333703, 0.3333333333333333703, 0.3333333333333333703, 0.3333333333333333703, 0.3333333333333333703, 0.3333333333333333703, 0.3333333333333333703, 0.3333333333333333703, 0.3333333333333333703, 0.3333333333333333703, 0.3333333333333333703, 0.3333333333333333703, 0.3333333333333333703, 0.3333333333333333703, 0.3333333333333333703, 0.3333333333333333703, 0.3333333333333333703, 0.3333333333333333703, 0.3333333333333333703, 0.3333333333333333703, 0.3333333333333333703, 0.3333333333333333703, 0.3333333333333333703, 0.3333333333333333703, 0.3333333333333333703, 0.3333333333333333703, 0.3333333333333333703, 0.3333333333333333703, 0.3333333333333333703, 0.3333333333333333703, 0.3333333333333333703, 0.3333333333333333703, 0.3333333333333333703, 0.3333333333333333703, 0.3333333333333333703, 0.3333333333333333703, 0.3333333333333333703, 0.3333333333333333703, 0.3333333333333333703, 0.3333333333333333703, 0.3333333333333333703, 0.3333333333333333703, 0.3333333333333333703, 0.3333333333333333703, 0.3333333333333333703, 0.3333333333333333703, 0.3333333333333333703, 0.3333333333333333703, 0.3333333333333333703, 0.3333333333333333703, 0.3333333333333333703, 0.3333333333333333703, 0.3333333333333333703, 0.3333333333333333703, 0.3333333333333333703, 0.3333333333333333703, 0.3333333333333333703, 0.3333333333333333703, 0.3333333333333333703, 0.3333333333333333703, 0.3333333333333333703, 0.3333333333333333703, 0.3333333333333333703, 0.3333333333333333703, 0.3333333333333333703, 0.3333333333333333703, 0.3333333333333333703, 0.3333333333333333703, 0.3333333333333333703, 0.3333333333333333703, 0.3333333333333333703, 0.3333333333333333703, 0.3333333333333333703, 0.3333333333333333703, 0.3333333333333333703, 0.3333333333333333703, 0.3333333333333333703, 0.3333333333333333703, 0.3333333333333333703, 0.3333333333333333703, 0.3333333333333333703, 0.3333333333333333703, 0.3333333333333333703, 0.3333333333333333703, 0.3333333333333333703, 0.3333333333333333703, 0.3333333333333333703, 0.3333333333333333703, 0.3333333333333333703, 0.3333333333333333703),
 ( 1.000000000000000000, 1.000000000000000000, 1.000000000000000000, 1.000000000000000000, 1.000000000000000000, 1.000000000000000000, 1.000000000000000000, 1.000000000000000000, 1.000000000000000000, 1.000000000000000000, 1.000000000000000000, 1.000000000000000000, 1.000000000000000000, 1.000000000000000000, 1.000000000000000000, 1.000000000000000000, 1.000000000000000000, 1.000000000000000000, 1.000000000000000000, 1.000000000000000000, 1.000000000000000000, 1.000000000000000000, 1.000000000000000000, 1.000000000000000000, 1.000000000000000000, 1.000000000000000000, 1.000000000000000000, 1.000000000000000000, 1.000000000000000000, 1.000000000000000000, 1.000000000000000000, 1.000000000000000000, 1.000000000000000000, 1.000000000000000000, 1.000000000000000000, 1.000000000000000000, 1.000000000000000000, 1.000000000000000000, 1.000000000000000000, 1.000000000000000000, 1.000000000000000000, 1.000000000000000000, 1.000000000000000000, 1.000000000000000000, 1.000000000000000000, 1.000000000000000000, 1.000000000000000000, 1.000000000000000000, 1.000000000000000000, 1.000000000000000000, 1.000000000000000000, 1.000000000000000000, 1.000000000000000000, 1.000000000000000000, 1.000000000000000000, 1.000000000000000000, 1.000000000000000000, 1.000000000000000000, 1.000000000000000000, 1.000000000000000000, 1.000000000000000000, 1.000000000000000000, 1.000000000000000000, 1.000000000000000000, 1.000000000000000000, 1.000000000000000000, 1.000000000000000000, 1.000000000000000000, 1.000000000000000000, 1.000000000000000000, 1.000000000000000000, 1.000000000000000000, 1.000000000000000000, 1.000000000000000000, 1.000000000000000000, 1.000000000000000000, 1.000000000000000000, 1.000000000000000000, 1.000000000000000000, 1.000000000000000000, 1.000000000000000000, 1.000000000000000000, 1.000000000000000000, 1.000000000000000000, 1.000000000000000000, 1.000000000000000000, 1.000000000000000000, 1.000000000000000000, 1.000000000000000000, 1.000000000000000000, 1.000000000000000000, 1.000000000000000000, 1.000000000000000000, 1.000000000000000000, 1.000000000000000000, 1.000000000000000000, 1.000000000000000000, 1.000000000000000000, 1.000000000000000000, 1.000000000000000000, 1.000000000000000000, 1.000000000000000000, 1.000000000000000000, 1.000000000000000000, 1.000000000000000000, 1.000000000000000000, 1.000000000000000000, 1.000000000000000000, 1.000000000000000000, 1.000000000000000000, 1.000000000000000000, 1.000000000000000000, 1.000000000000000000, 1.000000000000000000, 1.000000000000000000, 1.000000000000000000, 1.000000000000000000, 1.000000000000000000, 1.000000000000000000, 1.000000000000000000, 1.000000000000000000, 1.000000000000000000, 1.000000000000000000, 1.000000000000000000, 1.000000000000000000, 1.000000000000000000, 1.000000000000000000, 1.000000000000000000, 1.000000000000000000, 1.000000000000000000, 1.000000000000000000, 1.000000000000000000, 1.000000000000000000, 1.000000000000000000, 1.000000000000000000, 1.000000000000000000, 1.000000000000000000, 1.000000000000000000, 1.000000000000000000, 1.000000000000000000, 1.000000000000000000, 1.000000000000000000, 1.000000000000000000, 1.000000000000000000, 1.000000000000000000, 1.000000000000000000, 1.000000000000000000, 1.000000000000000000, 1.000000000000000000, 1.000000000000000000, 1.000000000000000000, 1.000000000000000000, 1.000000000000000000, 1.000000000000000000, 1.000000000000000000, 1.000000000000000000, 1.000000000000000000, 1.000000000000000000, 1.000000000000000000, 1.000000000000000000, 1.000000000000000000, 1.000000000000000000, 1.000000000000000000, 1.000000000000000000, 1.000000000000000000, 1.000000000000000000, 1.000000000000000000, 1.000000000000000000, 1.000000000000000000, 1.000000000000000000, 1.000000000000000000, 1.000000000000000000, 1.000000000000000000, 1.000000000000000000, 1.000000000000000000, 1.000000000000000000, 1.000000000000000000, 1.000000000000000000, 1.000000000000000000, 1.000000000000000000, 1.000000000000000000, 1.000000000000000000, 1.000000000000000000, 1.000000000000000000, 1.000000000000000000, 1.000000000000000000),
 ( 0.3333333333333333703, 0.3333333333333333703, 0.3333333333333333703, 0.3333333333333333703, 0.3333333333333333703, 0.3333333333333333703, 0.3333333333333333703, 0.3333333333333333703, 0.3333333333333333703, 0.3333333333333333703, 0.3333333333333333703, 0.3333333333333333703, 0.3333333333333333703, 0.3333333333333333703, 0.3333333333333333703, 0.3333333333333333703, 0.3333333333333333703, 0.3333333333333333703, 0.3333333333333333703, 0.3333333333333333703, 0.3333333333333333703, 0.3333333333333333703, 0.3333333333333333703, 0.3333333333333333703, 0.3333333333333333703, 0.3333333333333333703, 0.3333333333333333703, 0.3333333333333333703, 0.3333333333333333703, 0.3333333333333333703, 0.3333333333333333703, 0.3333333333333333703, 0.3333333333333333703, 0.3333333333333333703, 0.3333333333333333703, 0.3333333333333333703, 0.3333333333333333703, 0.3333333333333333703, 0.3333333333333333703, 0.3333333333333333703, 0.3333333333333333703, 0.3333333333333333703, 0.3333333333333333703, 0.3333333333333333703, 0.3333333333333333703, 0.3333333333333333703, 0.3333333333333333703, 0.3333333333333333703, 0.3333333333333333703, 0.3333333333333333703, 0.3333333333333333703, 0.3333333333333333703, 0.3333333333333333703, 0.3333333333333333703, 0.3333333333333333703, 0.3333333333333333703, 0.3333333333333333703, 0.3333333333333333703, 0.3333333333333333703, 0.3333333333333333703, 0.3333333333333333703, 0.3333333333333333703, 0.3333333333333333703, 0.3333333333333333703, 0.3333333333333333703, 0.3333333333333333703, 0.3333333333333333703, 0.3333333333333333703, 0.3333333333333333703, 0.3333333333333333703, 0.3333333333333333703, 0.3333333333333333703, 0.3333333333333333703, 0.3333333333333333703, 0.3333333333333333703, 0.3333333333333333703, 0.3333333333333333703, 0.3333333333333333703, 0.3333333333333333703, 0.3333333333333333703, 0.3333333333333333703, 0.3333333333333333703, 0.3333333333333333703, 0.3333333333333333703, 0.3333333333333333703, 0.3333333333333333703, 0.3333333333333333703, 0.3333333333333333703, 0.3333333333333333703, 0.3333333333333333703, 0.3333333333333333703, 0.3333333333333333703, 0.3333333333333333703, 0.3333333333333333703, 0.3333333333333333703, 0.3333333333333333703, 0.3333333333333333703, 0.3333333333333333703, 0.3333333333333333703, 0.3333333333333333703, 0.3333333333333333703, 0.3333333333333333703, 0.3333333333333333703, 0.3333333333333333703, 0.3333333333333333703, 0.3333333333333333703, 0.3333333333333333703, 0.3333333333333333703, 0.3333333333333333703, 0.3333333333333333703, 0.3333333333333333703, 0.3333333333333333703, 0.3333333333333333703, 0.3333333333333333703, 0.3333333333333333703, 0.3333333333333333703, 0.3333333333333333703, 0.3333333333333333703, 0.3333333333333333703, 0.3333333333333333703, 0.3333333333333333703, 0.3333333333333333703, 0.3333333333333333703, 0.3333333333333333703, 0.3333333333333333703, 0.3333333333333333703, 0.3333333333333333703, 0.3333333333333333703, 0.3333333333333333703, 0.3333333333333333703, 0.3333333333333333703, 0.3333333333333333703, 0.3333333333333333703, 0.3333333333333333703, 0.3333333333333333703, 0.3333333333333333703, 0.3333333333333333703, 0.3333333333333333703, 0.3333333333333333703, 0.3333333333333333703, 0.3333333333333333703, 0.3333333333333333703, 0.3333333333333333703, 0.3333333333333333703, 0.3333333333333333703, 0.3333333333333333703, 0.3333333333333333703, 0.3333333333333333703, 0.3333333333333333703, 0.3333333333333333703, 0.3333333333333333703, 0.3333333333333333703, 0.3333333333333333703, 0.3333333333333333703, 0.3333333333333333703, 0.3333333333333333703, 0.3333333333333333703, 0.3333333333333333703, 0.3333333333333333703, 0.3333333333333333703, 0.3333333333333333703, 0.3333333333333333703, 0.3333333333333333703, 0.3333333333333333703, 0.3333333333333333703, 0.3333333333333333703, 0.3333333333333333703, 0.3333333333333333703, 0.3333333333333333703, 0.3333333333333333703, 0.3333333333333333703, 0.3333333333333333703, 0.3333333333333333703, 0.3333333333333333703, 0.3333333333333333703, 0.3333333333333333703, 0.3333333333333333703, 0.3333333333333333703, 0.3333333333333333703, 0.3333333333333333703, 0.3333333333333333703, 0.3333333333333333703, 0.3333333333333333703, 0.3333333333333333703, 0.3333333333333333703, 0.3333333333333333703),
 ( 0.3333333333333333703, 0.3333333333333333703, 0.3333333333333333703, 0.3333333333333333703, 0.3333333333333333703, 0.3333333333333333703, 0.3333333333333333703, 0.3333333333333333703, 0.3333333333333333703, 0.3333333333333333703, 0.3333333333333333703, 0.3333333333333333703, 0.3333333333333333703, 0.3333333333333333703, 0.3333333333333333703, 0.3333333333333333703, 0.3333333333333333703, 0.3333333333333333703, 0.3333333333333333703, 0.3333333333333333703, 0.3333333333333333703, 0.3333333333333333703, 0.3333333333333333703, 0.3333333333333333703, 0.3333333333333333703, 0.3333333333333333703, 0.3333333333333333703, 0.3333333333333333703, 0.3333333333333333703, 0.3333333333333333703, 0.3333333333333333703, 0.3333333333333333703, 0.3333333333333333703, 0.3333333333333333703, 0.3333333333333333703, 0.3333333333333333703, 0.3333333333333333703, 0.3333333333333333703, 0.3333333333333333703, 0.3333333333333333703, 0.3333333333333333703, 0.3333333333333333703, 0.3333333333333333703, 0.3333333333333333703, 0.3333333333333333703, 0.3333333333333333703, 0.3333333333333333703, 0.3333333333333333703, 0.3333333333333333703, 0.3333333333333333703, 0.3333333333333333703, 0.3333333333333333703, 0.3333333333333333703, 0.3333333333333333703, 0.3333333333333333703, 0.3333333333333333703, 0.3333333333333333703, 0.3333333333333333703, 0.3333333333333333703, 0.3333333333333333703, 0.3333333333333333703, 0.3333333333333333703, 0.3333333333333333703, 0.3333333333333333703, 0.3333333333333333703, 0.3333333333333333703, 0.3333333333333333703, 0.3333333333333333703, 0.3333333333333333703, 0.3333333333333333703, 0.3333333333333333703, 0.3333333333333333703, 0.3333333333333333703, 0.3333333333333333703, 0.3333333333333333703, 0.3333333333333333703, 0.3333333333333333703, 0.3333333333333333703, 0.3333333333333333703, 0.3333333333333333703, 0.3333333333333333703, 0.3333333333333333703, 0.3333333333333333703, 0.3333333333333333703, 0.3333333333333333703, 0.3333333333333333703, 0.3333333333333333703, 0.3333333333333333703, 0.3333333333333333703, 0.3333333333333333703, 0.3333333333333333703, 0.3333333333333333703, 0.3333333333333333703, 0.3333333333333333703, 0.3333333333333333703, 0.3333333333333333703, 0.3333333333333333703, 0.3333333333333333703, 0.3333333333333333703, 0.3333333333333333703, 0.3333333333333333703, 0.3333333333333333703, 0.3333333333333333703, 0.3333333333333333703, 0.3333333333333333703, 0.3333333333333333703, 0.3333333333333333703, 0.3333333333333333703, 0.3333333333333333703, 0.3333333333333333703, 0.3333333333333333703, 0.3333333333333333703, 0.3333333333333333703, 0.3333333333333333703, 0.3333333333333333703, 0.3333333333333333703, 0.3333333333333333703, 0.3333333333333333703, 0.3333333333333333703, 0.3333333333333333703, 0.3333333333333333703, 0.3333333333333333703, 0.3333333333333333703, 0.3333333333333333703, 0.3333333333333333703, 0.3333333333333333703, 0.3333333333333333703, 0.3333333333333333703, 0.3333333333333333703, 0.3333333333333333703, 0.3333333333333333703, 0.3333333333333333703, 0.3333333333333333703, 0.3333333333333333703, 0.3333333333333333703, 0.3333333333333333703, 0.3333333333333333703, 0.3333333333333333703, 0.3333333333333333703, 0.3333333333333333703, 0.3333333333333333703, 0.3333333333333333703, 0.3333333333333333703, 0.3333333333333333703, 0.3333333333333333703, 0.3333333333333333703, 0.3333333333333333703, 0.3333333333333333703, 0.3333333333333333703, 0.3333333333333333703, 0.3333333333333333703, 0.3333333333333333703, 0.3333333333333333703, 0.3333333333333333703, 0.3333333333333333703, 0.3333333333333333703, 0.3333333333333333703, 0.3333333333333333703, 0.3333333333333333703, 0.3333333333333333703, 0.3333333333333333703, 0.3333333333333333703, 0.3333333333333333703, 0.3333333333333333703, 0.3333333333333333703, 0.3333333333333333703, 0.3333333333333333703, 0.3333333333333333703, 0.3333333333333333703, 0.3333333333333333703, 0.3333333333333333703, 0.3333333333333333703, 0.3333333333333333703, 0.3333333333333333703, 0.3333333333333333703, 0.3333333333333333703, 0.3333333333333333703, 0.3333333333333333703, 0.3333333333333333703, 0.3333333333333333703, 0.3333333333333333703, 0.3333333333333333703, 0.3333333333333333703, 0.3333333333333333703, 0.3333333333333333703, 0.3333333333333333703),
 ( 1.000000000000000000, 1.000000000000000000, 1.000000000000000000, 1.000000000000000000, 1.000000000000000000, 1.000000000000000000, 1.000000000000000000, 1.000000000000000000, 1.000000000000000000, 1.000000000000000000, 1.000000000000000000, 1.000000000000000000, 1.000000000000000000, 1.000000000000000000, 1.000000000000000000, 1.000000000000000000, 1.000000000000000000, 1.000000000000000000, 1.000000000000000000, 1.000000000000000000, 1.000000000000000000, 1.000000000000000000, 1.000000000000000000, 1.000000000000000000, 1.000000000000000000, 1.000000000000000000, 1.000000000000000000, 1.000000000000000000, 1.000000000000000000, 1.000000000000000000, 1.000000000000000000, 1.000000000000000000, 1.000000000000000000, 1.000000000000000000, 1.000000000000000000, 1.000000000000000000, 1.000000000000000000, 1.000000000000000000, 1.000000000000000000, 1.000000000000000000, 1.000000000000000000, 1.000000000000000000, 1.000000000000000000, 1.000000000000000000, 1.000000000000000000, 1.000000000000000000, 1.000000000000000000, 1.000000000000000000, 1.000000000000000000, 1.000000000000000000, 1.000000000000000000, 1.000000000000000000, 1.000000000000000000, 1.000000000000000000, 1.000000000000000000, 1.000000000000000000, 1.000000000000000000, 1.000000000000000000, 1.000000000000000000, 1.000000000000000000, 1.000000000000000000, 1.000000000000000000, 1.000000000000000000, 1.000000000000000000, 1.000000000000000000, 1.000000000000000000, 1.000000000000000000, 1.000000000000000000, 1.000000000000000000, 1.000000000000000000, 1.000000000000000000, 1.000000000000000000, 1.000000000000000000, 1.000000000000000000, 1.000000000000000000, 1.000000000000000000, 1.000000000000000000, 1.000000000000000000, 1.000000000000000000, 1.000000000000000000, 1.000000000000000000, 1.000000000000000000, 1.000000000000000000, 1.000000000000000000, 1.000000000000000000, 1.000000000000000000, 1.000000000000000000, 1.000000000000000000, 1.000000000000000000, 1.000000000000000000, 1.000000000000000000, 1.000000000000000000, 1.000000000000000000, 1.000000000000000000, 1.000000000000000000, 1.000000000000000000, 1.000000000000000000, 1.000000000000000000, 1.000000000000000000, 1.000000000000000000, 1.000000000000000000, 1.000000000000000000, 1.000000000000000000, 1.000000000000000000, 1.000000000000000000, 1.000000000000000000, 1.000000000000000000, 1.000000000000000000, 1.000000000000000000, 1.000000000000000000, 1.000000000000000000, 1.000000000000000000, 1.000000000000000000, 1.000000000000000000, 1.000000000000000000, 1.000000000000000000, 1.000000000000000000, 1.000000000000000000, 1.000000000000000000, 1.000000000000000000, 1.000000000000000000, 1.000000000000000000, 1.000000000000000000, 1.000000000000000000, 1.000000000000000000, 1.000000000000000000, 1.000000000000000000, 1.000000000000000000, 1.000000000000000000, 1.000000000000000000, 1.000000000000000000, 1.000000000000000000, 1.000000000000000000, 1.000000000000000000, 1.000000000000000000, 1.000000000000000000, 1.000000000000000000, 1.000000000000000000, 1.000000000000000000, 1.000000000000000000, 1.000000000000000000, 1.000000000000000000, 1.000000000000000000, 1.000000000000000000, 1.000000000000000000, 1.000000000000000000, 1.000000000000000000, 1.000000000000000000, 1.000000000000000000, 1.000000000000000000, 1.000000000000000000, 1.000000000000000000, 1.000000000000000000, 1.000000000000000000, 1.000000000000000000, 1.000000000000000000, 1.000000000000000000, 1.000000000000000000, 1.000000000000000000, 1.000000000000000000, 1.000000000000000000, 1.000000000000000000, 1.000000000000000000, 1.000000000000000000, 1.000000000000000000, 1.000000000000000000, 1.000000000000000000, 1.000000000000000000, 1.000000000000000000, 1.000000000000000000, 1.000000000000000000, 1.000000000000000000, 1.000000000000000000, 1.000000000000000000, 1.000000000000000000, 1.000000000000000000, 1.000000000000000000, 1.000000000000000000, 1.000000000000000000, 1.000000000000000000, 1.000000000000000000, 1.000000000000000000, 1.000000000000000000, 1.000000000000000000, 1.000000000000000000, 1.000000000000000000) ) ) 
 REPRESENTATION_ITEM ( '' )  SURFACE ( )  );
#15574 = ORIENTED_EDGE ( 'NONE', *, *, #8015, .F. ) ;
#15575 = CARTESIAN_POINT ( 'NONE',  ( 12.77278825050581013, 8.691252192278360766, -14.91275796197543890 ) ) ;
#15576 = VECTOR ( 'NONE', #4316, 1000.000000000000000 ) ;
#15577 = CARTESIAN_POINT ( 'NONE',  ( 10.70135522441200671, 8.911701773272509897, -16.39640207298747754 ) ) ;
#15578 = DIRECTION ( 'NONE',  ( 0.9510565162951536422, 2.566386769018988816E-16, 0.3090169943749472292 ) ) ;
#15579 = DIRECTION ( 'NONE',  ( -0.9510565162951536422, -2.566386769018988323E-16, 0.3090169943749475623 ) ) ;
#15580 = ORIENTED_EDGE ( 'NONE', *, *, #11954, .T. ) ;
#15581 = AXIS2_PLACEMENT_3D ( 'NONE', #29455, #22677, #8473 ) ;
#15582 = DIRECTION ( 'NONE',  ( -0.9510565162951536422, -2.566386769018988323E-16, 0.3090169943749475623 ) ) ;
#15583 = VERTEX_POINT ( 'NONE', #18031 ) ;
#15584 = CARTESIAN_POINT ( 'NONE',  ( 10.35864918915110877, 16.97212501191939538, -17.92015940598198753 ) ) ;
#15585 = CARTESIAN_POINT ( 'NONE',  ( 33.19592593216645326, -10.35933293216661610, -17.69446280125821147 ) ) ;
#15586 = CARTESIAN_POINT ( 'NONE',  ( 24.92864811393110358, -0.2441600445015326137, -14.78813717129899885 ) ) ;
#15587 = ORIENTED_EDGE ( 'NONE', *, *, #3957, .F. ) ;
#15588 = EDGE_CURVE ( 'NONE', #17672, #20109, #20315, .T. ) ;
#15589 = EDGE_CURVE ( 'NONE', #15809, #7334, #27446, .T. ) ;
#15590 = CARTESIAN_POINT ( 'NONE',  ( -2.100000000000000977, -6.754115128641868940E-16, 1.700000000000000178 ) ) ;
#15591 = EDGE_CURVE ( 'NONE', #25090, #7345, #13305, .T. ) ;
#15592 = LINE ( 'NONE', #13156, #10182 ) ;
#15593 = EDGE_CURVE ( 'NONE', #20384, #12010, #23221, .T. ) ;
#15594 = CARTESIAN_POINT ( 'NONE',  ( 4.000000000000003553, 2.309401076758525573, -0.3572655899081716435 ) ) ;
#15595 = CARTESIAN_POINT ( 'NONE',  ( 24.16496757332932788, -10.42823604606268617, -16.34834267607407909 ) ) ;
#15596 = CARTESIAN_POINT ( 'NONE',  ( 24.71165717419137309, -6.805198111665588634, -19.34662478563667065 ) ) ;
#15597 =( GEOMETRIC_REPRESENTATION_CONTEXT ( 3 ) GLOBAL_UNCERTAINTY_ASSIGNED_CONTEXT ( ( #9175 ) ) GLOBAL_UNIT_ASSIGNED_CONTEXT ( ( #23222, #28145, #23678 ) ) REPRESENTATION_CONTEXT ( 'NONE', 'WORKASPACE' ) );
#15598 = ORIENTED_EDGE ( 'NONE', *, *, #3440, .T. ) ;
#15599 = CARTESIAN_POINT ( 'NONE',  ( 157.0152310637605240, -4.999999999999975131, -15.61832212156129707 ) ) ;
#15600 = VECTOR ( 'NONE', #18398, 1000.000000000000000 ) ;
#15601 = CARTESIAN_POINT ( 'NONE',  ( 149.7287565553230309, -1.999999999999975353, -33.82050807568879947 ) ) ;
#15602 = DIRECTION ( 'NONE',  ( 0.000000000000000000, 0.000000000000000000, -1.000000000000000000 ) ) ;
#15603 = DIRECTION ( 'NONE',  ( -0.9510565162951536422, 0.000000000000000000, -0.3090169943749472292 ) ) ;
#15604 = DIRECTION ( 'NONE',  ( -2.908569913943825554E-16, 1.000000000000000000, -0.000000000000000000 ) ) ;
#15605 = DIRECTION ( 'NONE',  ( -1.000000000000000000, 0.000000000000000000, -0.000000000000000000 ) ) ;
#15606 = UNCERTAINTY_MEASURE_WITH_UNIT (LENGTH_MEASURE( 1.000000000000000082E-05 ), #25786, 'distance_accuracy_value', 'NONE');
#15607 = CARTESIAN_POINT ( 'NONE',  ( 11.21589157578718421, 9.127945497600544300, -17.24491392235805876 ) ) ;
#15608 = CARTESIAN_POINT ( 'NONE',  ( 10.33811693838771717, 18.38618951776012267, -23.00000000000000711 ) ) ;
#15610 = AXIS2_PLACEMENT_3D ( 'NONE', #5156, #12312, #30252 ) ;
#15609 = DIRECTION ( 'NONE',  ( 0.000000000000000000, 0.000000000000000000, -1.000000000000000000 ) ) ;
#15611 = ORIENTED_EDGE ( 'NONE', *, *, #29040, .F. ) ;
#15612 = LINE ( 'NONE', #17746, #25659 ) ;
#15613 = FACE_BOUND ( 'NONE', #12773, .T. ) ;
#15614 = ORIENTED_EDGE ( 'NONE', *, *, #19722, .T. ) ;
#15615 = VECTOR ( 'NONE', #12688, 1000.000000000000000 ) ;
#15616 = CARTESIAN_POINT ( 'NONE',  ( 9.641384570184822422, 17.66873631484086715, -17.89388817125738385 ) ) ;
#15617 = PLANE ( 'NONE',  #24768 ) ;
#15618 = DIRECTION ( 'NONE',  ( 0.000000000000000000, 0.000000000000000000, 1.000000000000000000 ) ) ;
#15619 = PLANE ( 'NONE',  #10299 ) ;
#15621 = ORIENTED_EDGE ( 'NONE', *, *, #22743, .T. ) ;
#15620 = CARTESIAN_POINT ( 'NONE',  ( 21.94319337455657859, -4.318501116253552041, -18.82930321547734920 ) ) ;
#15622 = ORIENTED_EDGE ( 'NONE', *, *, #24836, .T. ) ;
#15623 = CARTESIAN_POINT ( 'NONE',  ( 131.1922820468854241, -4.999999999999982236, -2.083034168790677043 ) ) ;
#15624 = CARTESIAN_POINT ( 'NONE',  ( 12.24596961785936777, 9.516471373605908113, -15.33264171117454744 ) ) ;
#15625 = CARTESIAN_POINT ( 'NONE',  ( 33.09970432537804896, -11.76965169494800989, -17.65272085910585886 ) ) ;
#15626 = DIRECTION ( 'NONE',  ( -2.698458740408365879E-16, 1.000000000000000000, 0.000000000000000000 ) ) ;
#15627 = CARTESIAN_POINT ( 'NONE',  ( 23.63863231746517712, -2.790269051896475450, -19.68844555248840678 ) ) ;
#15628 = CARTESIAN_POINT ( 'NONE',  ( 0.000000000000000000, 0.000000000000000000, 0.000000000000000000 ) ) ;
#15629 = CARTESIAN_POINT ( 'NONE',  ( 21.15397186503396654, -1.756306506132798706, -15.01670888948634364 ) ) ;
#15630 = EDGE_LOOP ( 'NONE', ( #5998, #27849, #10359, #11189, #20023 ) ) ;
#15631 = ADVANCED_FACE ( 'NONE', ( #27400 ), #18330, .T. ) ;
#15632 = LINE ( 'NONE', #29589, #29133 ) ;
#15633 = ORIENTED_EDGE ( 'NONE', *, *, #13686, .T. ) ;
#15634 =( LENGTH_UNIT ( ) NAMED_UNIT ( * ) SI_UNIT ( .MILLI., .METRE. ) );
#15635 = CARTESIAN_POINT ( 'NONE',  ( 16.36264732604271899, 7.873549196589271659, -20.78255227469630739 ) ) ;
#15636 = CARTESIAN_POINT ( 'NONE',  ( 26.70980024742295456, -9.230482666323300833, -19.13350686062700134 ) ) ;
#15637 = VERTEX_POINT ( 'NONE', #1727 ) ;
#15638 = VECTOR ( 'NONE', #28390, 1000.000000000000000 ) ;
#15639 = CARTESIAN_POINT ( 'NONE',  ( 29.22485947447185595, -8.910266539455653501, -18.36689805200119707 ) ) ;
#15640 = VECTOR ( 'NONE', #1345, 1000.000000000000000 ) ;
#15641 = DIRECTION ( 'NONE',  ( -0.9510565162951536422, 0.000000000000000000, -0.3090169943749472292 ) ) ;
#15642 = ORIENTED_EDGE ( 'NONE', *, *, #2676, .F. ) ;
#15643 = MECHANICAL_DESIGN_GEOMETRIC_PRESENTATION_REPRESENTATION (  '', ( #14170 ), #20518 ) ;
#15644 = LINE ( 'NONE', #20366, #13145 ) ;
#15645 = DIRECTION ( 'NONE',  ( 0.3090169943749472292, 8.338696094057992503E-17, -0.9510565162951536422 ) ) ;
#15646 = CARTESIAN_POINT ( 'NONE',  ( 137.0152310637606092, -1.999999999999979572, -15.61832212156129351 ) ) ;
#15647 = CARTESIAN_POINT ( 'NONE',  ( 9.641350810849047548, 17.66889113945805789, -17.94384837343789485 ) ) ;
#15648 = CARTESIAN_POINT ( 'NONE',  ( 24.01829950071418907, -5.359185124211399476, -18.14381017295562160 ) ) ;
#15649 = CARTESIAN_POINT ( 'NONE',  ( 17.46151185945609186, 6.859213057953727599, -13.86392132274949418 ) ) ;
#15650 = EDGE_CURVE ( 'NONE', #3131, #24567, #25065, .T. ) ;
#15651 = CARTESIAN_POINT ( 'NONE',  ( 32.82219004228267778, -9.671386367997632405, -18.62901690529166743 ) ) ;
#15652 = B_SPLINE_CURVE_WITH_KNOTS ( 'NONE', 3,
 ( #26905, #17108, #26437, #13577 ),
 .UNSPECIFIED., .F., .F.,
 ( 4, 4 ),
 ( 2.380737581676867028E-07, 0.002336974151641585049 ),
 .UNSPECIFIED. ) ;
#15653 = CARTESIAN_POINT ( 'NONE',  ( 2.500000000000000444, 2.357898499370430834, -3.469446951953614189E-15 ) ) ;
#15654 = CARTESIAN_POINT ( 'NONE',  ( 11.47652547240386944, 9.253065934422213701, -15.85936358228339316 ) ) ;
#15655 = DIRECTION ( 'NONE',  ( 1.000000000000000000, 4.440892098500622217E-16, 0.000000000000000000 ) ) ;
#15656 = LINE ( 'NONE', #18092, #16843 ) ;
#15657 = CARTESIAN_POINT ( 'NONE',  ( 9.661883061612440926, 16.25482663361732705, -17.92981046679734547 ) ) ;
#15658 = DIRECTION ( 'NONE',  ( -2.698458740408365879E-16, 1.000000000000000000, 0.000000000000000000 ) ) ;
#15659 = DIRECTION ( 'NONE',  ( 0.9510565162951536422, 0.000000000000000000, -0.3090169943749475623 ) ) ;
#15660 = CARTESIAN_POINT ( 'NONE',  ( 10.33811693838771717, 18.38618951776012267, -17.95086732675816776 ) ) ;
#15661 = EDGE_LOOP ( 'NONE', ( #29534, #28945, #20142 ) ) ;
#15662 = VECTOR ( 'NONE', #7234, 999.9999999999998863 ) ;
#15663 = DIRECTION ( 'NONE',  ( 1.000000000000000000, 2.168404344971006896E-16, 0.000000000000000000 ) ) ;
#15664 = FACE_OUTER_BOUND ( 'NONE', #25279, .T. ) ;
#15665 = DIRECTION ( 'NONE',  ( -0.5877852522924731371, 0.000000000000000000, 0.8090169943749474513 ) ) ;
#15666 = EDGE_LOOP ( 'NONE', ( #9027, #11190, #9564, #29438 ) ) ;
#15667 = CARTESIAN_POINT ( 'NONE',  ( 13.37841584274036855, 7.625425322794393779, -15.70882597216490240 ) ) ;
#15668 = CARTESIAN_POINT ( 'NONE',  ( 31.92618181579182135, -10.29178896789921893, -18.33933693937521880 ) ) ;
#15669 = CARTESIAN_POINT ( 'NONE',  ( 18.04051923446642292, -0.4597542321540471488, -16.60176153622942508 ) ) ;
#15670 = CARTESIAN_POINT ( 'NONE',  ( 26.95082352492110189, -12.40836276091286194, -17.97502949936508898 ) ) ;
#15671 = DIRECTION ( 'NONE',  ( 0.000000000000000000, -0.5000000000000011102, -0.8660254037844379305 ) ) ;
#15672 = CYLINDRICAL_SURFACE ( 'NONE', #9855, 2.500000000000002665 ) ;
#15673 = CARTESIAN_POINT ( 'NONE',  ( 19.28943675834911531, -1.002762487816046155, -14.40755329178536037 ) ) ;
#15674 = EDGE_LOOP ( 'NONE', ( #26648, #13953, #25963, #5056 ) ) ;
#15675 = FACE_OUTER_BOUND ( 'NONE', #18558, .T. ) ;
#15676 = ORIENTED_EDGE ( 'NONE', *, *, #17176, .T. ) ;
#15678 = VERTEX_POINT ( 'NONE', #24925 ) ;
#15677 = DIRECTION ( 'NONE',  ( 0.5877852522924731371, 1.586114251531760728E-16, 0.8090169943749474513 ) ) ;
#15679 = FACE_OUTER_BOUND ( 'NONE', #5240, .T. ) ;
#15680 = PLANE ( 'NONE',  #7013 ) ;
#15681 = ADVANCED_BREP_SHAPE_REPRESENTATION ( '', ( #1479, #13190 ), #21465 ) ;
#15682 = CARTESIAN_POINT ( 'NONE',  ( 149.5152310637605808, -4.999999999999976907, -1.659952520591374334E-14 ) ) ;
#15683 = EDGE_CURVE ( 'NONE', #19711, #8784, #27541, .T. ) ;
#15684 = EDGE_CURVE ( 'NONE', #2471, #24619, #15697, .T. ) ;
#15685 = CARTESIAN_POINT ( 'NONE',  ( 35.50545599541538877, -20.99072003637593653, -18.92103158260024642 ) ) ;
#15686 = VERTEX_POINT ( 'NONE', #29859 ) ;
#15687 = CARTESIAN_POINT ( 'NONE',  ( 10.64844024921564092, 9.137493944846720950, -16.41957189434499753 ) ) ;
#15689 = EDGE_CURVE ( 'NONE', #21114, #24657, #8871, .T. ) ;
#15688 = PRODUCT ( 'socket head cap screw_iso_ISO 4762 M5 x 20 - 20N', 'socket head cap screw_iso_ISO 4762 M5 x 20 - 20N', '', ( #8083 ) ) ;
#15690 = CARTESIAN_POINT ( 'NONE',  ( 29.62588713853392264, -10.65184931322849060, -12.76488833982454629 ) ) ;
#15691 = PLANE ( 'NONE',  #11364 ) ;
#15692 = CARTESIAN_POINT ( 'NONE',  ( 10.35864924400752862, 16.97212476034085782, -17.91519562840587199 ) ) ;
#15693 = CYLINDRICAL_SURFACE ( 'NONE', #20435, 3.000000000000002665 ) ;
#15694 = ORIENTED_EDGE ( 'NONE', *, *, #21900, .F. ) ;
#15695 = DIRECTION ( 'NONE',  ( 0.5877852522924731371, 1.586114251531760728E-16, 0.8090169943749474513 ) ) ;
#15696 = CARTESIAN_POINT ( 'NONE',  ( 16.84948243412402036, 10.49281628697410262, -11.66356073909478575 ) ) ;
#15698 = PLANE ( 'NONE',  #29175 ) ;
#15697 = CIRCLE ( 'NONE', #22047, 13.00000000000000178 ) ;
#15699 = VERTEX_POINT ( 'NONE', #15885 ) ;
#15700 = LINE ( 'NONE', #29962, #7164 ) ;
#15701 = VERTEX_POINT ( 'NONE', #18489 ) ;
#15702 = CARTESIAN_POINT ( 'NONE',  ( 9.661883061612440926, 16.25482663361732705, -17.91928203681695564 ) ) ;
#15703 = CARTESIAN_POINT ( 'NONE',  ( 18.26079443319284934, -0.1287745640203900310, -14.06839115638798354 ) ) ;
#15704 = CARTESIAN_POINT ( 'NONE',  ( 19.20998527735078198, 1.665648160765265784, -20.80323043525838855 ) ) ;
#15705 = ORIENTED_EDGE ( 'NONE', *, *, #27930, .T. ) ;
#15706 = DIRECTION ( 'NONE',  ( -0.9510565162951536422, -2.566386769018988816E-16, -0.3090169943749472292 ) ) ;
#15707 = CARTESIAN_POINT ( 'NONE',  ( 132.2287565553230024, -10.00000000000000888, -29.49038105676660138 ) ) ;
#15708 = CARTESIAN_POINT ( 'NONE',  ( 20.72626264887238534, -1.914771856900582714, -13.62749948506543518 ) ) ;
#15709 = VECTOR ( 'NONE', #4865, 999.9999999999998863 ) ;
#15710 = CARTESIAN_POINT ( 'NONE',  ( 176.1922820468852535, -9.999999999999994671, -2.083034168790677043 ) ) ;
#15711 = LINE ( 'NONE', #25041, #6945 ) ;
#15712 = VECTOR ( 'NONE', #29786, 1000.000000000000000 ) ;
#15713 = ORIENTED_EDGE ( 'NONE', *, *, #5510, .F. ) ;
#15714 = CARTESIAN_POINT ( 'NONE',  ( 10.46817501828509123, 16.46982559821503145, -17.33665662920367723 ) ) ;
#15715 = EDGE_CURVE ( 'NONE', #12381, #17616, #13750, .T. ) ;
#15716 = CARTESIAN_POINT ( 'NONE',  ( 154.5152310637604955, -4.999999999999976019, -13.05155085951651195 ) ) ;
#15717 = DIRECTION ( 'NONE',  ( 1.000000000000000000, 2.891205793294675861E-16, 0.000000000000000000 ) ) ;
#15718 = ORIENTED_EDGE ( 'NONE', *, *, #26, .T. ) ;
#15719 = EDGE_CURVE ( 'NONE', #22060, #11457, #11453, .T. ) ;
#15720 = ORIENTED_EDGE ( 'NONE', *, *, #21269, .T. ) ;
#15721 = CARTESIAN_POINT ( 'NONE',  ( 143.6922820468854241, -1.999999999999978018, -6.413161187712876909 ) ) ;
#15722 = EDGE_CURVE ( 'NONE', #13765, #13649, #30152, .T. ) ;
#15723 = CARTESIAN_POINT ( 'NONE',  ( 19.05868480923028940, 8.129737193291200370, -16.02886444249750042 ) ) ;
#15724 = CARTESIAN_POINT ( 'NONE',  ( 12.24513942169458858, 9.516104476910269838, -15.33330339355663519 ) ) ;
#15725 = CARTESIAN_POINT ( 'NONE',  ( 35.54287943964028784, -22.15884374752674546, -18.65915260879160797 ) ) ;
#15726 = ORIENTED_EDGE ( 'NONE', *, *, #14952, .T. ) ;
#15727 = DIRECTION ( 'NONE',  ( 0.000000000000000000, 0.000000000000000000, 1.000000000000000000 ) ) ;
#15728 = CARTESIAN_POINT ( 'NONE',  ( 12.75280283744833376, 7.624395256242640251, -14.92868632776139037 ) ) ;
#15729 = FACE_BOUND ( 'NONE', #29331, .T. ) ;
#15730 = CARTESIAN_POINT ( 'NONE',  ( 167.0152310637604671, -4.999999999999972466, -1.854241549900775467E-14 ) ) ;
#15731 = VERTEX_POINT ( 'NONE', #25514 ) ;
#15732 = CARTESIAN_POINT ( 'NONE',  ( 126.7486941615241989, -4.999999999999984013, -92.08831667749211647 ) ) ;
#15733 = ORIENTED_EDGE ( 'NONE', *, *, #12140, .T. ) ;
#15734 = CARTESIAN_POINT ( 'NONE',  ( 12.90243451339205194, 9.531139938431367753, -16.08819151157827321 ) ) ;
#15735 = CARTESIAN_POINT ( 'NONE',  ( 33.07549275714919901, -10.34104163876563831, -17.35407900654646340 ) ) ;
#15736 = CARTESIAN_POINT ( 'NONE',  ( 19.83745040964868522, -2.306422872736943575, -14.39351019504378293 ) ) ;
#15737 = EDGE_LOOP ( 'NONE', ( #2217, #1312, #9541, #8001 ) ) ;
#15738 = CARTESIAN_POINT ( 'NONE',  ( 2.500000000000000444, 2.357898499370430834, -3.469446951953614189E-15 ) ) ;
#15739 = AXIS2_PLACEMENT_3D ( 'NONE', #29161, #29639, #6078 ) ;
#15740 = CARTESIAN_POINT ( 'NONE',  ( 20.00000000000017053, 34.64101615137744972, 14.00000000000000178 ) ) ;
#15741 = PRESENTATION_STYLE_ASSIGNMENT (( #15283 ) ) ;
#15742 = CARTESIAN_POINT ( 'NONE',  ( 30.78125299044525320, -8.317598597646391312, -16.28273480984023891 ) ) ;
#15743 = CARTESIAN_POINT ( 'NONE',  ( 24.28190956353967422, -4.127413435877471670, -12.52835809790152766 ) ) ;
#15744 = ORIENTED_EDGE ( 'NONE', *, *, #11879, .F. ) ;
#15745 = CARTESIAN_POINT ( 'NONE',  ( 146.1922820468854241, -1.999999999999977573, -13.59645775552055902 ) ) ;
#15746 = LINE ( 'NONE', #15897, #13497 ) ;
#15747 = PLANE ( 'NONE',  #8233 ) ;
#15748 = EDGE_CURVE ( 'NONE', #5490, #29035, #16544, .T. ) ;
#15749 = DIRECTION ( 'NONE',  ( 0.9510565162951536422, 2.566386769018988816E-16, 0.3090169943749472292 ) ) ;
#15750 = AXIS2_PLACEMENT_3D ( 'NONE', #14838, #828, #9822 ) ;
#15751 = CARTESIAN_POINT ( 'NONE',  ( 11.09431937732777129, 9.685491096586417825, -17.29518830297554643 ) ) ;
#15752 = ADVANCED_FACE ( 'NONE', ( #16496 ), #9773, .T. ) ;
#15753 = EDGE_CURVE ( 'NONE', #23552, #9765, #28444, .T. ) ;
#15754 = CARTESIAN_POINT ( 'NONE',  ( 12.50035968906703765, 8.570861208087439564, -15.12988832871674560 ) ) ;
#15755 = EDGE_CURVE ( 'NONE', #11857, #29468, #11907, .T. ) ;
#15756 = CARTESIAN_POINT ( 'NONE',  ( 27.62103240953636174, -12.62788667074165794, -13.46147607715242245 ) ) ;
#15757 = ORIENTED_EDGE ( 'NONE', *, *, #29864, .T. ) ;
#15758 = CYLINDRICAL_SURFACE ( 'NONE', #6668, 8.000000000000007105 ) ;
#15759 = ORIENTED_EDGE ( 'NONE', *, *, #681, .T. ) ;
#15760 = DIRECTION ( 'NONE',  ( -1.000000000000000000, 0.000000000000000000, 0.000000000000000000 ) ) ;
#15761 = PLANE ( 'NONE',  #15486 ) ;
#15762 = CARTESIAN_POINT ( 'NONE',  ( 18.98827506421364575, 7.203492520304279445, -17.17051369180543929 ) ) ;
#15763 = CARTESIAN_POINT ( 'NONE',  ( 130.4440631633587202, -4.999999999999982236, -94.77315941399760391 ) ) ;
#15764 = CARTESIAN_POINT ( 'NONE',  ( 149.5152310637605808, -4.999999999999976907, -30.37205893520531319 ) ) ;
#15766 = VERTEX_POINT ( 'NONE', #4752 ) ;
#15765 = CARTESIAN_POINT ( 'NONE',  ( 23.11440248821028831, -7.346120041196752659, -16.32852059634029018 ) ) ;
#15767 = EDGE_LOOP ( 'NONE', ( #755, #8072, #30034, #25994 ) ) ;
#15768 = CARTESIAN_POINT ( 'NONE',  ( 146.1922820468854525, -1.999999999999977129, -30.91696583120935671 ) ) ;
#15769 = CARTESIAN_POINT ( 'NONE',  ( 12.24552273913795730, 9.516269270964150095, -15.33299823368393078 ) ) ;
#15770 = CARTESIAN_POINT ( 'NONE',  ( 34.82539348385352440, -18.93555941106099993, -20.13934242161363741 ) ) ;
#15771 = DIRECTION ( 'NONE',  ( 0.5877852522924731371, 1.586114251531760728E-16, -0.8090169943749474513 ) ) ;
#15772 = CARTESIAN_POINT ( 'NONE',  ( 25.97256211245905533, -8.171536508395311316, -18.54953510021574559 ) ) ;
#15773 = CARTESIAN_POINT ( 'NONE',  ( 8.000000000000001776, 4.336808689942017736E-15, -5.000000000000000888 ) ) ;
#15774 = CARTESIAN_POINT ( 'NONE',  ( 25.36902537161520499, -2.228419832982303728, -15.31576610616191481 ) ) ;
#15775 = ORIENTED_EDGE ( 'NONE', *, *, #12511, .F. ) ;
#15776 = CARTESIAN_POINT ( 'NONE',  ( 10.35864918915111055, 16.97212501191939182, -23.00000000000000711 ) ) ;
#15777 = SHAPE_REPRESENTATION_RELATIONSHIP ( 'NONE' , 'NONE' ,  #22819, #15681 ) ;
#15778 = CARTESIAN_POINT ( 'NONE',  ( 29.60951380729897764, -9.700310021160106544, -19.83312561509874783 ) ) ;
#15779 = CARTESIAN_POINT ( 'NONE',  ( 29.51995068812739476, -6.211492405346085377, -16.93985997890334261 ) ) ;
#15780 = AXIS2_PLACEMENT_3D ( 'NONE', #5783, #19506, #5480 ) ;
#15781 = VERTEX_POINT ( 'NONE', #28144 ) ;
#15782 = ORIENTED_EDGE ( 'NONE', *, *, #7320, .T. ) ;
#15783 = CARTESIAN_POINT ( 'NONE',  ( 134.5152310637605524, -4.999999999999981348, -1.493419066897600538E-14 ) ) ;
#15784 = CARTESIAN_POINT ( 'NONE',  ( 134.5152310637605524, -4.999999999999981348, -21.71180489736090991 ) ) ;
#15785 = DIRECTION ( 'NONE',  ( 0.000000000000000000, 0.000000000000000000, -1.000000000000000000 ) ) ;
#15786 = DIRECTION ( 'NONE',  ( -0.9510565162951536422, -2.566386769018988816E-16, -0.3090169943749472292 ) ) ;
#15787 = EDGE_CURVE ( 'NONE', #22258, #117, #5362, .T. ) ;
#15788 = PLANE ( 'NONE',  #10440 ) ;
#15789 = EDGE_CURVE ( 'NONE', #16318, #18472, #7495, .T. ) ;
#15790 = DIRECTION ( 'NONE',  ( -1.000000000000000000, 0.000000000000000000, -0.000000000000000000 ) ) ;
#15791 = EDGE_CURVE ( 'NONE', #9240, #3706, #2933, .T. ) ;
#15792 = CARTESIAN_POINT ( 'NONE',  ( 24.01770293978927384, -9.123702295727731837, -14.45939194930751448 ) ) ;
#15793 = CARTESIAN_POINT ( 'NONE',  ( 20.51209521231993094, 3.083376493849706801, -19.38174501956431683 ) ) ;
#15794 = CARTESIAN_POINT ( 'NONE',  ( 33.89278150306358128, -11.43586942258664507, -20.72336631513872973 ) ) ;
#15795 = DIRECTION ( 'NONE',  ( -1.000000000000000000, 0.000000000000000000, -0.000000000000000000 ) ) ;
#15796 = CARTESIAN_POINT ( 'NONE',  ( 12.50035968906703765, 8.570861208087439564, -15.12988832871674560 ) ) ;
#15797 = VECTOR ( 'NONE', #9399, 1000.000000000000000 ) ;
#15798 = CARTESIAN_POINT ( 'NONE',  ( 8.500000000000088818, 17.32050807568872486, -17.99999999999999645 ) ) ;
#15799 = DIRECTION ( 'NONE',  ( -2.698458740408365879E-16, 1.000000000000000000, 0.000000000000000000 ) ) ;
#15800 = CARTESIAN_POINT ( 'NONE',  ( 9.797549260427590667, 15.63264415243319938, -17.83144836289601898 ) ) ;
#15801 = CARTESIAN_POINT ( 'NONE',  ( 162.2287565553229456, -9.999999999999998224, -20.83012701892220520 ) ) ;
#15802 = ORIENTED_EDGE ( 'NONE', *, *, #15166, .T. ) ;
#15803 = CARTESIAN_POINT ( 'NONE',  ( 420.0000000000002274, 43.64101615137744972, 12.00000000000000178 ) ) ;
#15804 = CARTESIAN_POINT ( 'NONE',  ( 12.29195110325218288, 8.516770644378290456, -15.29309475950548958 ) ) ;
#15805 = EDGE_LOOP ( 'NONE', ( #110, #25194, #459, #11392, #7343 ) ) ;
#15806 = DIRECTION ( 'NONE',  ( -0.9510565162951536422, 0.000000000000000000, -0.3090169943749472292 ) ) ;
#15807 = CARTESIAN_POINT ( 'NONE',  ( 139.5152310637606092, -1.999999999999978684, -28.60870317832789311 ) ) ;
#15808 = DIRECTION ( 'NONE',  ( -0.8090169943749474513, -2.183098979609982436E-16, -0.5877852522924731371 ) ) ;
#15809 = VERTEX_POINT ( 'NONE', #23996 ) ;
#15810 = VECTOR ( 'NONE', #4765, 1000.000000000000000 ) ;
#15811 = ORIENTED_EDGE ( 'NONE', *, *, #12035, .F. ) ;
#15812 = CARTESIAN_POINT ( 'NONE',  ( 13.59703899429919005, 7.722038565090276308, -15.53457947969411634 ) ) ;
#15813 = CARTESIAN_POINT ( 'NONE',  ( 35.41344336761681433, -22.57735604011907071, -20.16400759377322061 ) ) ;
#15814 = CARTESIAN_POINT ( 'NONE',  ( 18.41232452102509143, -0.3525767977158695277, -15.58598945151665305 ) ) ;
#15815 = CARTESIAN_POINT ( 'NONE',  ( 17.64917075666736679, 6.165203978315560995, -14.56523922633501655 ) ) ;
#15816 = LINE ( 'NONE', #6383, #16202 ) ;
#15817 = CARTESIAN_POINT ( 'NONE',  ( 21.04533358917985808, -3.575919577149618167, -19.74844908412899969 ) ) ;
#15818 = EDGE_CURVE ( 'NONE', #8937, #3493, #937, .T. ) ;
#15819 = AXIS2_PLACEMENT_3D ( 'NONE', #12865, #8728, #1140 ) ;
#15820 = ORIENTED_EDGE ( 'NONE', *, *, #20289, .T. ) ;
#15821 = DIRECTION ( 'NONE',  ( 1.000000000000000000, 4.440892098500622217E-16, 0.000000000000000000 ) ) ;
#15823 = ORIENTED_EDGE ( 'NONE', *, *, #7117, .T. ) ;
#15822 = CARTESIAN_POINT ( 'NONE',  ( 113.6585242177747972, -4.999999999999986677, -82.57775151454063689 ) ) ;
#15824 = LINE ( 'NONE', #1821, #26863 ) ;
#15825 = DIRECTION ( 'NONE',  ( 1.000000000000000000, 0.000000000000000000, 0.000000000000000000 ) ) ;
#15826 = CARTESIAN_POINT ( 'NONE',  ( 20.00000000000017053, 41.64101615137744972, 14.00000000000000178 ) ) ;
#15827 = CARTESIAN_POINT ( 'NONE',  ( 35.15837367389831769, -19.43146302041509443, -19.19767279675701488 ) ) ;
#15828 = ORIENTED_EDGE ( 'NONE', *, *, #15854, .T. ) ;
#15829 = CARTESIAN_POINT ( 'NONE',  ( 10.66059746906157635, 9.081739384948186000, -16.41454445628326297 ) ) ;
#15830 = VERTEX_POINT ( 'NONE', #19833 ) ;
#15831 = LINE ( 'NONE', #25162, #6873 ) ;
#15832 = LINE ( 'NONE', #3180, #7976 ) ;
#15833 = CARTESIAN_POINT ( 'NONE',  ( 11.76876341733043141, 10.50516141373230106, -16.79855566342228101 ) ) ;
#15834 = PLANE ( 'NONE',  #16568 ) ;
#15835 = ORIENTED_EDGE ( 'NONE', *, *, #6915, .F. ) ;
#15836 = LINE ( 'NONE', #25319, #13436 ) ;
#15837 = AXIS2_PLACEMENT_3D ( 'NONE', #12192, #23350, #5181 ) ;
#15838 = LINE ( 'NONE', #29814, #1986 ) ;
#15840 = EDGE_LOOP ( 'NONE', ( #11273, #6033, #26893, #1537 ) ) ;
#15839 = DIRECTION ( 'NONE',  ( -0.8090169943749474513, -2.183098979609982436E-16, -0.5877852522924731371 ) ) ;
#15841 = ORIENTED_EDGE ( 'NONE', *, *, #22911, .F. ) ;
#15842 = ORIENTED_EDGE ( 'NONE', *, *, #25287, .T. ) ;
#15843 = CARTESIAN_POINT ( 'NONE',  ( 157.0152310637605524, -4.999999999999975131, -34.70218595412750773 ) ) ;
#15844 = ORIENTED_EDGE ( 'NONE', *, *, #2983, .F. ) ;
#15845 = CARTESIAN_POINT ( 'NONE',  ( 13.12723341905928898, 8.572452836447732594, -15.90902281579132449 ) ) ;
#15846 = EDGE_LOOP ( 'NONE', ( #13033, #26463, #1214, #13901, #6286 ) ) ;
#15847 = CARTESIAN_POINT ( 'NONE',  ( 24.59799960276797393, -1.134526835705675918, -15.12159415400816975 ) ) ;
#15848 = CARTESIAN_POINT ( 'NONE',  ( 22.87580194831562252, -0.07614860672512525908, -19.74465839296685132 ) ) ;
#15849 = CARTESIAN_POINT ( 'NONE',  ( 21.92441584138004984, 2.204866226087792924, -14.79409581392398110 ) ) ;
#15850 = CARTESIAN_POINT ( 'NONE',  ( 173.6922820468853672, -9.999999999999994671, -32.39392330124607611 ) ) ;
#15851 = DIRECTION ( 'NONE',  ( 0.9510565162951535312, 2.566386769018988816E-16, -0.3090169943749475623 ) ) ;
#15852 = CIRCLE ( 'NONE', #2709, 4.000000000000004441 ) ;
#15853 = EDGE_CURVE ( 'NONE', #22258, #13830, #26901, .T. ) ;
#15854 = EDGE_CURVE ( 'NONE', #16825, #6890, #5962, .T. ) ;
#15855 = CARTESIAN_POINT ( 'NONE',  ( 21.42923412144385509, -1.598955984811285536, -13.33006947543598741 ) ) ;
#15856 = DIRECTION ( 'NONE',  ( -0.5877852522924731371, -1.586114251531760235E-16, 0.8090169943749474513 ) ) ;
#15857 = DIRECTION ( 'NONE',  ( 0.000000000000000000, -0.4999999999999993894, 0.8660254037844389297 ) ) ;
#15858 = VECTOR ( 'NONE', #14807, 1000.000000000000000 ) ;
#15859 = PRESENTATION_LAYER_ASSIGNMENT (  '', '', ( #17819 ) ) ;
#15860 = ORIENTED_EDGE ( 'NONE', *, *, #21558, .T. ) ;
#15861 = CARTESIAN_POINT ( 'NONE',  ( 146.1922820468854525, -10.00000000000000178, -19.40354224447947828 ) ) ;
#15862 = CARTESIAN_POINT ( 'NONE',  ( 35.54859390953724585, -22.18451583373416014, -17.22552805718784441 ) ) ;
#15863 = CARTESIAN_POINT ( 'NONE',  ( 0.000000000000000000, 0.000000000000000000, -18.00000000000000000 ) ) ;
#15864 = ORIENTED_EDGE ( 'NONE', *, *, #5895, .F. ) ;
#15865 = ORIENTED_EDGE ( 'NONE', *, *, #18168, .T. ) ;
#15866 = CARTESIAN_POINT ( 'NONE',  ( 133.7287565553229172, -9.999999999999980460, -33.50000000000000000 ) ) ;
#15867 = CARTESIAN_POINT ( 'NONE',  ( 19.25048709941964376, 7.441878894999256921, -18.84525011105569803 ) ) ;
#15868 = CARTESIAN_POINT ( 'NONE',  ( 12.24619727527933222, 9.516571979449480523, -15.33246026419563890 ) ) ;
#15869 = CARTESIAN_POINT ( 'NONE',  ( 35.53434814243864537, -22.12051714835155281, -18.84852710552948096 ) ) ;
#15870 = ORIENTED_EDGE ( 'NONE', *, *, #23847, .F. ) ;
#15871 = PLANE ( 'NONE',  #13719 ) ;
#15872 = AXIS2_PLACEMENT_3D ( 'NONE', #5458, #26530, #16895 ) ;
#15873 = CARTESIAN_POINT ( 'NONE',  ( 9.641350810849047548, 17.66889113945805789, -17.91796598306941135 ) ) ;
#15874 = CARTESIAN_POINT ( 'NONE',  ( 153.6922820468854241, -4.999999999999976019, -23.73366926340167637 ) ) ;
#15875 = CARTESIAN_POINT ( 'NONE',  ( 154.5152310637605524, -4.999999999999976019, -30.37205893520531319 ) ) ;
#15876 = ORIENTED_EDGE ( 'NONE', *, *, #26528, .F. ) ;
#15877 = DIRECTION ( 'NONE',  ( 0.000000000000000000, 0.000000000000000000, 1.000000000000000000 ) ) ;
#15878 = VERTEX_POINT ( 'NONE', #3670 ) ;
#15879 = CARTESIAN_POINT ( 'NONE',  ( 12.86837137031974621, 9.516086858917468305, -16.11534043535873906 ) ) ;
#15881 = CARTESIAN_POINT ( 'NONE',  ( 33.16581763841239194, -10.35476010881584052, -17.60936685258081624 ) ) ;
#15880 = VECTOR ( 'NONE', #26526, 1000.000000000000000 ) ;
#15882 = CARTESIAN_POINT ( 'NONE',  ( 24.78692427941192733, -9.284778175067517125, -17.23615439686343720 ) ) ;
#15883 = VECTOR ( 'NONE', #26583, 1000.000000000000114 ) ;
#15884 = DIRECTION ( 'NONE',  ( 0.000000000000000000, 0.000000000000000000, 1.000000000000000000 ) ) ;
#15885 = CARTESIAN_POINT ( 'NONE',  ( 134.5152310637605808, -1.999999999999980460, -28.60870317832789311 ) ) ;
#15886 = ORIENTED_EDGE ( 'NONE', *, *, #5714, .F. ) ;
#15887 =( NAMED_UNIT ( * ) PLANE_ANGLE_UNIT ( ) SI_UNIT ( $, .RADIAN. ) );
#15888 = EDGE_CURVE ( 'NONE', #12515, #16524, #20573, .T. ) ;
#15889 = ADVANCED_FACE ( 'NONE', ( #1391 ), #24278, .T. ) ;
#15890 = CARTESIAN_POINT ( 'NONE',  ( 30.02037170576755187, -9.505783518442527225, -18.49971606337314967 ) ) ;
#15891 = EDGE_CURVE ( 'NONE', #27920, #25350, #15402, .T. ) ;
#15892 = CARTESIAN_POINT ( 'NONE',  ( 27.68339325353806046, -3.782361434017075474, -17.87574284786517964 ) ) ;
#15893 = EDGE_CURVE ( 'NONE', #20965, #22051, #17100, .T. ) ;
#15894 = ORIENTED_EDGE ( 'NONE', *, *, #4697, .T. ) ;
#15895 = CARTESIAN_POINT ( 'NONE',  ( 20.00000000000001066, 60.00000000000000711, 24.99999999999998579 ) ) ;
#15896 = AXIS2_PLACEMENT_3D ( 'NONE', #12887, #22061, #10444 ) ;
#15897 = CARTESIAN_POINT ( 'NONE',  ( 153.6922820468853672, -10.00000000000000178, -9.266330736598359152 ) ) ;
#15898 = FACE_OUTER_BOUND ( 'NONE', #6763, .T. ) ;
#15899 = VECTOR ( 'NONE', #11636, 1000.000000000000000 ) ;
#15900 = LINE ( 'NONE', #6758, #2682 ) ;
#15901 = VECTOR ( 'NONE', #4426, 1000.000000000000000 ) ;
#15902 = UNCERTAINTY_MEASURE_WITH_UNIT (LENGTH_MEASURE( 1.000000000000000082E-05 ), #4940, 'distance_accuracy_value', 'NONE');
#15903 = CARTESIAN_POINT ( 'NONE',  ( 12.49860086554322436, 8.570087612320898884, -15.13128986298120537 ) ) ;
#15904 = LINE ( 'NONE', #2196, #17046 ) ;
#15905 = CARTESIAN_POINT ( 'NONE',  ( 151.1922820468853672, -1.999999999999976241, -2.083034168790677043 ) ) ;
#15906 = ORIENTED_EDGE ( 'NONE', *, *, #24246, .T. ) ;
#15907 = CARTESIAN_POINT ( 'NONE',  ( 0.000000000000000000, 0.000000000000000000, 23.00000000000000000 ) ) ;
#15908 = CARTESIAN_POINT ( 'NONE',  ( 18.11961939296043056, 8.971021047410516758, -18.23824686698257125 ) ) ;
#15909 = LINE ( 'NONE', #25389, #12190 ) ;
#15910 = LINE ( 'NONE', #4326, #17988 ) ;
#15912 = EDGE_LOOP ( 'NONE', ( #21949, #3130, #4247, #28737 ) ) ;
#15911 = CARTESIAN_POINT ( 'NONE',  ( 25.45462155318426767, -0.2439708902934435431, -15.99927030562601438 ) ) ;
#15913 = VERTEX_POINT ( 'NONE', #5512 ) ;
#15914 = CARTESIAN_POINT ( 'NONE',  ( 152.0152310637604955, -10.00000000000000178, -8.721423840594312082 ) ) ;
#15915 = CARTESIAN_POINT ( 'NONE',  ( 12.31319128649213646, 9.546177831575306527, -15.27906485473354792 ) ) ;
#15916 = EDGE_CURVE ( 'NONE', #18267, #25189, #14793, .T. ) ;
#15917 = EDGE_LOOP ( 'NONE', ( #14672, #28752, #19664, #12394 ) ) ;
#15918 = CARTESIAN_POINT ( 'NONE',  ( 34.11209566957792561, -15.73109017586260272, -19.92372960426217787 ) ) ;
#15919 = CARTESIAN_POINT ( 'NONE',  ( 168.6922820468853956, -9.999999999999996447, -32.39392330124607611 ) ) ;
#15920 = CARTESIAN_POINT ( 'NONE',  ( 28.12266609392075267, -5.599633216697744942, -16.00068813756295327 ) ) ;
#15921 = DIRECTION ( 'NONE',  ( -2.698458740408365879E-16, 1.000000000000000000, 0.000000000000000000 ) ) ;
#15922 = CARTESIAN_POINT ( 'NONE',  ( 25.85951265464835203, -2.375871015539448461, -16.96122936427994787 ) ) ;
#15923 = ORIENTED_EDGE ( 'NONE', *, *, #15553, .T. ) ;
#15924 = CARTESIAN_POINT ( 'NONE',  ( -28.20515957282649921, 30.94299554780361206, 9.999999999999998224 ) ) ;
#15925 = CARTESIAN_POINT ( 'NONE',  ( 30.28288205714520132, -11.65814127372701670, -12.00898047443557459 ) ) ;
#15926 = VECTOR ( 'NONE', #21328, 1000.000000000000000 ) ;
#15927 = CARTESIAN_POINT ( 'NONE',  ( 27.75006011364712322, -11.91879133414019698, -17.49150313904273801 ) ) ;
#15928 = EDGE_CURVE ( 'NONE', #28006, #20351, #10223, .T. ) ;
#15929 = CIRCLE ( 'NONE', #2794, 5.000000000000000888 ) ;
#15930 = EDGE_CURVE ( 'NONE', #29592, #19798, #13264, .T. ) ;
#15931 = EDGE_CURVE ( 'NONE', #3131, #4293, #2000, .T. ) ;
#15932 = EDGE_CURVE ( 'NONE', #11734, #11863, #29516, .T. ) ;
#15933 = EDGE_LOOP ( 'NONE', ( #6787, #25506, #13202, #10879 ) ) ;
#15934 = ORIENTED_EDGE ( 'NONE', *, *, #18379, .F. ) ;
#15935 = CARTESIAN_POINT ( 'NONE',  ( -2.678494666091066456, -3.072372537026392791, -2.415789719053448970 ) ) ;
#15936 = VECTOR ( 'NONE', #6308, 1000.000000000000114 ) ;
#15937 = CARTESIAN_POINT ( 'NONE',  ( 163.6922820468853388, -1.999999999999973133, -23.73366926340167282 ) ) ;
#15938 = PLANE ( 'NONE',  #5861 ) ;
#15939 = CARTESIAN_POINT ( 'NONE',  ( 139.5152310637605808, -1.999999999999978684, -30.37205893520530964 ) ) ;
#15940 = DIRECTION ( 'NONE',  ( -0.8660254037844370423, -0.5000000000000027756, 0.000000000000000000 ) ) ;
#15941 = VECTOR ( 'NONE', #24301, 1000.000000000000000 ) ;
#15942 = DIRECTION ( 'NONE',  ( 1.000000000000000000, 2.698458740408365879E-16, -1.110223024625156540E-16 ) ) ;
#15943 = CARTESIAN_POINT ( 'NONE',  ( 24.94059380785660451, 0.5691772567322460619, -14.01379559947946518 ) ) ;
#15944 = CARTESIAN_POINT ( 'NONE',  ( 16.54288150113237066, 3.399532473721276649, -19.15960874834559746 ) ) ;
#15945 = CARTESIAN_POINT ( 'NONE',  ( 31.73602415849877900, -9.487789691486469223, -15.56998832973926916 ) ) ;
#15946 = AXIS2_PLACEMENT_3D ( 'NONE', #23788, #22198, #19909 ) ;
#15947 = CARTESIAN_POINT ( 'NONE',  ( 12.07641845611955489, 8.540206757827041528, -15.45582622123028216 ) ) ;
#15948 = DIRECTION ( 'NONE',  ( 0.000000000000000000, 0.000000000000000000, 1.000000000000000000 ) ) ;
#15949 = LINE ( 'NONE', #13666, #6604 ) ;
#15950 = CARTESIAN_POINT ( 'NONE',  ( 9.688134281814004822, 16.13443519152062677, -17.87669530545171881 ) ) ;
#15951 = DIRECTION ( 'NONE',  ( 0.3090169943749475623, 8.338696094058001131E-17, 0.9510565162951536422 ) ) ;
#15952 = EDGE_LOOP ( 'NONE', ( #14985, #20616, #17171, #25653 ) ) ;
#15953 = CYLINDRICAL_SURFACE ( 'NONE', #19284, 4.250000000000000000 ) ;
#15954 = CARTESIAN_POINT ( 'NONE',  ( 12.49977518293622758, 8.570603418560722275, -15.13035415120363325 ) ) ;
#15955 = VERTEX_POINT ( 'NONE', #18292 ) ;
#15956 = FACE_BOUND ( 'NONE', #12151, .T. ) ;
#15957 = CARTESIAN_POINT ( 'NONE',  ( 152.0152310637605808, -10.00000000000000000, -34.70218595412750773 ) ) ;
#15958 = DIRECTION ( 'NONE',  ( 0.9510565162951536422, 0.000000000000000000, -0.3090169943749475623 ) ) ;
#15959 = ORIENTED_EDGE ( 'NONE', *, *, #14574, .F. ) ;
#15960 = ORIENTED_EDGE ( 'NONE', *, *, #25246, .T. ) ;
#15961 = CARTESIAN_POINT ( 'NONE',  ( 9.112637166705713554, 16.18088265059586561, -17.05468042929993189 ) ) ;
#15962 = CARTESIAN_POINT ( 'NONE',  ( 35.54750751241274287, -23.17963522693337453, -18.53372063443203999 ) ) ;
#15963 = ORIENTED_EDGE ( 'NONE', *, *, #1239, .T. ) ;
#15964 = CARTESIAN_POINT ( 'NONE',  ( 20.66677465483945397, 4.408179161683285052, -13.64328152160912033 ) ) ;
#15965 = EDGE_CURVE ( 'NONE', #2298, #21422, #20587, .T. ) ;
#15966 = CARTESIAN_POINT ( 'NONE',  ( 15.71409287621466788, 5.292507472020409942, -15.15310296786427635 ) ) ;
#15967 = ADVANCED_FACE ( 'NONE', ( #27209 ), #29969, .T. ) ;
#15968 = VECTOR ( 'NONE', #1683, 1000.000000000000000 ) ;
#15969 = EDGE_CURVE ( 'NONE', #27920, #2723, #11133, .T. ) ;
#15970 = CARTESIAN_POINT ( 'NONE',  ( -5.000000000000006217, -2.220446049250313870E-15, -4.974599999999998801 ) ) ;
#15971 = EDGE_CURVE ( 'NONE', #3306, #18890, #4424, .T. ) ;
#15972 = CARTESIAN_POINT ( 'NONE',  ( 22.17025134254096130, -8.444422103036636429, -16.38876926059057126 ) ) ;
#15973 = VECTOR ( 'NONE', #28442, 1000.000000000000000 ) ;
#15974 = EDGE_LOOP ( 'NONE', ( #14596, #26109, #536, #21734 ) ) ;
#15975 = PLANE ( 'NONE',  #27961 ) ;
#15977 = ORIENTED_EDGE ( 'NONE', *, *, #5010, .F. ) ;
#15976 = DIRECTION ( 'NONE',  ( 0.000000000000000000, 0.000000000000000000, 1.000000000000000000 ) ) ;
#15978 = FACE_BOUND ( 'NONE', #14292, .T. ) ;
#15979 = CARTESIAN_POINT ( 'NONE',  ( 153.6922820468854241, -1.999999999999974909, -26.58683881228715862 ) ) ;
#15980 = ORIENTED_EDGE ( 'NONE', *, *, #18612, .F. ) ;
#15981 = CARTESIAN_POINT ( 'NONE',  ( 34.62340031318386480, -17.02811109401968181, -19.03596318374462726 ) ) ;
#15982 = CARTESIAN_POINT ( 'NONE',  ( 12.65299103417153681, 7.585129394224154886, -15.00786874580416530 ) ) ;
#15983 = ORIENTED_EDGE ( 'NONE', *, *, #8242, .T. ) ;
#15984 = VECTOR ( 'NONE', #24516, 1000.000000000000000 ) ;
#15985 = CARTESIAN_POINT ( 'NONE',  ( 26.72610680620850232, -7.491537437428757329, -18.63066883040512067 ) ) ;
#15986 = CARTESIAN_POINT ( 'NONE',  ( 2.678494666091048693, 3.072372537026350159, -0.03421028094652719953 ) ) ;
#15987 = CARTESIAN_POINT ( 'NONE',  ( 10.47151541139924547, 16.45450612959241354, -17.33501744001014444 ) ) ;
#15988 = CARTESIAN_POINT ( 'NONE',  ( 172.7287565553229456, -1.999999999999970468, 0.5000000000000029976 ) ) ;
#15989 = DIRECTION ( 'NONE',  ( -0.9510565162951536422, -2.566386769018988816E-16, -0.3090169943749472292 ) ) ;
#15990 = ORIENTED_EDGE ( 'NONE', *, *, #19896, .T. ) ;
#15991 = AXIS2_PLACEMENT_3D ( 'NONE', #7902, #5621, #5470 ) ;
#15992 = DIRECTION ( 'NONE',  ( 0.3090169943749472292, 8.338696094057992503E-17, -0.9510565162951536422 ) ) ;
#15993 = DIRECTION ( 'NONE',  ( -0.9510565162951536422, -2.566386769018988816E-16, -0.3090169943749472292 ) ) ;
#15994 = ORIENTED_EDGE ( 'NONE', *, *, #15363, .F. ) ;
#15995 = ORIENTED_EDGE ( 'NONE', *, *, #22496, .F. ) ;
#15996 = LINE ( 'NONE', #4264, #17386 ) ;
#15997 = VECTOR ( 'NONE', #5471, 1000.000000000000000 ) ;
#15998 = ORIENTED_EDGE ( 'NONE', *, *, #1318, .F. ) ;
#15999 = CARTESIAN_POINT ( 'NONE',  ( 10.89980385979276356, 10.57756405496316710, -17.37562731196375410 ) ) ;
#16000 = CARTESIAN_POINT ( 'NONE',  ( 20.06573045921589227, -2.681363122285017386, -18.07621394912722934 ) ) ;
#16001 = CARTESIAN_POINT ( 'NONE',  ( 24.51656338950621361, -2.114370418465405521, -18.20187689272319176 ) ) ;
#16002 = CARTESIAN_POINT ( 'NONE',  ( 19.23896461120675383, 4.098237937441782996, -14.15247350351863886 ) ) ;
#16003 = LINE ( 'NONE', #13415, #27738 ) ;
#16004 = EDGE_CURVE ( 'NONE', #10540, #24599, #20282, .T. ) ;
#16005 = DIRECTION ( 'NONE',  ( -0.9510565162951536422, -2.566386769018988816E-16, -0.3090169943749472292 ) ) ;
#16006 = ADVANCED_FACE ( 'NONE', ( #13718 ), #4273, .F. ) ;
#16007 = VERTEX_POINT ( 'NONE', #8683 ) ;
#16008 = CARTESIAN_POINT ( 'NONE',  ( 21.48529164538665981, 5.106035544247377267, -18.65531623833433628 ) ) ;
#16009 = CARTESIAN_POINT ( 'NONE',  ( 0.000000000000000000, 0.000000000000000000, 0.000000000000000000 ) ) ;
#16010 = LINE ( 'NONE', #8539, #9358 ) ;
#16011 = VECTOR ( 'NONE', #15671, 1000.000000000000114 ) ;
#16012 = VECTOR ( 'NONE', #20333, 1000.000000000000000 ) ;
#16013 = AXIS2_PLACEMENT_3D ( 'NONE', #26094, #453, #16310 ) ;
#16014 = CARTESIAN_POINT ( 'NONE',  ( 10.35864918915110877, 16.97212501191939538, -19.66666666666842644 ) ) ;
#16015 = CARTESIAN_POINT ( 'NONE',  ( 14.97564302476352971, -5.000000000000013323, 46.09028999592811005 ) ) ;
#16016 = FACE_OUTER_BOUND ( 'NONE', #9831, .T. ) ;
#16017 = ORIENTED_EDGE ( 'NONE', *, *, #25044, .T. ) ;
#16018 = ORIENTED_EDGE ( 'NONE', *, *, #30122, .T. ) ;
#16019 = LINE ( 'NONE', #18009, #20714 ) ;
#16020 = CARTESIAN_POINT ( 'NONE',  ( 19.11618317516819587, 7.271703427217982352, -19.10559232466456692 ) ) ;
#16021 = CARTESIAN_POINT ( 'NONE',  ( 11.28421916535349112, 16.64009977454265865, -16.78120545242191142 ) ) ;
#16022 = CARTESIAN_POINT ( 'NONE',  ( 172.0152310637605240, -1.999999999999969358, -32.93883019725009120 ) ) ;
#16023 = ORIENTED_EDGE ( 'NONE', *, *, #18448, .F. ) ;
#16024 = EDGE_CURVE ( 'NONE', #30179, #17865, #18148, .T. ) ;
#16025 = VERTEX_POINT ( 'NONE', #8536 ) ;
#16026 = CARTESIAN_POINT ( 'NONE',  ( 9.879812780108833792, 16.57527415160161510, -16.52987074417163527 ) ) ;
#16027 = PRODUCT_RELATED_PRODUCT_CATEGORY ( 'part', '', ( #14920 ) ) ;
#16028 = CARTESIAN_POINT ( 'NONE',  ( 9.641485839925177714, 17.66827187890266160, -17.87200850766020110 ) ) ;
#16029 = DIRECTION ( 'NONE',  ( -0.8090169943749474513, -2.183098979609982436E-16, 0.5877852522924731371 ) ) ;
#16030 = LINE ( 'NONE', #1712, #2814 ) ;
#16031 = DIRECTION ( 'NONE',  ( -6.938893903907227392E-16, 0.000000000000000000, -1.000000000000000000 ) ) ;
#16032 = VERTEX_POINT ( 'NONE', #20137 ) ;
#16033 = CARTESIAN_POINT ( 'NONE',  ( 13.00452062571394229, 9.576253617860157163, -16.00682707811506233 ) ) ;
#16034 = VECTOR ( 'NONE', #27702, 1000.000000000000000 ) ;
#16035 = CARTESIAN_POINT ( 'NONE',  ( 35.34711162051457478, -16.78689235204268115, -20.22678452305727603 ) ) ;
#16036 = CARTESIAN_POINT ( 'NONE',  ( 24.18219217278060995, -6.970120066757704791, -14.18070892486464629 ) ) ;
#16037 = ORIENTED_EDGE ( 'NONE', *, *, #2235, .T. ) ;
#16038 = DIRECTION ( 'NONE',  ( -0.5877852522924731371, 0.000000000000000000, 0.8090169943749474513 ) ) ;
#16039 = AXIS2_PLACEMENT_3D ( 'NONE', #17876, #4013, #29411 ) ;
#16040 = DIRECTION ( 'NONE',  ( -2.698458740408365879E-16, 1.000000000000000000, 0.000000000000000000 ) ) ;
#16041 = APPLICATION_PROTOCOL_DEFINITION ( 'draft international standard', 'automotive_design', 1998, #1518 ) ;
#16042 = CARTESIAN_POINT ( 'NONE',  ( 14.93998017692337221, 5.301442995092576105, -18.84457556472494488 ) ) ;
#16043 = CARTESIAN_POINT ( 'NONE',  ( 21.03482577225312156, -5.582666113748667058, -14.36824825895596014 ) ) ;
#16044 = ORIENTED_EDGE ( 'NONE', *, *, #14160, .T. ) ;
#16045 = CARTESIAN_POINT ( 'NONE',  ( 161.1922820468853388, -4.999999999999973355, -13.59645775552055902 ) ) ;
#16046 = ORIENTED_EDGE ( 'NONE', *, *, #10517, .F. ) ;
#16047 = LINE ( 'NONE', #25522, #1856 ) ;
#16048 = VECTOR ( 'NONE', #13286, 1000.000000000000000 ) ;
#16049 = DIRECTION ( 'NONE',  ( -2.698458740408365879E-16, 1.000000000000000000, 0.000000000000000000 ) ) ;
#16050 = DIRECTION ( 'NONE',  ( 0.5877852522924731371, 0.000000000000000000, 0.8090169943749474513 ) ) ;
#16051 = CARTESIAN_POINT ( 'NONE',  ( 10.33931768503335924, 18.38068274058360885, -17.76381606660089929 ) ) ;
#16052 = AXIS2_PLACEMENT_3D ( 'NONE', #6837, #6236, #15529 ) ;
#16053 = CARTESIAN_POINT ( 'NONE',  ( 31.88113401528661939, -11.03952345999570994, -14.96145667752709763 ) ) ;
#16054 = EDGE_CURVE ( 'NONE', #16025, #1829, #13416, .T. ) ;
#16055 = ADVANCED_FACE ( 'NONE', ( #11421 ), #17991, .T. ) ;
#16056 = EDGE_LOOP ( 'NONE', ( #257, #6822 ) ) ;
#16057 = PLANE ( 'NONE',  #827 ) ;
#16058 = EDGE_LOOP ( 'NONE', ( #9716, #6620, #22526, #23949 ) ) ;
#16059 = CARTESIAN_POINT ( 'NONE',  ( 9.826288910175632552, 16.82074144182198694, -16.60662094963572244 ) ) ;
#16060 = ADVANCED_FACE ( 'NONE', ( #8977 ), #2294, .T. ) ;
#16061 = CARTESIAN_POINT ( 'NONE',  ( 28.05683000375443825, -12.20169833507544865, -14.26034257730772126 ) ) ;
#16062 = DIRECTION ( 'NONE',  ( -0.9510565162951536422, -2.566386769018988323E-16, 0.3090169943749475623 ) ) ;
#16063 = CARTESIAN_POINT ( 'NONE',  ( 144.7287565553230309, -1.999999999999977129, -25.16025403784439973 ) ) ;
#16064 = EDGE_CURVE ( 'NONE', #16652, #11518, #1692, .T. ) ;
#16066 = ORIENTED_EDGE ( 'NONE', *, *, #7837, .T. ) ;
#16065 = LINE ( 'NONE', #30178, #18529 ) ;
#16067 = ORIENTED_EDGE ( 'NONE', *, *, #18138, .F. ) ;
#16068 = LINE ( 'NONE', #27717, #7120 ) ;
#16069 = CARTESIAN_POINT ( 'NONE',  ( 12.24830724310059082, 9.517209185634078139, -15.33080109912759070 ) ) ;
#16070 = CARTESIAN_POINT ( 'NONE',  ( 35.54787733059053778, -22.18129662410796854, -18.46719521006932396 ) ) ;
#16071 = CARTESIAN_POINT ( 'NONE',  ( 132.0152310637605808, -1.999999999999981348, -24.27857615940569147 ) ) ;
#16072 = FACE_OUTER_BOUND ( 'NONE', #20911, .T. ) ;
#16073 = CARTESIAN_POINT ( 'NONE',  ( 20.31058213454123162, -2.053861134507735109, -16.68646832148754200 ) ) ;
#16074 = VERTEX_POINT ( 'NONE', #30114 ) ;
#16075 = AXIS2_PLACEMENT_3D ( 'NONE', #9160, #2490, #21081 ) ;
#16076 = CARTESIAN_POINT ( 'NONE',  ( 4.000000000000000000, -0.7779732554280925916, -0.03354435108167886509 ) ) ;
#16077 = VERTEX_POINT ( 'NONE', #18454 ) ;
#16078 = AXIS2_PLACEMENT_3D ( 'NONE', #19483, #26844, #19627 ) ;
#16079 = CARTESIAN_POINT ( 'NONE',  ( 18.68520274485960542, 10.62608585526774441, -17.78552708330943588 ) ) ;
#16080 = CARTESIAN_POINT ( 'NONE',  ( 28.61400761516875590, -9.413816014945153299, -13.42719155385534080 ) ) ;
#16081 = VECTOR ( 'NONE', #16996, 1000.000000000000000 ) ;
#16082 = VECTOR ( 'NONE', #23773, 1000.000000000000000 ) ;
#16083 = ORIENTED_EDGE ( 'NONE', *, *, #14439, .F. ) ;
#16084 = DIRECTION ( 'NONE',  ( -1.000000000000000000, -4.440892098500622217E-16, 0.000000000000000000 ) ) ;
#16085 = CARTESIAN_POINT ( 'NONE',  ( 152.0152310637604955, -4.999999999999976907, -8.721423840594312082 ) ) ;
#16086 = ORIENTED_EDGE ( 'NONE', *, *, #28876, .F. ) ;
#16087 = CARTESIAN_POINT ( 'NONE',  ( 167.2287565553229172, -9.999999999999998224, -12.16987298107780369 ) ) ;
#16088 = VECTOR ( 'NONE', #207, 999.9999999999998863 ) ;
#16089 = LINE ( 'NONE', #2082, #5765 ) ;
#16090 = DIRECTION ( 'NONE',  ( 0.9510565162951536422, 0.000000000000000000, -0.3090169943749475623 ) ) ;
#16091 = DIRECTION ( 'NONE',  ( -0.9510565162951536422, 0.000000000000000000, -0.3090169943749472292 ) ) ;
#16092 = CARTESIAN_POINT ( 'NONE',  ( 25.07632161252335123, -1.101686516974712315, -19.85338880782979132 ) ) ;
#16093 = CARTESIAN_POINT ( 'NONE',  ( 19.23896461120675383, 4.098237937441782996, -14.15247350351863886 ) ) ;
#16094 = EDGE_CURVE ( 'NONE', #1424, #19824, #18684, .T. ) ;
#16095 = CARTESIAN_POINT ( 'NONE',  ( 31.38423252821215570, -10.20947814759437655, -16.80760986317607930 ) ) ;
#16097 = CARTESIAN_POINT ( 'NONE',  ( 154.5152310637604671, -1.999999999999975353, -4.391296821672111328 ) ) ;
#16096 = VECTOR ( 'NONE', #19652, 1000.000000000000000 ) ;
#16098 = CARTESIAN_POINT ( 'NONE',  ( 11.51951884677450266, 9.108496074915260365, -15.83757232928968683 ) ) ;
#16099 = EDGE_CURVE ( 'NONE', #6302, #29149, #28552, .T. ) ;
#16100 = EDGE_CURVE ( 'NONE', #20699, #28260, #26088, .T. ) ;
#16101 = FACE_OUTER_BOUND ( 'NONE', #15952, .T. ) ;
#16102 = CARTESIAN_POINT ( 'NONE',  ( 14.97081799254939050, -5.000000000000013323, -46.07544007371636496 ) ) ;
#16103 = EDGE_CURVE ( 'NONE', #4171, #17166, #7308, .T. ) ;
#16105 = EDGE_LOOP ( 'NONE', ( #24147, #2096, #22338, #7822 ) ) ;
#16104 = CARTESIAN_POINT ( 'NONE',  ( 5.000000000000000000, 6.123233995736766282E-16, 18.00000000000000000 ) ) ;
#16106 = ORIENTED_EDGE ( 'NONE', *, *, #18692, .F. ) ;
#16107 = DIRECTION ( 'NONE',  ( -2.698458740408365879E-16, 1.000000000000000000, 0.000000000000000000 ) ) ;
#16108 = CARTESIAN_POINT ( 'NONE',  ( 12.50016782010997751, 8.570776461014483871, -15.13004124836345632 ) ) ;
#16109 = ORIENTED_EDGE ( 'NONE', *, *, #6265, .F. ) ;
#16110 = CARTESIAN_POINT ( 'NONE',  ( 141.1922820468854525, -10.00000000000000533, -13.59645775552055902 ) ) ;
#16111 = CARTESIAN_POINT ( 'NONE',  ( 174.5152310637604955, -1.999999999999968914, -28.60870317832789667 ) ) ;
#16112 = APPLICATION_CONTEXT ( 'automotive_design' ) ;
#16113 = DIRECTION ( 'NONE',  ( 1.000000000000000000, 2.698458740408365879E-16, -1.110223024625156540E-16 ) ) ;
#16114 = ORIENTED_EDGE ( 'NONE', *, *, #1969, .F. ) ;
#16115 = CARTESIAN_POINT ( 'NONE',  ( 9.115110896146415342, 16.16953781205366170, -17.05365751988364309 ) ) ;
#16117 = AXIS2_PLACEMENT_3D ( 'NONE', #20388, #20238, #15958 ) ;
#16116 = CARTESIAN_POINT ( 'NONE',  ( 33.08402606333302742, -12.15068820457383403, -20.63309441556253176 ) ) ;
#16118 = CARTESIAN_POINT ( 'NONE',  ( 14.32916401545863039, 6.225515681311286187, -14.04012878508491369 ) ) ;
#16119 = VECTOR ( 'NONE', #325, 1000.000000000000000 ) ;
#16120 = CARTESIAN_POINT ( 'NONE',  ( 19.26077778332419044, 5.765437233969479713, -18.81236659294151892 ) ) ;
#16121 = CARTESIAN_POINT ( 'NONE',  ( 149.5152310637605240, -1.999999999999976241, -13.05155085951651195 ) ) ;
#16122 = CARTESIAN_POINT ( 'NONE',  ( 18.61935276534875783, -1.259532457306228315, -15.72749031817820331 ) ) ;
#16123 = EDGE_LOOP ( 'NONE', ( #29541, #27238 ) ) ;
#16124 = DIRECTION ( 'NONE',  ( -2.908569913943825554E-16, 1.000000000000000000, -0.000000000000000000 ) ) ;
#16125 = EDGE_CURVE ( 'NONE', #21788, #8702, #2595, .T. ) ;
#16127 = ORIENTED_EDGE ( 'NONE', *, *, #19880, .T. ) ;
#16126 = CARTESIAN_POINT ( 'NONE',  ( 137.0152310637605808, -10.00000000000000533, -26.04193191628310800 ) ) ;
#16128 = VERTEX_POINT ( 'NONE', #26239 ) ;
#16129 = FACE_OUTER_BOUND ( 'NONE', #6667, .T. ) ;
#16130 = VECTOR ( 'NONE', #5452, 1000.000000000000000 ) ;
#16131 = LINE ( 'NONE', #15682, #4395 ) ;
#16132 = CARTESIAN_POINT ( 'NONE',  ( 34.49426285277334614, -12.00696374527110066, -18.89673795385250799 ) ) ;
#16133 = AXIS2_PLACEMENT_3D ( 'NONE', #27281, #6626, #17760 ) ;
#16134 = CARTESIAN_POINT ( 'NONE',  ( 11.57911078346310774, 7.697743364462890980, -15.81898674067912225 ) ) ;
#16135 = ORIENTED_EDGE ( 'NONE', *, *, #10213, .T. ) ;
#16136 = ADVANCED_FACE ( 'NONE', ( #7604 ), #16909, .T. ) ;
#16137 = EDGE_CURVE ( 'NONE', #19023, #19635, #9276, .T. ) ;
#16138 = DIRECTION ( 'NONE',  ( 0.000000000000000000, -1.000000000000000000, 0.000000000000000000 ) ) ;
#16139 = CARTESIAN_POINT ( 'NONE',  ( 3.673643420401897952, 2.497823135841248821, -0.2484800633749905674 ) ) ;
#16140 = ADVANCED_FACE ( 'NONE', ( #28097 ), #25933, .T. ) ;
#16141 = CARTESIAN_POINT ( 'NONE',  ( 10.38089682401341385, 16.87009452252716102, -17.57504515238516873 ) ) ;
#16142 = CARTESIAN_POINT ( 'NONE',  ( 148.6922820468854525, -10.00000000000000178, -35.24709285013155835 ) ) ;
#16143 = EDGE_CURVE ( 'NONE', #4706, #1754, #4711, .T. ) ;
#16144 = ORIENTED_EDGE ( 'NONE', *, *, #11954, .F. ) ;
#16145 = CARTESIAN_POINT ( 'NONE',  ( 172.2287565553229456, -4.999999999999970690, -20.83012701892220164 ) ) ;
#16146 = ORIENTED_EDGE ( 'NONE', *, *, #11110, .F. ) ;
#16147 = LINE ( 'NONE', #11268, #14412 ) ;
#16148 = PLANE ( 'NONE',  #16647 ) ;
#16149 = DIRECTION ( 'NONE',  ( 0.000000000000000000, 2.775557561562890735E-17, -1.000000000000000000 ) ) ;
#16150 = ORIENTED_EDGE ( 'NONE', *, *, #24705, .T. ) ;
#16151 = CARTESIAN_POINT ( 'NONE',  ( 9.667859621686535121, 16.22741736728331929, -17.88507964468380251 ) ) ;
#16152 = CARTESIAN_POINT ( 'NONE',  ( 17.03934835405440751, -0.5873649402599611102, -16.44458879923593742 ) ) ;
#16153 = CARTESIAN_POINT ( 'NONE',  ( 22.62754675296084983, -4.373583220233932423, -15.05708262856468060 ) ) ;
#16154 = CARTESIAN_POINT ( 'NONE',  ( 16.12927480167980576, 2.990883400875756326, -18.25071113400840517 ) ) ;
#16155 = DIRECTION ( 'NONE',  ( -0.8090169943749474513, -2.183098979609982436E-16, 0.5877852522924731371 ) ) ;
#16156 = CARTESIAN_POINT ( 'NONE',  ( 13.61739406634275618, -5.000000000000014211, -41.91002953721110202 ) ) ;
#16157 = CARTESIAN_POINT ( 'NONE',  ( 153.6922820468854525, -1.999999999999974465, -35.24709285013155835 ) ) ;
#16158 = CONICAL_SURFACE ( 'NONE', #15101, 5.000000000000006217, 0.9599310885968819207 ) ;
#16159 = CARTESIAN_POINT ( 'NONE',  ( 23.56138260001205964, -6.829566487537672259, -18.05074380722902916 ) ) ;
#16160 = B_SPLINE_CURVE_WITH_KNOTS ( 'NONE', 3,
 ( #19443, #12274, #28814, #7852, #17303, #26642 ),
 .UNSPECIFIED., .F., .F.,
 ( 4, 2, 4 ),
 ( 0.002336974151641542981, 0.003500975885716449756, 0.004664977619791356098 ),
 .UNSPECIFIED. ) ;
#16161 = ORIENTED_EDGE ( 'NONE', *, *, #26108, .T. ) ;
#16162 = CARTESIAN_POINT ( 'NONE',  ( 137.0152310637606092, -1.999999999999979572, -32.93883019725009120 ) ) ;
#16163 = LINE ( 'NONE', #20440, #1115 ) ;
#16164 = DIRECTION ( 'NONE',  ( 1.000000000000000000, 0.000000000000000000, 0.000000000000000000 ) ) ;
#16165 = AXIS2_PLACEMENT_3D ( 'NONE', #19427, #26023, #23570 ) ;
#16166 = LINE ( 'NONE', #11730, #19009 ) ;
#16167 = CARTESIAN_POINT ( 'NONE',  ( 0.000000000000000000, 0.000000000000000000, 1.700000000000000178 ) ) ;
#16168 = CARTESIAN_POINT ( 'NONE',  ( 10.36430886937160167, 16.94616899698690204, -17.73806594831300032 ) ) ;
#16169 = DIRECTION ( 'NONE',  ( -0.000000000000000000, -0.000000000000000000, 1.000000000000000000 ) ) ;
#16170 = CARTESIAN_POINT ( 'NONE',  ( 82.76178917566952009, -4.999999999999994671, 60.12995952993764348 ) ) ;
#16171 = ORIENTED_EDGE ( 'NONE', *, *, #1415, .T. ) ;
#16172 = ORIENTED_EDGE ( 'NONE', *, *, #20371, .F. ) ;
#16173 = ADVANCED_FACE ( 'NONE', ( #7163 ), #28257, .T. ) ;
#16174 = CARTESIAN_POINT ( 'NONE',  ( 147.0152310637604955, -1.999999999999977573, -0.06116980274991495881 ) ) ;
#16175 = AXIS2_PLACEMENT_3D ( 'NONE', #8388, #17692, #27053 ) ;
#16176 = CARTESIAN_POINT ( 'NONE',  ( 17.63704213852533442, 9.806822523219006271, -18.50018230520716145 ) ) ;
#16177 = CARTESIAN_POINT ( 'NONE',  ( 11.05558847800967648, 17.68862925033535660, -17.87192865789842955 ) ) ;
#16178 = CARTESIAN_POINT ( 'NONE',  ( 35.54859390953724585, -22.18451583373416014, -17.78191007148576475 ) ) ;
#16179 = EDGE_CURVE ( 'NONE', #28260, #7113, #23959, .T. ) ;
#16180 = ORIENTED_EDGE ( 'NONE', *, *, #995, .T. ) ;
#16181 = ORIENTED_EDGE ( 'NONE', *, *, #270, .T. ) ;
#16182 = ORIENTED_EDGE ( 'NONE', *, *, #19880, .F. ) ;
#16183 = CARTESIAN_POINT ( 'NONE',  ( 9.907423389235603395, 16.44864837861227969, -16.50891839478055090 ) ) ;
#16184 = CARTESIAN_POINT ( 'NONE',  ( 12.82404076521984670, 7.655871835264917102, -14.87190880308183871 ) ) ;
#16185 = FACE_OUTER_BOUND ( 'NONE', #6252, .T. ) ;
#16186 = CARTESIAN_POINT ( 'NONE',  ( 143.6922820468853956, -10.00000000000000533, -0.6060766987539614181 ) ) ;
#16187 = ORIENTED_EDGE ( 'NONE', *, *, #27289, .F. ) ;
#16188 = ORIENTED_EDGE ( 'NONE', *, *, #19614, .T. ) ;
#16189 = CARTESIAN_POINT ( 'NONE',  ( 7.347286611336969031, 4.995646404165290377, -4.503039949738246506 ) ) ;
#16190 = VERTEX_POINT ( 'NONE', #23487 ) ;
#16191 = CARTESIAN_POINT ( 'NONE',  ( 10.36007019289729847, 16.96560810760319882, -17.82599398985513872 ) ) ;
#16192 = CARTESIAN_POINT ( 'NONE',  ( 31.87116100697361887, -10.15812870475309815, -13.95024105943860171 ) ) ;
#16193 = CARTESIAN_POINT ( 'NONE',  ( 25.04068920418659161, -5.475481712173364990, -18.92835678451453774 ) ) ;
#16194 = VECTOR ( 'NONE', #4466, 1000.000000000000000 ) ;
#16195 = ORIENTED_EDGE ( 'NONE', *, *, #7085, .F. ) ;
#16196 = DIRECTION ( 'NONE',  ( 0.4108911781748706971, -0.9116843969807022496, 0.000000000000000000 ) ) ;
#16197 = DIRECTION ( 'NONE',  ( -2.207829878515935943E-16, 1.000000000000000000, 0.000000000000000000 ) ) ;
#16198 = DIRECTION ( 'NONE',  ( 0.000000000000000000, 0.000000000000000000, 1.000000000000000000 ) ) ;
#16199 = CARTESIAN_POINT ( 'NONE',  ( 18.45234147263269620, 6.489596213788811241, -14.85506563039705519 ) ) ;
#16200 = CARTESIAN_POINT ( 'NONE',  ( 21.56333733550986409, -5.354713294276967517, -13.65854400988971484 ) ) ;
#16201 = ORIENTED_EDGE ( 'NONE', *, *, #22669, .T. ) ;
#16202 = VECTOR ( 'NONE', #25143, 1000.000000000000000 ) ;
#16203 = EDGE_LOOP ( 'NONE', ( #16287, #5940 ) ) ;
#16204 = ADVANCED_FACE ( 'NONE', ( #7461 ), #4859, .T. ) ;
#16205 = DIRECTION ( 'NONE',  ( 0.9510565162951535312, 2.566386769018988816E-16, -0.3090169943749475623 ) ) ;
#16206 = DIRECTION ( 'NONE',  ( 0.000000000000000000, 0.000000000000000000, 1.000000000000000000 ) ) ;
#16207 = LINE ( 'NONE', #4165, #15557 ) ;
#16208 = AXIS2_PLACEMENT_3D ( 'NONE', #23087, #8877, #9171 ) ;
#16209 = CYLINDRICAL_SURFACE ( 'NONE', #5111, 3.000000000000002665 ) ;
#16210 = CARTESIAN_POINT ( 'NONE',  ( 10.71436926824426550, 16.66064837202128501, -15.95707641581892133 ) ) ;
#16211 = CARTESIAN_POINT ( 'NONE',  ( -8.000000000000000000, 0.000000000000000000, 15.00000000000000000 ) ) ;
#16212 = ORIENTED_EDGE ( 'NONE', *, *, #817, .T. ) ;
#16213 = CARTESIAN_POINT ( 'NONE',  ( 162.0152310637604955, -4.999999999999973355, -15.61832212156129707 ) ) ;
#16214 = ORIENTED_EDGE ( 'NONE', *, *, #28616, .F. ) ;
#16215 = CARTESIAN_POINT ( 'NONE',  ( 9.926830210242822972, 16.35964622367879784, -16.50025672554925293 ) ) ;
#16216 = VECTOR ( 'NONE', #13970, 1000.000000000000000 ) ;
#16217 = CARTESIAN_POINT ( 'NONE',  ( 18.67591552545227174, 7.243412299697878254, -16.30691131850022657 ) ) ;
#16218 = DIRECTION ( 'NONE',  ( -2.698458740408365879E-16, 1.000000000000000000, 0.000000000000000000 ) ) ;
#16219 = LINE ( 'NONE', #1751, #7653 ) ;
#16221 = ORIENTED_EDGE ( 'NONE', *, *, #14402, .T. ) ;
#16220 = CARTESIAN_POINT ( 'NONE',  ( 31.22280883588763700, -10.09333740185288875, -13.86128061636125786 ) ) ;
#16222 = VERTEX_POINT ( 'NONE', #20881 ) ;
#16223 = LINE ( 'NONE', #23866, #8581 ) ;
#16224 = CARTESIAN_POINT ( 'NONE',  ( 11.31663841827600692, 16.49142094814642334, -16.76779895092377615 ) ) ;
#16225 = ORIENTED_EDGE ( 'NONE', *, *, #1553, .T. ) ;
#16226 = CARTESIAN_POINT ( 'NONE',  ( 35.52583876341286384, -22.08228901593173177, -18.97221062538168113 ) ) ;
#16227 = LINE ( 'NONE', #4935, #4947 ) ;
#16228 = ORIENTED_EDGE ( 'NONE', *, *, #3077, .T. ) ;
#16229 = PLANE ( 'NONE',  #26211 ) ;
#16230 = CARTESIAN_POINT ( 'NONE',  ( 23.96437976099892708, -9.208260125601851698, -18.67152130837153123 ) ) ;
#16231 = VERTEX_POINT ( 'NONE', #294 ) ;
#16232 = DIRECTION ( 'NONE',  ( -0.8090169943749474513, -2.183098979609982436E-16, -0.5877852522924731371 ) ) ;
#16233 = CARTESIAN_POINT ( 'NONE',  ( 20.13607245741800611, 4.456688099076253629, -14.49627829575511129 ) ) ;
#16234 = CARTESIAN_POINT ( 'NONE',  ( 25.85465836959373220, -10.01954208144345770, -18.53069695322523103 ) ) ;
#16235 = ORIENTED_EDGE ( 'NONE', *, *, #11616, .F. ) ;
#16236 = EDGE_CURVE ( 'NONE', #26921, #19956, #26942, .T. ) ;
#16237 = LINE ( 'NONE', #2225, #2474 ) ;
#16238 = EDGE_CURVE ( 'NONE', #6539, #24548, #5015, .T. ) ;
#16239 = VECTOR ( 'NONE', #27130, 1000.000000000000000 ) ;
#16240 = DIRECTION ( 'NONE',  ( 0.5877852522924731371, 0.000000000000000000, 0.8090169943749474513 ) ) ;
#16241 = CARTESIAN_POINT ( 'NONE',  ( 132.0152310637605524, -1.999999999999981348, -26.04193191628310800 ) ) ;
#16242 = CARTESIAN_POINT ( 'NONE',  ( 157.0152310637605240, -10.00000000000000000, -15.61832212156129707 ) ) ;
#16243 = CARTESIAN_POINT ( 'NONE',  ( 9.644802874473198173, 17.65305953564175567, -17.69767226479352118 ) ) ;
#16244 = CARTESIAN_POINT ( 'NONE',  ( 20.36141319467227362, -5.793038086071195636, -16.11598603859005507 ) ) ;
#16245 = CARTESIAN_POINT ( 'NONE',  ( 21.81760893248375766, -3.923850722439390815, -13.93537712798182682 ) ) ;
#16246 = CARTESIAN_POINT ( 'NONE',  ( 32.41494245136814811, -10.61148775487728813, -19.57799680467864789 ) ) ;
#16247 =( NAMED_UNIT ( * ) PLANE_ANGLE_UNIT ( ) SI_UNIT ( $, .RADIAN. ) );
#16248 = DIRECTION ( 'NONE',  ( -0.5877852522924731371, -1.586114251531760728E-16, -0.8090169943749474513 ) ) ;
#16249 = CARTESIAN_POINT ( 'NONE',  ( 131.1922820468854241, -1.999999999999982236, -13.59645775552055547 ) ) ;
#16250 = CARTESIAN_POINT ( 'NONE',  ( 5.000000000000000888, 0.000000000000000000, 0.000000000000000000 ) ) ;
#16251 = CARTESIAN_POINT ( 'NONE',  ( 13.77718166750865869, 8.859676595473324312, -15.39100258941132182 ) ) ;
#16252 = VERTEX_POINT ( 'NONE', #18903 ) ;
#16253 = DIRECTION ( 'NONE',  ( 1.000000000000000000, 0.000000000000000000, 0.000000000000000000 ) ) ;
#16254 = CARTESIAN_POINT ( 'NONE',  ( 10.33811693838771717, 18.38618951776012267, -17.93331994345748726 ) ) ;
#16255 = ORIENTED_EDGE ( 'NONE', *, *, #3600, .T. ) ;
#16256 = PLANE ( 'NONE',  #19303 ) ;
#16257 = CARTESIAN_POINT ( 'NONE',  ( 159.5152310637605240, -1.999999999999973133, -19.94844914048349693 ) ) ;
#16258 = CARTESIAN_POINT ( 'NONE',  ( 15.94478687392618355, 4.193953704849600506, -19.05305658475056063 ) ) ;
#16259 = VECTOR ( 'NONE', #18611, 1000.000000000000000 ) ;
#16260 = EDGE_LOOP ( 'NONE', ( #8606, #12535, #27234, #25536 ) ) ;
#16261 = CARTESIAN_POINT ( 'NONE',  ( 34.31408884023914396, -17.63853849290766362, -21.02710884213126263 ) ) ;
#16262 = ORIENTED_EDGE ( 'NONE', *, *, #5811, .F. ) ;
#16263 = CARTESIAN_POINT ( 'NONE',  ( 22.68669718693540105, -3.283095500849226411, -14.44170700164887933 ) ) ;
#16264 = CARTESIAN_POINT ( 'NONE',  ( 16.70639138691818459, 6.939553047386250562, -20.38695695975560085 ) ) ;
#16265 = VERTEX_POINT ( 'NONE', #27954 ) ;
#16266 = CARTESIAN_POINT ( 'NONE',  ( 19.83814782303322133, -0.7621604502531613701, -13.87429439740111370 ) ) ;
#16267 = EDGE_CURVE ( 'NONE', #28698, #29509, #7011, .T. ) ;
#16268 = EDGE_CURVE ( 'NONE', #4554, #18145, #12021, .T. ) ;
#16269 = VERTEX_POINT ( 'NONE', #21494 ) ;
#16270 = EDGE_CURVE ( 'NONE', #7228, #16074, #9883, .T. ) ;
#16271 = DIRECTION ( 'NONE',  ( 0.9510565162951536422, 0.000000000000000000, -0.3090169943749475623 ) ) ;
#16273 = ORIENTED_EDGE ( 'NONE', *, *, #10448, .T. ) ;
#16272 = DIRECTION ( 'NONE',  ( 0.000000000000000000, 0.000000000000000000, -1.000000000000000000 ) ) ;
#16274 = ORIENTED_EDGE ( 'NONE', *, *, #15748, .T. ) ;
#16275 = CARTESIAN_POINT ( 'NONE',  ( 8.000000000000000000, 9.797174393178825657E-16, 15.00000000000000000 ) ) ;
#16276 = AXIS2_PLACEMENT_3D ( 'NONE', #9059, #8915, #18385 ) ;
#16277 = DIRECTION ( 'NONE',  ( -0.000000000000000000, -0.000000000000000000, -1.000000000000000000 ) ) ;
#16278 = CARTESIAN_POINT ( 'NONE',  ( 33.01527616964045109, -10.33189599206409959, -17.18388710919138873 ) ) ;
#16279 = CARTESIAN_POINT ( 'NONE',  ( 9.641350829061996919, 17.66889105593114806, -17.91548090047172437 ) ) ;
#16280 = VERTEX_POINT ( 'NONE', #5474 ) ;
#16281 = DIRECTION ( 'NONE',  ( 0.000000000000000000, -1.000000000000000000, 1.471414886128461471E-15 ) ) ;
#16282 = CARTESIAN_POINT ( 'NONE',  ( 161.1922820468853104, -1.999999999999974021, -4.936203717676158398 ) ) ;
#16283 = CIRCLE ( 'NONE', #7050, 1.499999999999996225 ) ;
#16284 = CARTESIAN_POINT ( 'NONE',  ( 10.35953768210033665, 16.96805026999784616, -17.84385765891457254 ) ) ;
#16285 = LINE ( 'NONE', #9711, #18989 ) ;
#16286 = FACE_OUTER_BOUND ( 'NONE', #6106, .T. ) ;
#16287 = ORIENTED_EDGE ( 'NONE', *, *, #16736, .F. ) ;
#16288 = DIRECTION ( 'NONE',  ( -2.698458740408365879E-16, 1.000000000000000000, 0.000000000000000000 ) ) ;
#16289 = LINE ( 'NONE', #433, #11707 ) ;
#16290 = ORIENTED_EDGE ( 'NONE', *, *, #1458, .T. ) ;
#16291 = DIRECTION ( 'NONE',  ( -0.5877852522924731371, -1.586114251531760728E-16, -0.8090169943749474513 ) ) ;
#16292 = ORIENTED_EDGE ( 'NONE', *, *, #23952, .F. ) ;
#16293 = CARTESIAN_POINT ( 'NONE',  ( 9.666872068725954392, 16.23194641104447911, -17.88584179299332533 ) ) ;
#16294 = ORIENTED_EDGE ( 'NONE', *, *, #1346, .F. ) ;
#16295 = CARTESIAN_POINT ( 'NONE',  ( 16.98604603105943767, -0.4850832133139416080, -17.48051239862526884 ) ) ;
#16296 = CARTESIAN_POINT ( 'NONE',  ( 21.05341046998850629, -2.558799731849103587, -14.42238450910079806 ) ) ;
#16297 = ORIENTED_EDGE ( 'NONE', *, *, #18366, .T. ) ;
#16298 = CARTESIAN_POINT ( 'NONE',  ( 20.38603433104324480, 7.363110203939331022, -17.91596102798271062 ) ) ;
#16299 = LINE ( 'NONE', #25614, #8672 ) ;
#16300 = CARTESIAN_POINT ( 'NONE',  ( -0.6527133886630267501, 8.860760056385757366, -0.4969600502617637638 ) ) ;
#16301 = VECTOR ( 'NONE', #29416, 1000.000000000000000 ) ;
#16302 = DIRECTION ( 'NONE',  ( 0.000000000000000000, 0.000000000000000000, 1.000000000000000000 ) ) ;
#16303 = CARTESIAN_POINT ( 'NONE',  ( 22.97938783112199701, -3.359759438970757017, -19.62490732200095067 ) ) ;
#16304 = EDGE_CURVE ( 'NONE', #24792, #11598, #19346, .T. ) ;
#16305 = EDGE_CURVE ( 'NONE', #23467, #29073, #21947, .T. ) ;
#16306 = ADVANCED_FACE ( 'NONE', ( #6074 ), #14757, .T. ) ;
#16307 = ORIENTED_EDGE ( 'NONE', *, *, #1239, .F. ) ;
#16308 = EDGE_CURVE ( 'NONE', #24567, #27103, #26862, .T. ) ;
#16309 = DIRECTION ( 'NONE',  ( -2.698458740408365879E-16, 1.000000000000000000, 0.000000000000000000 ) ) ;
#16310 = DIRECTION ( 'NONE',  ( -0.9510565162951536422, 0.000000000000000000, -0.3090169943749472292 ) ) ;
#16311 = CARTESIAN_POINT ( 'NONE',  ( 162.0152310637605240, -4.999999999999974243, -1.798730398669518271E-14 ) ) ;
#16312 = CARTESIAN_POINT ( 'NONE',  ( 20.00000000000017053, 34.64101615137744972, 14.00000000000000178 ) ) ;
#16313 = CARTESIAN_POINT ( 'NONE',  ( 10.35864918915110877, 16.97212501191939538, -17.92015940598198753 ) ) ;
#16314 = FACE_OUTER_BOUND ( 'NONE', #8947, .T. ) ;
#16315 = CARTESIAN_POINT ( 'NONE',  ( 33.41663030065195272, -12.60673267154789201, -19.71350710734569134 ) ) ;
#16316 = ORIENTED_EDGE ( 'NONE', *, *, #13008, .F. ) ;
#16317 = CARTESIAN_POINT ( 'NONE',  ( 11.96143972814086531, 7.837808674300617007, -16.77422427047595477 ) ) ;
#16318 = VERTEX_POINT ( 'NONE', #24245 ) ;
#16319 = DIRECTION ( 'NONE',  ( 0.5877852522924731371, 1.586114251531760728E-16, 0.8090169943749474513 ) ) ;
#16320 = VECTOR ( 'NONE', #9749, 1000.000000000000000 ) ;
#16321 = CARTESIAN_POINT ( 'NONE',  ( 20.50636976340433293, -0.9757509181830721356, -19.91080244439677571 ) ) ;
#16322 = CARTESIAN_POINT ( 'NONE',  ( 11.16343636398553052, 17.19402509784177369, -16.95964061678045454 ) ) ;
#16323 = CARTESIAN_POINT ( 'NONE',  ( 427.0000000000002274, 34.64101615137744972, 10.00000000000000178 ) ) ;
#16324 = VERTEX_POINT ( 'NONE', #15362 ) ;
#16325 = ORIENTED_EDGE ( 'NONE', *, *, #8357, .T. ) ;
#16326 = EDGE_LOOP ( 'NONE', ( #25587, #18314 ) ) ;
#16327 = CARTESIAN_POINT ( 'NONE',  ( 9.905109554012803130, 16.45925992188944420, -16.51025697316969953 ) ) ;
#16328 = LINE ( 'NONE', #16, #27735 ) ;
#16329 = CARTESIAN_POINT ( 'NONE',  ( 9.641350810849047548, 17.66889113945805789, -17.92981046679734547 ) ) ;
#16330 = DIRECTION ( 'NONE',  ( -2.698458740408365879E-16, 1.000000000000000000, 0.000000000000000000 ) ) ;
#16331 = CARTESIAN_POINT ( 'NONE',  ( 175.7287565553229456, -4.999999999999970690, -22.10610323145030520 ) ) ;
#16332 = ORIENTED_EDGE ( 'NONE', *, *, #5089, .T. ) ;
#16333 = CARTESIAN_POINT ( 'NONE',  ( 5.355005115540903304, 6.145890662064663168, -0.08224679563972060736 ) ) ;
#16334 = ORIENTED_EDGE ( 'NONE', *, *, #26256, .T. ) ;
#16335 = CARTESIAN_POINT ( 'NONE',  ( 10.49225533350670858, 16.35939020308235925, -17.32643665990597981 ) ) ;
#16336 = ORIENTED_EDGE ( 'NONE', *, *, #26361, .F. ) ;
#16337 = CARTESIAN_POINT ( 'NONE',  ( 36.54859590101256828, -22.18452478037840336, -18.26685560724362034 ) ) ;
#16338 = CARTESIAN_POINT ( 'NONE',  ( 25.67262840375075328, -3.322766148301121714, -14.04542551033457798 ) ) ;
#16339 = PLANE ( 'NONE',  #23791 ) ;
#16340 = CARTESIAN_POINT ( 'NONE',  ( 34.43765690731135720, -12.70119407716533111, -19.95187818093482335 ) ) ;
#16341 = DIRECTION ( 'NONE',  ( -1.000000000000000000, 0.000000000000000000, 0.000000000000000000 ) ) ;
#16342 = CARTESIAN_POINT ( 'NONE',  ( 14.82995595102070752, 5.192148136363496036, -18.54057990209784634 ) ) ;
#16343 = CARTESIAN_POINT ( 'NONE',  ( 26.72351632055398696, -11.69804524575189397, -15.34103589027250791 ) ) ;
#16344 = ADVANCED_FACE ( 'NONE', ( #22247 ), #12473, .T. ) ;
#16345 =( GEOMETRIC_REPRESENTATION_CONTEXT ( 3 ) GLOBAL_UNCERTAINTY_ASSIGNED_CONTEXT ( ( #23234 ) ) GLOBAL_UNIT_ASSIGNED_CONTEXT ( ( #2237, #243, #23277 ) ) REPRESENTATION_CONTEXT ( 'NONE', 'WORKASPACE' ) );
#16346 = B_SPLINE_CURVE_WITH_KNOTS ( 'NONE', 3,
 ( #1328, #17191, #6202, #19472, #8332, #17331, #15495, #17635, #13057, #22077, #24224, #12446, #28845, #26518, #26990, #3176, #6048, #15337, #14878, #3324, #12603, #26677, #5754, #15036, #24368, #19765, #29134, #6650, #27744, #29763, #30205, #13798, #1636, #9214, #27449, #20821, #15649, #4210, #1939, #13358, #9064, #8772, #27302, #6356, #18389, #11505, #18087, #22683, #3914, #1784, #25271, #11069, #22834, #15944, #4357, #23124, #13660, #22984, #6502, #24982, #20224, #6804, #29610, #2233, #10915, #16093, #18541, #27895, #29911, #30054, #22538, #20373, #2087, #18234, #6957, #8626, #24826, #25420, #15793, #11221, #17926, #25120, #4509, #13507, #11363, #13214, #4065, #20524, #8918, #27592, #20667, #4804, #14248, #9829, #19145, #26032, #7256, #687, #16854, #25879, #18697, #9974, #28502, #21277, #11813, #9366, #2543, #21588, #21128, #18839, #28355, #23430, #28042, #389, #28200, #7550, #23579, #240, #7098, #2675, #13944, #23738, #7411, #16398, #9517, #19289, #11662, #25721, #14550, #14097, #16555, #4958, #2835, #5262, #11961, #9675, #18997, #26181, #20976, #23897, #2389, #12121, #21436, #28645, #16711, #5106, #14396, #547, #2994, #12269, #16245, #25557, #4652, #23274, #85, #12868, #22181, #26485, #10580, #7991, #15150, #20047, #1291, #8140, #21732, #26954, #19586, #17156, #835, #22340, #3427, #22040, #17299, #7696, #10424, #1144, #26638, #1443, #19887, #12718, #3289, #19733, #12416, #10126, #17009, #15000, #15298, #5565, #5720, #6011, #13024, #24334, #29101, #14700, #7847, #24630, #14845, #24481, #17448, #19436, #12564, #24188, #21883, #3727, #26332, #28955, #26797, #5868, #28809, #10736, #24042, #29258, #994, #10277, #3579, #8290, #5415, #17599, #3141, #4025, #20634, #9025, #8440, #27264, #18349, #22948, #6463, #11180, #2048, #13320, #4474, #27705, #6164, #13764, #1742, #25380, #20186, #8731, #15756, #17884, #13617, #22644, #1599, #10876, #11327, #16053 ),
 .UNSPECIFIED., .F., .F.,
 ( 4, 2, 2, 2, 2, 2, 2, 2, 2, 2, 2, 2, 2, 2, 2, 2, 2, 2, 2, 2, 2, 2, 2, 2, 2, 2, 2, 2, 2, 2, 2, 2, 2, 2, 2, 2, 2, 2, 2, 2, 2, 2, 2, 2, 2, 2, 2, 2, 2, 2, 2, 2, 2, 2, 2, 2, 2, 2, 2, 2, 2, 2, 2, 2, 2, 2, 2, 2, 2, 2, 2, 2, 2, 2, 2, 2, 2, 2, 2, 2, 2, 2, 2, 2, 2, 2, 2, 2, 2, 2, 2, 2, 2, 2, 2, 2, 2, 2, 2, 2, 2, 2, 2, 2, 2, 2, 2, 2, 2, 2, 2, 2, 2, 2, 2, 2, 2, 2, 2, 2, 2, 2, 4 ),
 ( 0.000000000000000000, 0.007812500000000000000, 0.01464843750000000000, 0.02148437500000000000, 0.02832031250000000000, 0.03515625000000000000, 0.04882812500000000000, 0.05566406250000000000, 0.06250000000000000000, 0.06933593750000000000, 0.07617187500000000000, 0.08984375000000000000, 0.09667968750000000000, 0.1035156250000000000, 0.1103515625000000000, 0.1171875000000000000, 0.1240234375000000000, 0.1308593750000000000, 0.1376953125000000000, 0.1445312500000000000, 0.1513671875000000000, 0.1582031250000000000, 0.1718750000000000000, 0.1787109375000000000, 0.1855468750000000000, 0.1992187500000000000, 0.2060546875000000000, 0.2128906250000000000, 0.2197265625000000000, 0.2265625000000000000, 0.2402343750000000000, 0.2470703125000000000, 0.2539062500000000000, 0.2607421875000000000, 0.2675781250000000000, 0.2812500000000000000, 0.2880859375000000000, 0.2949218750000000000, 0.3017578125000000000, 0.3085937500000000000, 0.3154296875000000000, 0.3222656250000000000, 0.3291015625000000000, 0.3359375000000000000, 0.3496093750000000000, 0.3564453125000000000, 0.3632812500000000000, 0.3701171875000000000, 0.3769531250000000000, 0.3906250000000000000, 0.3974609375000000000, 0.4042968750000000000, 0.4179687500000000000, 0.4316406250000000000, 0.4384765625000000000, 0.4453125000000000000, 0.4521484375000000000, 0.4589843750000000000, 0.4658203125000000000, 0.4726562500000000000, 0.4794921875000000000, 0.4863281250000000000, 0.4931640625000000000, 0.5000000000000000000, 0.5078125000000000000, 0.5156250000000000000, 0.5234375000000000000, 0.5312500000000000000, 0.5390625000000000000, 0.5468750000000000000, 0.5625000000000000000, 0.5693359375000000000, 0.5761718750000000000, 0.5898437500000000000, 0.5966796875000000000, 0.6035156250000000000, 0.6103515625000000000, 0.6171875000000000000, 0.6308593750000000000, 0.6376953125000000000, 0.6445312500000000000, 0.6513671875000000000, 0.6582031250000000000, 0.6718750000000000000, 0.6787109375000000000, 0.6855468750000000000, 0.6992187500000000000, 0.7128906250000000000, 0.7197265625000000000, 0.7265625000000000000, 0.7333984375000000000, 0.7402343750000000000, 0.7470703125000000000, 0.7539062500000000000, 0.7607421875000000000, 0.7675781250000000000, 0.7744140625000000000, 0.7812500000000000000, 0.7890625000000000000, 0.7968750000000000000, 0.8046875000000000000, 0.8125000000000000000, 0.8203125000000000000, 0.8281250000000000000, 0.8437500000000000000, 0.8505859375000000000, 0.8574218750000000000, 0.8710937500000000000, 0.8779296875000000000, 0.8847656250000000000, 0.8916015625000000000, 0.8984375000000000000, 0.9121093750000000000, 0.9189453125000000000, 0.9257812500000000000, 0.9326171875000000000, 0.9394531250000000000, 0.9531250000000000000, 0.9589843750000000000, 0.9648437500000000000, 0.9765625000000000000, 0.9882812500000000000, 1.000000000000000000 ),
 .UNSPECIFIED. ) ;
#16347 = EDGE_CURVE ( 'NONE', #8301, #27211, #19792, .T. ) ;
#16349 = EDGE_LOOP ( 'NONE', ( #6455, #12539, #13570, #20995 ) ) ;
#16348 = EDGE_CURVE ( 'NONE', #5191, #27103, #14903, .T. ) ;
#16350 = LINE ( 'NONE', #25981, #28923 ) ;
#16351 = VECTOR ( 'NONE', #4964, 1000.000000000000000 ) ;
#16352 = LINE ( 'NONE', #11770, #27727 ) ;
#16353 = CARTESIAN_POINT ( 'NONE',  ( 168.6922820468853672, -9.999999999999996447, -26.58683881228715862 ) ) ;
#16354 = LINE ( 'NONE', #13761, #15333 ) ;
#16355 = AXIS2_PLACEMENT_3D ( 'NONE', #14594, #16601, #19041 ) ;
#16356 = CARTESIAN_POINT ( 'NONE',  ( 10.72091424521701519, 16.63063227333373462, -15.95414859203816782 ) ) ;
#16357 = LINE ( 'NONE', #2954, #14113 ) ;
#16358 = ORIENTED_EDGE ( 'NONE', *, *, #14203, .F. ) ;
#16359 = CARTESIAN_POINT ( 'NONE',  ( 175.7287565553229456, -4.999999999999969802, -13.44584919360591257 ) ) ;
#16360 = ORIENTED_EDGE ( 'NONE', *, *, #16445, .T. ) ;
#16361 = VECTOR ( 'NONE', #4485, 1000.000000000000000 ) ;
#16362 = CARTESIAN_POINT ( 'NONE',  ( 11.47276097331165623, 9.269810413962238371, -15.86095999428340697 ) ) ;
#16363 = ORIENTED_EDGE ( 'NONE', *, *, #7736, .F. ) ;
#16364 = VECTOR ( 'NONE', #23972, 1000.000000000000000 ) ;
#16365 = CARTESIAN_POINT ( 'NONE',  ( 15.96855819401819865, 6.783166013289068985, -19.29613786212107840 ) ) ;
#16366 = DIRECTION ( 'NONE',  ( -2.698458740408365879E-16, 1.000000000000000000, 0.000000000000000000 ) ) ;
#16367 = CARTESIAN_POINT ( 'NONE',  ( 120.0000000000000000, 20.00000000000000355, -15.00000000000000000 ) ) ;
#16368 = CARTESIAN_POINT ( 'NONE',  ( 27.11191462667604313, -11.78482644060662743, -13.28705938033944989 ) ) ;
#16369 = ORIENTED_EDGE ( 'NONE', *, *, #12802, .T. ) ;
#16370 = DIRECTION ( 'NONE',  ( -0.5877852522924731371, -1.586114251531760235E-16, 0.8090169943749474513 ) ) ;
#16371 = CARTESIAN_POINT ( 'NONE',  ( 11.27618196228310232, 16.67695941232857137, -16.78452903358395076 ) ) ;
#16372 = EDGE_CURVE ( 'NONE', #18739, #2712, #1059, .T. ) ;
#16373 = VECTOR ( 'NONE', #9969, 1000.000000000000000 ) ;
#16374 = CARTESIAN_POINT ( 'NONE',  ( 35.54859390953724585, -21.18451583373416014, -18.19919658220850422 ) ) ;
#16375 = CARTESIAN_POINT ( 'NONE',  ( 16.77165338796101324, 10.12286561294300569, -15.51291369241808304 ) ) ;
#16376 = CARTESIAN_POINT ( 'NONE',  ( 171.1922820468853104, -1.999999999999970912, -13.59645775552055902 ) ) ;
#16377 = CARTESIAN_POINT ( 'NONE',  ( 23.86193934616450818, -4.638293873783104537, -19.03466029786466152 ) ) ;
#16378 = ORIENTED_EDGE ( 'NONE', *, *, #19646, .T. ) ;
#16379 = DIRECTION ( 'NONE',  ( 0.3090169943749472292, 8.338696094057992503E-17, -0.9510565162951536422 ) ) ;
#16380 = SURFACE_STYLE_FILL_AREA ( #2221 ) ;
#16381 = CARTESIAN_POINT ( 'NONE',  ( 22.90957683611224738, 2.308586283387667581, -16.61139769879808625 ) ) ;
#16382 = CARTESIAN_POINT ( 'NONE',  ( 15.60254075764268755, 8.625145012302763092, -14.61600764054077395 ) ) ;
#16383 = AXIS2_PLACEMENT_3D ( 'NONE', #12740, #17766, #10602 ) ;
#16384 = ADVANCED_BREP_SHAPE_REPRESENTATION ( '', ( #11840, #13190 ), #12225 ) ;
#16385 = EDGE_CURVE ( 'NONE', #29420, #22008, #17216, .T. ) ;
#16386 = ORIENTED_EDGE ( 'NONE', *, *, #6642, .F. ) ;
#16388 = ORIENTED_EDGE ( 'NONE', *, *, #25246, .F. ) ;
#16387 = EDGE_CURVE ( 'NONE', #6140, #20355, #24394, .T. ) ;
#16389 = LINE ( 'NONE', #4500, #4393 ) ;
#16390 = VECTOR ( 'NONE', #29540, 1000.000000000000000 ) ;
#16391 = VECTOR ( 'NONE', #21678, 1000.000000000000000 ) ;
#16392 = PLANE ( 'NONE',  #26024 ) ;
#16393 = CARTESIAN_POINT ( 'NONE',  ( 154.7287565553230309, -4.999999999999975131, -33.82050807568879947 ) ) ;
#16394 = CARTESIAN_POINT ( 'NONE',  ( -8.000000000000001776, -4.336808689942017736E-15, 0.000000000000000000 ) ) ;
#16395 = CARTESIAN_POINT ( 'NONE',  ( 144.7287565553230309, -1.999999999999977129, -16.50000000000000355 ) ) ;
#16396 = CARTESIAN_POINT ( 'NONE',  ( 9.913797604922770290, 16.41941541294738727, -16.50570979788118464 ) ) ;
#16397 = CARTESIAN_POINT ( 'NONE',  ( 26.04927874075684713, 0.2391533594452614209, -17.67486400872287788 ) ) ;
#16398 = CARTESIAN_POINT ( 'NONE',  ( 21.30888034401541731, -0.8953576338359930942, -14.03585182699830369 ) ) ;
#16400 = VERTEX_POINT ( 'NONE', #17508 ) ;
#16399 = CARTESIAN_POINT ( 'NONE',  ( 31.92618181579182135, -10.29178896789921893, -18.33933693937521880 ) ) ;
#16401 = CARTESIAN_POINT ( 'NONE',  ( 12.51757296969303290, 8.578467993704791184, -15.11616904564172792 ) ) ;
#16402 = CIRCLE ( 'NONE', #16883, 8.000000000000000000 ) ;
#16403 = CARTESIAN_POINT ( 'NONE',  ( 2.407616245347821593, -5.000000000000016875, 7.409880882142680036 ) ) ;
#16404 = CARTESIAN_POINT ( 'NONE',  ( 152.0152310637604955, -10.00000000000000178, 1.702185954127501066 ) ) ;
#16406 = EDGE_LOOP ( 'NONE', ( #20263, #5202 ) ) ;
#16405 = CARTESIAN_POINT ( 'NONE',  ( 149.5152310637605524, -10.00000000000000178, -11.28819510263909542 ) ) ;
#16407 = VERTEX_POINT ( 'NONE', #10336 ) ;
#16408 = CARTESIAN_POINT ( 'NONE',  ( 129.5152310637605808, -10.00000000000000888, -19.94844914048349338 ) ) ;
#16409 = CARTESIAN_POINT ( 'NONE',  ( 10.33931768503335924, 18.38068274058360885, -17.76381606660089929 ) ) ;
#16410 = EDGE_CURVE ( 'NONE', #16190, #11956, #1356, .T. ) ;
#16411 = VERTEX_POINT ( 'NONE', #29011 ) ;
#16412 = VECTOR ( 'NONE', #3998, 1000.000000000000000 ) ;
#16413 = CARTESIAN_POINT ( 'NONE',  ( -24.99999999999998934, 60.00000000000000711, 29.99999999999999289 ) ) ;
#16414 = FACE_OUTER_BOUND ( 'NONE', #17885, .T. ) ;
#16415 = EDGE_CURVE ( 'NONE', #17928, #14061, #5992, .T. ) ;
#16416 = VECTOR ( 'NONE', #20590, 1000.000000000000000 ) ;
#16417 = CARTESIAN_POINT ( 'NONE',  ( 17.95327243003904982, 7.812726124483462264, -14.88485059575767266 ) ) ;
#16418 = CARTESIAN_POINT ( 'NONE',  ( 15.41555982967951444, 8.269517134526982005, -21.14450021912286104 ) ) ;
#16419 = EDGE_LOOP ( 'NONE', ( #14676, #11478 ) ) ;
#16420 = CARTESIAN_POINT ( 'NONE',  ( 35.21546461977369091, -21.68794239832507742, -20.90642333977985956 ) ) ;
#16421 = VECTOR ( 'NONE', #7986, 1000.000000000000000 ) ;
#16422 = CARTESIAN_POINT ( 'NONE',  ( 20.47999367081501632, -2.041782396245861442, -15.93780510180117638 ) ) ;
#16423 = CARTESIAN_POINT ( 'NONE',  ( 21.74214448781610542, 1.960522507982400020, -19.23370281053773923 ) ) ;
#16424 = ORIENTED_EDGE ( 'NONE', *, *, #823, .T. ) ;
#16425 = CARTESIAN_POINT ( 'NONE',  ( 27.29378187812181267, -6.326311925282933402, -12.73600023524891967 ) ) ;
#16426 = AXIS2_PLACEMENT_3D ( 'NONE', #16367, #9647, #4776 ) ;
#16427 = ORIENTED_EDGE ( 'NONE', *, *, #14201, .T. ) ;
#16428 = DIRECTION ( 'NONE',  ( 0.3090169943749475623, 8.338696094058001131E-17, 0.9510565162951536422 ) ) ;
#16429 = AXIS2_PLACEMENT_3D ( 'NONE', #18594, #23630, #25325 ) ;
#16430 = ORIENTED_EDGE ( 'NONE', *, *, #24105, .T. ) ;
#16431 = DIRECTION ( 'NONE',  ( -0.8090169943749474513, -2.183098979609982436E-16, -0.5877852522924731371 ) ) ;
#16432 = CARTESIAN_POINT ( 'NONE',  ( 171.1922820468852819, -9.999999999999996447, -4.936203717676158398 ) ) ;
#16433 = CARTESIAN_POINT ( 'NONE',  ( 34.64580997985590471, -12.63631557036062247, -18.97247631304233195 ) ) ;
#16434 = CARTESIAN_POINT ( 'NONE',  ( 17.10490717348788081, 9.547663288818908356, -11.45998271326893381 ) ) ;
#16435 = ORIENTED_EDGE ( 'NONE', *, *, #16410, .F. ) ;
#16436 = FACE_OUTER_BOUND ( 'NONE', #24238, .T. ) ;
#16437 = CARTESIAN_POINT ( 'NONE',  ( 130.7287565553229456, -9.999999999999982236, 3.500000000000003109 ) ) ;
#16438 = CARTESIAN_POINT ( 'NONE',  ( 10.47224519147693478, 16.45115926513079074, -17.33471155705291977 ) ) ;
#16439 = LINE ( 'NONE', #9411, #11175 ) ;
#16440 = FACE_BOUND ( 'NONE', #21845, .T. ) ;
#16441 = ADVANCED_FACE ( 'NONE', ( #10187 ), #15057, .T. ) ;
#16442 = EDGE_CURVE ( 'NONE', #29543, #14718, #29425, .T. ) ;
#16443 = ORIENTED_EDGE ( 'NONE', *, *, #11755, .T. ) ;
#16444 = FACE_OUTER_BOUND ( 'NONE', #18391, .T. ) ;
#16445 = EDGE_CURVE ( 'NONE', #15239, #2318, #8198, .T. ) ;
#16446 = VECTOR ( 'NONE', #24670, 1000.000000000000000 ) ;
#16447 = DIRECTION ( 'NONE',  ( 1.000000000000000000, 0.000000000000000000, 0.000000000000000000 ) ) ;
#16448 = EDGE_CURVE ( 'NONE', #29689, #27920, #15215, .T. ) ;
#16449 = DIRECTION ( 'NONE',  ( 0.000000000000000000, 0.000000000000000000, 1.000000000000000000 ) ) ;
#16450 = ORIENTED_EDGE ( 'NONE', *, *, #9968, .F. ) ;
#16451 = CARTESIAN_POINT ( 'NONE',  ( 9.668885350391278166, 16.22271324469333109, -17.88465541571617834 ) ) ;
#16452 = CIRCLE ( 'NONE', #21815, 13.00000000000000178 ) ;
#16453 = CARTESIAN_POINT ( 'NONE',  ( 23.59197141788265384, -6.183129490800155281, -14.78464116683282015 ) ) ;
#16454 = CARTESIAN_POINT ( 'NONE',  ( 20.29352232415978463, 1.537418251635638944, -14.27211978419980021 ) ) ;
#16455 = DIRECTION ( 'NONE',  ( -1.000000000000000000, 0.000000000000000000, 0.000000000000000000 ) ) ;
#16456 = DIRECTION ( 'NONE',  ( -0.5000000000000015543, 0.8660254037844378194, 0.000000000000000000 ) ) ;
#16457 = CARTESIAN_POINT ( 'NONE',  ( -7.347286611336976136, -4.995646404165301036, -0.4969600502617637638 ) ) ;
#16458 = CARTESIAN_POINT ( 'NONE',  ( 23.21730923944814506, -4.364887171357101359, -13.63095412955673247 ) ) ;
#16459 = PLANE ( 'NONE',  #24013 ) ;
#16460 = CARTESIAN_POINT ( 'NONE',  ( 0.000000000000000000, 0.000000000000000000, -18.00000000000000000 ) ) ;
#16461 = VECTOR ( 'NONE', #25644, 1000.000000000000000 ) ;
#16462 = CARTESIAN_POINT ( 'NONE',  ( 177.2287565553229172, -1.999999999999968026, -29.49038105676660493 ) ) ;
#16463 = CARTESIAN_POINT ( 'NONE',  ( -20.00000000000017053, 34.64101615137744972, -10.00000000000000000 ) ) ;
#16464 = CARTESIAN_POINT ( 'NONE',  ( 10.47452605456472696, 16.44069893626776491, -17.33376834041267145 ) ) ;
#16465 = CARTESIAN_POINT ( 'NONE',  ( 35.54287943964028784, -22.15884374752674546, -18.65915260879160797 ) ) ;
#16466 = CARTESIAN_POINT ( 'NONE',  ( 32.62126879184269512, -11.04717877266006987, -18.30218954475424908 ) ) ;
#16467 = VECTOR ( 'NONE', #23179, 1000.000000000000000 ) ;
#16468 = ORIENTED_EDGE ( 'NONE', *, *, #6826, .T. ) ;
#16469 = CARTESIAN_POINT ( 'NONE',  ( 8.944584683310379702, 16.95159276115599667, -17.93331994345748726 ) ) ;
#16470 = ORIENTED_EDGE ( 'NONE', *, *, #25580, .F. ) ;
#16471 = LINE ( 'NONE', #7329, #16320 ) ;
#16472 = CARTESIAN_POINT ( 'NONE',  ( 19.23836061553175369, 5.151828676608854352, -13.99136221198299168 ) ) ;
#16473 = CARTESIAN_POINT ( 'NONE',  ( 11.05545861061968083, 17.68922483874021978, -17.89384690447096560 ) ) ;
#16474 = CARTESIAN_POINT ( 'NONE',  ( 149.5152310637605524, -1.999999999999976241, -11.28819510263909542 ) ) ;
#16475 = ORIENTED_EDGE ( 'NONE', *, *, #28801, .F. ) ;
#16476 = VECTOR ( 'NONE', #25792, 1000.000000000000000 ) ;
#16477 = ORIENTED_EDGE ( 'NONE', *, *, #25146, .T. ) ;
#16478 = CARTESIAN_POINT ( 'NONE',  ( 9.826288910175632552, 16.82074144182198694, -16.60662094963572244 ) ) ;
#16479 = CARTESIAN_POINT ( 'NONE',  ( 144.5152310637606092, -10.00000000000000178, -19.94844914048349693 ) ) ;
#16480 = EDGE_CURVE ( 'NONE', #18591, #8784, #28708, .T. ) ;
#16481 = CARTESIAN_POINT ( 'NONE',  ( 10.07879545831710999, 15.66271422494645904, -16.43741374977755143 ) ) ;
#16482 = DIRECTION ( 'NONE',  ( 0.3090169943749472292, 8.338696094057992503E-17, -0.9510565162951536422 ) ) ;
#16483 = PLANE ( 'NONE',  #7677 ) ;
#16484 = EDGE_CURVE ( 'NONE', #16977, #8387, #25297, .T. ) ;
#16485 = EDGE_LOOP ( 'NONE', ( #2355, #17969, #9802, #21534 ) ) ;
#16486 = FACE_OUTER_BOUND ( 'NONE', #166, .T. ) ;
#16487 = ORIENTED_EDGE ( 'NONE', *, *, #23729, .F. ) ;
#16488 = CARTESIAN_POINT ( 'NONE',  ( 10.73134732381016576, 15.26288385841099249, -17.22756371135774245 ) ) ;
#16489 = CARTESIAN_POINT ( 'NONE',  ( 33.89278150306358128, -11.43586942258664507, -20.72336631513872973 ) ) ;
#16490 = CARTESIAN_POINT ( 'NONE',  ( 29.90031526554274777, -7.862644070287768905, -16.42500436498598049 ) ) ;
#16491 = CARTESIAN_POINT ( 'NONE',  ( 29.30346499805017757, -7.722527705200430859, -14.56292402596598556 ) ) ;
#16492 = ORIENTED_EDGE ( 'NONE', *, *, #4323, .F. ) ;
#16493 = ORIENTED_EDGE ( 'NONE', *, *, #18555, .F. ) ;
#16494 = VECTOR ( 'NONE', #5648, 1000.000000000000000 ) ;
#16495 = DIRECTION ( 'NONE',  ( 0.9510565162951536422, 0.000000000000000000, -0.3090169943749475623 ) ) ;
#16496 = FACE_OUTER_BOUND ( 'NONE', #9753, .T. ) ;
#16497 = CARTESIAN_POINT ( 'NONE',  ( 29.95311431238071975, -11.57681909846818691, -12.96816900313696230 ) ) ;
#16498 = CIRCLE ( 'NONE', #3355, 8.000000000000007105 ) ;
#16499 = CARTESIAN_POINT ( 'NONE',  ( 28.32023557703361405, -7.180604414193060059, -17.61256657898508138 ) ) ;
#16500 = VECTOR ( 'NONE', #29703, 1000.000000000000000 ) ;
#16501 = VERTEX_POINT ( 'NONE', #10799 ) ;
#16502 = FACE_OUTER_BOUND ( 'NONE', #10198, .T. ) ;
#16503 = AXIS2_PLACEMENT_3D ( 'NONE', #25942, #18232, #8916 ) ;
#16504 = ORIENTED_EDGE ( 'NONE', *, *, #24814, .T. ) ;
#16505 = FACE_OUTER_BOUND ( 'NONE', #6663, .T. ) ;
#16506 = DIRECTION ( 'NONE',  ( -0.000000000000000000, -0.000000000000000000, -1.000000000000000000 ) ) ;
#16507 = LINE ( 'NONE', #3101, #22170 ) ;
#16508 = UNCERTAINTY_MEASURE_WITH_UNIT (LENGTH_MEASURE( 1.000000000000000082E-05 ), #14232, 'distance_accuracy_value', 'NONE');
#16509 = CARTESIAN_POINT ( 'NONE',  ( 10.72487265201256434, 16.61247851518984575, -15.95251179903439542 ) ) ;
#16510 = DIRECTION ( 'NONE',  ( 0.5877852522924731371, 1.586114251531760728E-16, 0.8090169943749474513 ) ) ;
#16511 = ORIENTED_EDGE ( 'NONE', *, *, #4741, .F. ) ;
#16512 = VECTOR ( 'NONE', #25075, 1000.000000000000000 ) ;
#16513 = DIRECTION ( 'NONE',  ( -2.698458740408365879E-16, 1.000000000000000000, 0.000000000000000000 ) ) ;
#16514 = VERTEX_POINT ( 'NONE', #25006 ) ;
#16515 = CARTESIAN_POINT ( 'NONE',  ( 11.47181023233108021, 9.274170903235749108, -15.86135313853478657 ) ) ;
#16516 = ORIENTED_EDGE ( 'NONE', *, *, #11031, .F. ) ;
#16517 = EDGE_CURVE ( 'NONE', #25397, #9138, #6226, .T. ) ;
#16518 = EDGE_CURVE ( 'NONE', #6555, #30249, #20550, .T. ) ;
#16519 = CARTESIAN_POINT ( 'NONE',  ( 10.31625730718771017, 13.25378293009361563, -17.61694433892753153 ) ) ;
#16520 = CARTESIAN_POINT ( 'NONE',  ( 20.64663396976543552, 5.620433075351431995, -17.27584747705915902 ) ) ;
#16521 = DIRECTION ( 'NONE',  ( -2.698458740408365879E-16, 1.000000000000000000, 0.000000000000000000 ) ) ;
#16522 = CARTESIAN_POINT ( 'NONE',  ( 157.0152310637605240, -4.999999999999975131, -26.04193191628311155 ) ) ;
#16523 = EDGE_CURVE ( 'NONE', #25751, #18805, #27166, .T. ) ;
#16524 = VERTEX_POINT ( 'NONE', #1813 ) ;
#16525 = CARTESIAN_POINT ( 'NONE',  ( 29.82081855766934453, -7.722587238354316597, -15.76009366473342332 ) ) ;
#16526 = VECTOR ( 'NONE', #2998, 1000.000000000000000 ) ;
#16527 = ORIENTED_EDGE ( 'NONE', *, *, #17916, .F. ) ;
#16528 = DIRECTION ( 'NONE',  ( 0.000000000000000000, 0.4999999999999993339, -0.8660254037844390407 ) ) ;
#16529 = EDGE_CURVE ( 'NONE', #19537, #18724, #27473, .T. ) ;
#16530 = CARTESIAN_POINT ( 'NONE',  ( 11.27674754065650653, 16.67436559781366157, -16.78429523206404994 ) ) ;
#16531 = ORIENTED_EDGE ( 'NONE', *, *, #28393, .F. ) ;
#16532 = CARTESIAN_POINT ( 'NONE',  ( 33.47764622482974062, -12.08535443106849883, -18.57070694247861553 ) ) ;
#16533 = DIRECTION ( 'NONE',  ( 0.000000000000000000, -1.000000000000000000, 0.000000000000000000 ) ) ;
#16534 = LINE ( 'NONE', #66, #870 ) ;
#16535 = CARTESIAN_POINT ( 'NONE',  ( 27.46460276834485370, -5.912627539431687396, -19.42860466253708296 ) ) ;
#16536 = ORIENTED_EDGE ( 'NONE', *, *, #16480, .F. ) ;
#16537 = FACE_OUTER_BOUND ( 'NONE', #2844, .T. ) ;
#16538 =( LENGTH_UNIT ( ) NAMED_UNIT ( * ) SI_UNIT ( .MILLI., .METRE. ) );
#16539 = CARTESIAN_POINT ( 'NONE',  ( 16.12927480167980576, 2.990883400875756326, -18.25071113400840517 ) ) ;
#16540 = CARTESIAN_POINT ( 'NONE',  ( 17.51631511252498186, 5.448942031446791567, -19.07752241466814880 ) ) ;
#16541 = ORIENTED_EDGE ( 'NONE', *, *, #4274, .F. ) ;
#16542 = ORIENTED_EDGE ( 'NONE', *, *, #12623, .F. ) ;
#16543 = ORIENTED_EDGE ( 'NONE', *, *, #20161, .F. ) ;
#16544 = B_SPLINE_CURVE_WITH_KNOTS ( 'NONE', 3,
 ( #2335, #11605, #20919, #18645, #27991, #15594 ),
 .UNSPECIFIED., .F., .F.,
 ( 4, 2, 4 ),
 ( 0.006456566858647419180, 0.007625406818786685526, 0.008794246778925951871 ),
 .UNSPECIFIED. ) ;
#16545 = LINE ( 'NONE', #18988, #3527 ) ;
#16546 = VECTOR ( 'NONE', #23230, 1000.000000000000000 ) ;
#16547 = LINE ( 'NONE', #26175, #23571 ) ;
#16548 = CIRCLE ( 'NONE', #3397, 4.756499999999999950 ) ;
#16549 = EDGE_CURVE ( 'NONE', #29920, #29503, #1662, .T. ) ;
#16550 = FACE_OUTER_BOUND ( 'NONE', #26306, .T. ) ;
#16551 = CARTESIAN_POINT ( 'NONE',  ( 120.0000000000000000, -19.99999999999999645, -17.99999999999998934 ) ) ;
#16552 = PLANE ( 'NONE',  #28030 ) ;
#16553 = CARTESIAN_POINT ( 'NONE',  ( 9.915973561396301150, 16.40943619918981256, -16.50475030878699556 ) ) ;
#16554 = CARTESIAN_POINT ( 'NONE',  ( 24.12676367385581244, 0.3224161365626431741, -13.25522683364457777 ) ) ;
#16555 = CARTESIAN_POINT ( 'NONE',  ( 24.14852421541024441, 0.2028892341458684023, -15.23052705399570428 ) ) ;
#16556 = CARTESIAN_POINT ( 'NONE',  ( 33.21739345078569272, -12.71166704379270129, -20.69560413545502797 ) ) ;
#16557 = CARTESIAN_POINT ( 'NONE',  ( 158.6922820468854241, -4.999999999999975131, -35.24709285013155835 ) ) ;
#16558 = CARTESIAN_POINT ( 'NONE',  ( 166.1922820468853104, -1.999999999999972689, -4.936203717676158398 ) ) ;
#16559 = DIRECTION ( 'NONE',  ( 0.000000000000000000, 0.000000000000000000, 1.000000000000000000 ) ) ;
#16560 = CARTESIAN_POINT ( 'NONE',  ( 172.0152310637604955, -9.999999999999994671, -24.27857615940569502 ) ) ;
#16561 = CARTESIAN_POINT ( 'NONE',  ( 16.53304876882650731, 8.555045913257369961, -19.77053526944897754 ) ) ;
#16562 = ORIENTED_EDGE ( 'NONE', *, *, #18980, .F. ) ;
#16563 = VERTEX_POINT ( 'NONE', #15970 ) ;
#16564 = CARTESIAN_POINT ( 'NONE',  ( 163.6922820468852819, -9.999999999999998224, 2.247092850131519715 ) ) ;
#16565 = EDGE_CURVE ( 'NONE', #8011, #6528, #22406, .T. ) ;
#16566 = CARTESIAN_POINT ( 'NONE',  ( 10.72487265201256434, 16.61247851518984575, -15.95251179903439542 ) ) ;
#16567 = ORIENTED_EDGE ( 'NONE', *, *, #3074, .T. ) ;
#16568 = AXIS2_PLACEMENT_3D ( 'NONE', #16142, #11547, #25165 ) ;
#16569 = CYLINDRICAL_SURFACE ( 'NONE', #6155, 8.000000000000007105 ) ;
#16570 = DIRECTION ( 'NONE',  ( 1.000000000000000000, 4.440892098500622217E-16, 0.000000000000000000 ) ) ;
#16571 = ORIENTED_EDGE ( 'NONE', *, *, #15334, .T. ) ;
#16572 = CARTESIAN_POINT ( 'NONE',  ( 15.44629794785920218, 3.545610805586186132, -16.71614555938632307 ) ) ;
#16573 = CARTESIAN_POINT ( 'NONE',  ( 16.69609108537820674, 9.478167028156011753, -20.90851310094495474 ) ) ;
#16574 = ORIENTED_EDGE ( 'NONE', *, *, #11576, .T. ) ;
#16575 = CARTESIAN_POINT ( 'NONE',  ( 32.68951927270060764, -11.07419627511998605, -18.48540492261787449 ) ) ;
#16576 = CARTESIAN_POINT ( 'NONE',  ( 24.04487210496366245, -0.6674514567044148583, -16.01806975046538284 ) ) ;
#16577 = CARTESIAN_POINT ( 'NONE',  ( 20.63695664501197413, 4.642632487595073520, -17.05591670970450124 ) ) ;
#16578 = EDGE_LOOP ( 'NONE', ( #4851, #15299, #5978, #4076 ) ) ;
#16579 = CARTESIAN_POINT ( 'NONE',  ( 29.92318863513849436, -9.020257460645494163, -14.67793329163371574 ) ) ;
#16580 = VECTOR ( 'NONE', #19253, 1000.000000000000000 ) ;
#16581 = ORIENTED_EDGE ( 'NONE', *, *, #26747, .T. ) ;
#16582 = LINE ( 'NONE', #2570, #16216 ) ;
#16583 = ADVANCED_FACE ( 'NONE', ( #22709 ), #15672, .F. ) ;
#16585 = ORIENTED_EDGE ( 'NONE', *, *, #18689, .T. ) ;
#16584 = DIRECTION ( 'NONE',  ( 0.9510565162951535312, 2.566386769018988816E-16, -0.3090169943749475623 ) ) ;
#16586 = VECTOR ( 'NONE', #13346, 999.9999999999998863 ) ;
#16587 = CARTESIAN_POINT ( 'NONE',  ( 23.16277852942019067, -5.000000000000011546, -71.28770215523300635 ) ) ;
#16588 = LINE ( 'NONE', #16884, #15094 ) ;
#16589 = CARTESIAN_POINT ( 'NONE',  ( 35.71575670127456448, -17.44301942315582110, -19.29589553906783905 ) ) ;
#16590 = CARTESIAN_POINT ( 'NONE',  ( 12.75568354342045119, 7.625663700289499580, -14.92639070443840588 ) ) ;
#16591 = EDGE_LOOP ( 'NONE', ( #17057, #13540, #9076 ) ) ;
#16592 = DIRECTION ( 'NONE',  ( -0.000000000000000000, -0.000000000000000000, -1.000000000000000000 ) ) ;
#16593 = LINE ( 'NONE', #718, #9004 ) ;
#16594 = CARTESIAN_POINT ( 'NONE',  ( 12.03623766312057519, 9.280706639558555793, -16.68777662621714342 ) ) ;
#16595 = LINE ( 'NONE', #12308, #26837 ) ;
#16596 = PLANE ( 'NONE',  #14391 ) ;
#16597 = AXIS2_PLACEMENT_3D ( 'NONE', #14595, #11860, #2585 ) ;
#16598 = ORIENTED_EDGE ( 'NONE', *, *, #28841, .F. ) ;
#16599 = ORIENTED_EDGE ( 'NONE', *, *, #6819, .T. ) ;
#16600 = VECTOR ( 'NONE', #23207, 999.9999999999998863 ) ;
#16601 = DIRECTION ( 'NONE',  ( -0.8090169943749474513, -2.183098979609982436E-16, 0.5877852522924731371 ) ) ;
#16602 = CARTESIAN_POINT ( 'NONE',  ( 10.00000000000008527, 17.32050807568872486, -30.00000000000000711 ) ) ;
#16603 = ORIENTED_EDGE ( 'NONE', *, *, #14134, .F. ) ;
#16604 = CARTESIAN_POINT ( 'NONE',  ( 74.18800000000001660, -1.387778780781445676E-16, 5.000000000000000888 ) ) ;
#16605 = ORIENTED_EDGE ( 'NONE', *, *, #20276, .T. ) ;
#16606 = CARTESIAN_POINT ( 'NONE',  ( 9.662623034719734605, 16.25143302262299372, -17.90105808085208849 ) ) ;
#16607 = VECTOR ( 'NONE', #28877, 1000.000000000000000 ) ;
#16608 = CARTESIAN_POINT ( 'NONE',  ( 27.58270427615865472, -5.135490454175970498, -17.42064064436273085 ) ) ;
#16609 = CARTESIAN_POINT ( 'NONE',  ( 23.39789874936200320, -0.01207823811560896493, -14.43595595811700782 ) ) ;
#16610 = CARTESIAN_POINT ( 'NONE',  ( 97.54326518300754856, -4.999999999999991118, 70.86933047595960034 ) ) ;
#16611 = CARTESIAN_POINT ( 'NONE',  ( 2.500000000000000444, -1.178949249685215417, 2.042000000000002036 ) ) ;
#16612 = CARTESIAN_POINT ( 'NONE',  ( 7.419037233917861407, -5.000000000000015987, 22.83344875651922123 ) ) ;
#16613 = CARTESIAN_POINT ( 'NONE',  ( 28.16462234717350199, -5.661059359726887230, -16.30864077692347536 ) ) ;
#16614 = CARTESIAN_POINT ( 'NONE',  ( 146.1922820468854525, -10.00000000000000178, -22.25671179336496053 ) ) ;
#16615 = ADVANCED_FACE ( 'NONE', ( #20107 ), #11095, .F. ) ;
#16616 = DIRECTION ( 'NONE',  ( 1.000000000000000000, 0.000000000000000000, 0.000000000000000000 ) ) ;
#16617 = ADVANCED_FACE ( 'NONE', ( #30079 ), #18110, .T. ) ;
#16618 = DIRECTION ( 'NONE',  ( 2.908569913943826047E-16, -1.000000000000000000, 6.826925868028107924E-18 ) ) ;
#16619 = EDGE_CURVE ( 'NONE', #14364, #10452, #15816, .T. ) ;
#16620 = CARTESIAN_POINT ( 'NONE',  ( -5.000000000000000000, 0.000000000000000000, -18.00000000000000000 ) ) ;
#16621 = DIRECTION ( 'NONE',  ( -2.698458740408365879E-16, 1.000000000000000000, 0.000000000000000000 ) ) ;
#16622 = CARTESIAN_POINT ( 'NONE',  ( 10.47195275365909595, 16.45250042224058618, -17.33483252618548676 ) ) ;
#16623 = PLANE ( 'NONE',  #16503 ) ;
#16624 = CARTESIAN_POINT ( 'NONE',  ( 33.75544676243647757, -14.12885555826641593, -19.81592319558764004 ) ) ;
#16625 = ORIENTED_EDGE ( 'NONE', *, *, #2896, .T. ) ;
#16626 = CARTESIAN_POINT ( 'NONE',  ( 8.944584683310379702, 16.95159276115599667, -17.91928203681695564 ) ) ;
#16627 = VERTEX_POINT ( 'NONE', #22859 ) ;
#16628 = LINE ( 'NONE', #19209, #22187 ) ;
#16629 = CARTESIAN_POINT ( 'NONE',  ( 18.50902107916489570, 2.085137940960992697, -20.06823964296112450 ) ) ;
#16630 = CARTESIAN_POINT ( 'NONE',  ( 11.28016675873817576, 16.65868462784220227, -16.78288126510920719 ) ) ;
#16631 = DIRECTION ( 'NONE',  ( -1.000000000000000000, -2.908569913943825554E-16, 0.000000000000000000 ) ) ;
#16632 = ORIENTED_EDGE ( 'NONE', *, *, #15931, .T. ) ;
#16633 = EDGE_LOOP ( 'NONE', ( #6732, #19267 ) ) ;
#16634 = VERTEX_POINT ( 'NONE', #6676 ) ;
#16635 = ORIENTED_EDGE ( 'NONE', *, *, #16267, .T. ) ;
#16636 = CARTESIAN_POINT ( 'NONE',  ( 9.843778300897430000, 16.74053286659246709, -16.57516421589427225 ) ) ;
#16637 = CARTESIAN_POINT ( 'NONE',  ( 21.09505124120717667, -5.000000000000011546, -64.92389192093176575 ) ) ;
#16638 = CARTESIAN_POINT ( 'NONE',  ( 9.912057827679275235, 16.42739425315605928, -16.50652470164456531 ) ) ;
#16639 = CARTESIAN_POINT ( 'NONE',  ( 152.0152310637605524, -1.999999999999974909, -26.04193191628311155 ) ) ;
#16640 = ORIENTED_EDGE ( 'NONE', *, *, #3444, .T. ) ;
#16641 = CARTESIAN_POINT ( 'NONE',  ( 148.6922820468854241, -1.999999999999976685, -17.92658477444275889 ) ) ;
#16642 = ORIENTED_EDGE ( 'NONE', *, *, #15294, .F. ) ;
#16643 = CARTESIAN_POINT ( 'NONE',  ( 10.47705880869930084, 16.42908340295556258, -17.33272095748315422 ) ) ;
#16644 = VECTOR ( 'NONE', #30057, 1000.000000000000000 ) ;
#16645 = ORIENTED_EDGE ( 'NONE', *, *, #27323, .F. ) ;
#16647 = AXIS2_PLACEMENT_3D ( 'NONE', #4556, #6408, #8823 ) ;
#16646 = CARTESIAN_POINT ( 'NONE',  ( 36.54859390953724585, -22.18451583373416014, -16.11276402859391865 ) ) ;
#16648 = CARTESIAN_POINT ( 'NONE',  ( 27.01132674553606350, -11.00696853675122711, -18.49859303458091730 ) ) ;
#16649 = CARTESIAN_POINT ( 'NONE',  ( 15.95367323521391256, 9.281262803959288377, -20.14168370736028280 ) ) ;
#16650 = EDGE_LOOP ( 'NONE', ( #15320, #16386, #29603, #28835 ) ) ;
#16651 = CARTESIAN_POINT ( 'NONE',  ( 166.1922820468853672, -9.999999999999998224, -19.40354224447947828 ) ) ;
#16652 = VERTEX_POINT ( 'NONE', #17804 ) ;
#16653 = CARTESIAN_POINT ( 'NONE',  ( 32.33411138940433460, -10.22844123512284575, -15.25869122620317953 ) ) ;
#16654 = CARTESIAN_POINT ( 'NONE',  ( 15.11341857612343809, 8.679638894638937785, -13.66094189273949056 ) ) ;
#16655 = CARTESIAN_POINT ( 'NONE',  ( 16.77165338796101324, 10.12286561294300569, -15.51291369241808304 ) ) ;
#16656 = ORIENTED_EDGE ( 'NONE', *, *, #14988, .T. ) ;
#16657 = FACE_BOUND ( 'NONE', #19907, .T. ) ;
#16658 = EDGE_CURVE ( 'NONE', #15913, #12566, #1961, .T. ) ;
#16659 = EDGE_CURVE ( 'NONE', #15488, #15781, #23453, .T. ) ;
#16660 = ADVANCED_FACE ( 'NONE', ( #3791 ), #20248, .F. ) ;
#16661 = DIRECTION ( 'NONE',  ( 0.000000000000000000, 0.000000000000000000, 1.000000000000000000 ) ) ;
#16662 = VECTOR ( 'NONE', #9033, 1000.000000000000000 ) ;
#16663 = DIRECTION ( 'NONE',  ( 0.000000000000000000, 0.000000000000000000, 1.000000000000000000 ) ) ;
#16664 = CARTESIAN_POINT ( 'NONE',  ( 152.0152310637604955, -1.999999999999976241, 1.702185954127501066 ) ) ;
#16665 = LINE ( 'NONE', #4914, #27572 ) ;
#16666 = CARTESIAN_POINT ( 'NONE',  ( 10.33819201225523621, 18.38584521943398187, -17.87775236254758227 ) ) ;
#16667 = LINE ( 'NONE', #7510, #4127 ) ;
#16668 = ORIENTED_EDGE ( 'NONE', *, *, #5713, .F. ) ;
#16669 = DIRECTION ( 'NONE',  ( -0.9510565162951536422, -2.566386769018988816E-16, -0.3090169943749472292 ) ) ;
#16670 = ORIENTED_EDGE ( 'NONE', *, *, #7774, .F. ) ;
#16671 = CARTESIAN_POINT ( 'NONE',  ( 9.997747326010761881, 16.03441129093729245, -16.47093000352221637 ) ) ;
#16672 = EDGE_LOOP ( 'NONE', ( #168, #6972, #4082, #16037, #24590 ) ) ;
#16673 = CARTESIAN_POINT ( 'NONE',  ( 9.667859086210386366, 16.22741982304516739, -17.88507982571460531 ) ) ;
#16674 = CARTESIAN_POINT ( 'NONE',  ( 20.19814137509539975, 5.716210941879356078, -15.87681946797394517 ) ) ;
#16675 = LINE ( 'NONE', #28468, #28832 ) ;
#16676 = FILL_AREA_STYLE_COLOUR ( '', #9599 ) ;
#16677 = CARTESIAN_POINT ( 'NONE',  ( 29.88803641097454999, -7.968445601786871002, -16.75847372370488131 ) ) ;
#16678 = ORIENTED_EDGE ( 'NONE', *, *, #23597, .T. ) ;
#16679 = DIRECTION ( 'NONE',  ( 0.9510565162951535312, 2.566386769018988816E-16, -0.3090169943749475623 ) ) ;
#16680 = CARTESIAN_POINT ( 'NONE',  ( 11.25757798850943381, 16.76227960750979307, -16.79548539596511247 ) ) ;
#16681 = ORIENTED_EDGE ( 'NONE', *, *, #5500, .F. ) ;
#16682 = CARTESIAN_POINT ( 'NONE',  ( 33.51257387524950815, -12.16639167148776224, -18.62538556556795655 ) ) ;
#16683 = CARTESIAN_POINT ( 'NONE',  ( 14.03850921439652311, 8.975161913830900673, -15.18271992443145635 ) ) ;
#16684 = CARTESIAN_POINT ( 'NONE',  ( 142.0152310637606092, -10.00000000000000355, -32.93883019725009120 ) ) ;
#16685 = VECTOR ( 'NONE', #22742, 1000.000000000000000 ) ;
#16686 = CARTESIAN_POINT ( 'NONE',  ( 9.371932165391852365, 14.99172273419688750, -16.94745289082924344 ) ) ;
#16687 = CARTESIAN_POINT ( 'NONE',  ( 31.26470888135608206, -7.466309307788507432, -16.51192723299172727 ) ) ;
#16688 = EDGE_LOOP ( 'NONE', ( #15998, #16180, #17158, #23564 ) ) ;
#16689 = LINE ( 'NONE', #23565, #19818 ) ;
#16690 = EDGE_CURVE ( 'NONE', #12383, #16269, #29635, .T. ) ;
#16691 =( NAMED_UNIT ( * ) PLANE_ANGLE_UNIT ( ) SI_UNIT ( $, .RADIAN. ) );
#16692 = CARTESIAN_POINT ( 'NONE',  ( 16.54288150113237066, 3.399532473721276649, -19.15960874834559746 ) ) ;
#16693 = CARTESIAN_POINT ( 'NONE',  ( 17.31141255128542511, 8.026854538702009378, -19.31233526832781777 ) ) ;
#16694 = ORIENTED_EDGE ( 'NONE', *, *, #1552, .T. ) ;
#16695 = CARTESIAN_POINT ( 'NONE',  ( 2.500000000000000444, 0.000000000000000000, 0.000000000000000000 ) ) ;
#16696 = ORIENTED_EDGE ( 'NONE', *, *, #19061, .F. ) ;
#16697 = CARTESIAN_POINT ( 'NONE',  ( 134.5152310637605524, -1.999999999999980460, -21.71180489736090991 ) ) ;
#16698 = AXIS2_PLACEMENT_3D ( 'NONE', #9737, #2743, #16616 ) ;
#16699 = EDGE_CURVE ( 'NONE', #17686, #2910, #4532, .T. ) ;
#16700 = APPLICATION_CONTEXT ( 'automotive_design' ) ;
#16701 = EDGE_CURVE ( 'NONE', #28698, #209, #7685, .T. ) ;
#16702 = ADVANCED_FACE ( 'NONE', ( #672 ), #10115, .T. ) ;
#16703 = CARTESIAN_POINT ( 'NONE',  ( 175.7287565553229456, -9.999999999999971578, -33.50000000000000000 ) ) ;
#16704 = EDGE_CURVE ( 'NONE', #5689, #1554, #21423, .T. ) ;
#16705 = FACE_OUTER_BOUND ( 'NONE', #17317, .T. ) ;
#16706 = CARTESIAN_POINT ( 'NONE',  ( 157.0152310637605240, -9.999999999999998224, -26.04193191628311155 ) ) ;
#16707 = DIRECTION ( 'NONE',  ( 0.000000000000000000, 0.000000000000000000, -1.000000000000000000 ) ) ;
#16708 = AXIS2_PLACEMENT_3D ( 'NONE', #5402, #28631, #2823 ) ;
#16709 = CARTESIAN_POINT ( 'NONE',  ( 9.641354186875979337, 17.66887565656821124, -17.90893343548146177 ) ) ;
#16710 = CARTESIAN_POINT ( 'NONE',  ( 27.81650010061016332, -6.490163795910067535, -14.16582606047713178 ) ) ;
#16711 = CARTESIAN_POINT ( 'NONE',  ( 20.86695504291294156, -3.984745147917406971, -17.88565525751875995 ) ) ;
#16713 = ORIENTED_EDGE ( 'NONE', *, *, #24489, .T. ) ;
#16712 = CARTESIAN_POINT ( 'NONE',  ( 33.13932541451587355, -12.36573032794433047, -20.66922553108291538 ) ) ;
#16714 = CARTESIAN_POINT ( 'NONE',  ( 49.00000000000000000, 0.000000000000000000, 0.000000000000000000 ) ) ;
#16715 = FACE_OUTER_BOUND ( 'NONE', #4654, .T. ) ;
#16716 = DIRECTION ( 'NONE',  ( -0.5877852522924731371, -1.586114251531760235E-16, 0.8090169943749474513 ) ) ;
#16717 = CARTESIAN_POINT ( 'NONE',  ( 2.339468227445709925, 3.268109542640638576, -2.450000000000006395 ) ) ;
#16718 = CARTESIAN_POINT ( 'NONE',  ( 14.57776618122778700, 6.338444840345393239, -15.85465340776532095 ) ) ;
#16719 = ORIENTED_EDGE ( 'NONE', *, *, #30194, .T. ) ;
#16720 = CARTESIAN_POINT ( 'NONE',  ( 82.33896265977239182, -4.999999999999994671, 59.82275808417004015 ) ) ;
#16721 = CARTESIAN_POINT ( 'NONE',  ( 10.72074420406304895, 16.63141210374104872, -15.95421917676928025 ) ) ;
#16722 = DIRECTION ( 'NONE',  ( 0.000000000000000000, 0.000000000000000000, 1.000000000000000000 ) ) ;
#16723 = CARTESIAN_POINT ( 'NONE',  ( 164.7287565553229740, -4.999999999999972466, -33.82050807568879947 ) ) ;
#16724 = CARTESIAN_POINT ( 'NONE',  ( 15.39489021548154568, 6.697694061803245447, -14.95590323207311734 ) ) ;
#16725 = CARTESIAN_POINT ( 'NONE',  ( 13.09464261414706066, 5.717622835290344874, -15.96348941799783816 ) ) ;
#16726 = ORIENTED_EDGE ( 'NONE', *, *, #29988, .T. ) ;
#16727 = CARTESIAN_POINT ( 'NONE',  ( 33.41663030065195272, -12.60673267154789201, -19.71350710734569134 ) ) ;
#16728 = EDGE_CURVE ( 'NONE', #1603, #7228, #22563, .T. ) ;
#16729 = CARTESIAN_POINT ( 'NONE',  ( 21.43024726678804726, -3.720057188146618010, -16.74626013867020902 ) ) ;
#16730 = CARTESIAN_POINT ( 'NONE',  ( 20.49785840140504689, 4.750029832917431527, -16.36601636927073145 ) ) ;
#16731 = VECTOR ( 'NONE', #23799, 1000.000000000000000 ) ;
#16732 = CARTESIAN_POINT ( 'NONE',  ( 28.61400761516875590, -9.413816014945153299, -13.42719155385534080 ) ) ;
#16733 = EDGE_CURVE ( 'NONE', #11366, #9707, #28487, .T. ) ;
#16734 = ORIENTED_EDGE ( 'NONE', *, *, #23958, .F. ) ;
#16735 = VERTEX_POINT ( 'NONE', #16121 ) ;
#16736 = EDGE_CURVE ( 'NONE', #19956, #26921, #20592, .T. ) ;
#16737 = DIRECTION ( 'NONE',  ( 0.000000000000000000, -1.000000000000000000, 0.000000000000000000 ) ) ;
#16738 = EDGE_CURVE ( 'NONE', #9954, #11059, #21714, .T. ) ;
#16739 = DIRECTION ( 'NONE',  ( -2.698458740408365879E-16, 1.000000000000000000, 0.000000000000000000 ) ) ;
#16740 = FACE_OUTER_BOUND ( 'NONE', #11664, .T. ) ;
#16741 = ORIENTED_EDGE ( 'NONE', *, *, #9965, .T. ) ;
#16742 = CARTESIAN_POINT ( 'NONE',  ( -4.000000000000001776, 2.309401076758532678, -2.092734410091829034 ) ) ;
#16743 = CARTESIAN_POINT ( 'NONE',  ( 36.54859497913844990, -21.18452063888661385, -18.28382709584098720 ) ) ;
#16744 = SHAPE_REPRESENTATION ( 'Ergonomic Serrated Toe Peg', ( #13190 ), #7783 ) ;
#16745 = CARTESIAN_POINT ( 'NONE',  ( 14.64119204185053391, 8.458903494591371697, -13.42360716063767967 ) ) ;
#16746 = AXIS2_PLACEMENT_3D ( 'NONE', #11498, #25264, #11356 ) ;
#16747 = LINE ( 'NONE', #2578, #26359 ) ;
#16748 = LINE ( 'NONE', #582, #19726 ) ;
#16749 = CARTESIAN_POINT ( 'NONE',  ( 12.01190781424926435, 9.390070215761314287, -16.69800690218674788 ) ) ;
#16750 = CARTESIAN_POINT ( 'NONE',  ( 0.000000000000000000, 0.000000000000000000, 0.000000000000000000 ) ) ;
#16751 = LINE ( 'NONE', #21781, #30076 ) ;
#16752 = EDGE_LOOP ( 'NONE', ( #30219, #1154, #20916, #7430 ) ) ;
#16753 = CARTESIAN_POINT ( 'NONE',  ( 420.0000000000002274, 34.64101615137744972, 12.00000000000000178 ) ) ;
#16754 = CARTESIAN_POINT ( 'NONE',  ( 151.1922820468853956, -1.999999999999976241, -10.74328820663507678 ) ) ;
#16755 = ORIENTED_EDGE ( 'NONE', *, *, #11615, .T. ) ;
#16756 = DIRECTION ( 'NONE',  ( -2.698458740408365879E-16, 1.000000000000000000, 0.000000000000000000 ) ) ;
#16757 = ORIENTED_EDGE ( 'NONE', *, *, #9429, .F. ) ;
#16758 = CARTESIAN_POINT ( 'NONE',  ( 13.37268442792299261, 7.622911828202562745, -15.71339253741762221 ) ) ;
#16759 = EDGE_CURVE ( 'NONE', #23759, #23604, #28791, .T. ) ;
#16760 = CARTESIAN_POINT ( 'NONE',  ( 27.43603605124483025, -4.716368786860208218, -15.63773258035017300 ) ) ;
#16761 = ORIENTED_EDGE ( 'NONE', *, *, #22631, .T. ) ;
#16762 = CARTESIAN_POINT ( 'NONE',  ( 22.42023978564754927, -3.655767601918122445, -13.54521809681785172 ) ) ;
#16763 = CARTESIAN_POINT ( 'NONE',  ( 25.00000000000000000, 2.789133085058098087E-16, -2.055000000000000160 ) ) ;
#16764 = CARTESIAN_POINT ( 'NONE',  ( 0.000000000000000000, 0.000000000000000000, -15.00000000000000355 ) ) ;
#16765 = CARTESIAN_POINT ( 'NONE',  ( 166.1922820468853672, -1.999999999999971800, -22.25671179336496053 ) ) ;
#16766 = VECTOR ( 'NONE', #6878, 1000.000000000000000 ) ;
#16767 = DIRECTION ( 'NONE',  ( 0.9510565162951536422, 2.566386769018988816E-16, 0.3090169943749472292 ) ) ;
#16768 = VERTEX_POINT ( 'NONE', #24032 ) ;
#16769 = CARTESIAN_POINT ( 'NONE',  ( 8.000000000000000000, -4.618802153517025388, -5.000000000000000888 ) ) ;
#16770 = CARTESIAN_POINT ( 'NONE',  ( 171.1922820468853672, -4.999999999999970690, -28.06379628232387802 ) ) ;
#16771 = CARTESIAN_POINT ( 'NONE',  ( 176.1922820468853104, -9.999999999999994671, -19.40354224447947828 ) ) ;
#16772 = CARTESIAN_POINT ( 'NONE',  ( 22.68532101535755885, -5.000000000000011546, -69.81823902450180697 ) ) ;
#16773 = CARTESIAN_POINT ( 'NONE',  ( 11.99569818778800645, 9.464409628959467469, -16.70471015293584216 ) ) ;
#16774 = LINE ( 'NONE', #26098, #18951 ) ;
#16775 = CARTESIAN_POINT ( 'NONE',  ( 35.07504771885155037, -20.05712364337910714, -20.21480690768607857 ) ) ;
#16776 = ORIENTED_EDGE ( 'NONE', *, *, #3148, .F. ) ;
#16777 = CARTESIAN_POINT ( 'NONE',  ( 8.944584683310379702, 16.95159276115599667, -17.91796598306941135 ) ) ;
#16778 = CARTESIAN_POINT ( 'NONE',  ( 420.0000000000002274, 27.64101615137744972, 12.00000000000000178 ) ) ;
#16779 = CARTESIAN_POINT ( 'NONE',  ( 17.96884874826282186, 1.586046385177752871, -19.67104016136476119 ) ) ;
#16780 = CARTESIAN_POINT ( 'NONE',  ( 12.83225144795546235, 9.540626470039393681, -16.14103964284477399 ) ) ;
#16781 = DIRECTION ( 'NONE',  ( -1.110223024625156540E-16, 0.000000000000000000, -1.000000000000000000 ) ) ;
#16782 = ORIENTED_EDGE ( 'NONE', *, *, #2114, .F. ) ;
#16783 = CARTESIAN_POINT ( 'NONE',  ( 10.24089172292967298, 14.91932009296530559, -16.37038124228770997 ) ) ;
#16784 = CARTESIAN_POINT ( 'NONE',  ( 8.000000000000003553, 4.618802153517037823, -0.7145311798163362926 ) ) ;
#16785 = AXIS2_PLACEMENT_3D ( 'NONE', #9702, #10159, #26517 ) ;
#16786 = CARTESIAN_POINT ( 'NONE',  ( 9.913797604922770290, 16.41941541294738727, -16.50570979788118464 ) ) ;
#16787 = CARTESIAN_POINT ( 'NONE',  ( 161.1922820468853672, -1.999999999999973133, -22.25671179336496053 ) ) ;
#16788 = EDGE_LOOP ( 'NONE', ( #2607, #22027, #1431, #29374 ) ) ;
#16789 = CARTESIAN_POINT ( 'NONE',  ( 169.7287565553229172, -1.999999999999970468, -16.50000000000000355 ) ) ;
#16790 = ORIENTED_EDGE ( 'NONE', *, *, #1581, .T. ) ;
#16791 = CARTESIAN_POINT ( 'NONE',  ( 10.47224519147693478, 16.45115926513079074, -17.33471155705291977 ) ) ;
#16792 = EDGE_CURVE ( 'NONE', #5157, #29543, #12402, .T. ) ;
#16793 = VERTEX_POINT ( 'NONE', #7538 ) ;
#16794 = CARTESIAN_POINT ( 'NONE',  ( 32.85377328814971065, -9.687349299063408026, -18.71178847241494481 ) ) ;
#16795 = CARTESIAN_POINT ( 'NONE',  ( 28.06689949639850212, -8.111051215268487269, -13.49421662364394514 ) ) ;
#16796 = CARTESIAN_POINT ( 'NONE',  ( 26.87449084144840938, -11.88902188497427481, -13.49525739704605343 ) ) ;
#16797 = EDGE_CURVE ( 'NONE', #5129, #26933, #534, .T. ) ;
#16798 = PLANE ( 'NONE',  #30183 ) ;
#16799 = CARTESIAN_POINT ( 'NONE',  ( 32.46393572324419807, -10.24815885013986794, -15.62561752695271622 ) ) ;
#16800 = CARTESIAN_POINT ( 'NONE',  ( 18.95088517700565944, -0.6660330538943091128, -18.51770762617101340 ) ) ;
#16801 = CARTESIAN_POINT ( 'NONE',  ( 26.64397501440380012, -9.555891369342745634, -14.23407566704858951 ) ) ;
#16802 = FACE_BOUND ( 'NONE', #13707, .T. ) ;
#16803 = VECTOR ( 'NONE', #4763, 1000.000000000000000 ) ;
#16804 = DIRECTION ( 'NONE',  ( -1.000000000000000000, 0.000000000000000000, -0.000000000000000000 ) ) ;
#16805 = CARTESIAN_POINT ( 'NONE',  ( 46.75000000000000000, 7.511012776518212944E-16, -5.000000000000000888 ) ) ;
#16806 = LINE ( 'NONE', #28156, #1437 ) ;
#16807 = ORIENTED_EDGE ( 'NONE', *, *, #2179, .F. ) ;
#16808 = CARTESIAN_POINT ( 'NONE',  ( 10.84018844833751594, -5.000000000000015099, 33.36266952732570701 ) ) ;
#16809 = CARTESIAN_POINT ( 'NONE',  ( 12.27697253541231426, 9.494350595542041304, -15.31066389949581463 ) ) ;
#16810 = CARTESIAN_POINT ( 'NONE',  ( 63.44486372867149981, -20.00000000000000355, -17.99999999999998934 ) ) ;
#16811 = VERTEX_POINT ( 'NONE', #7835 ) ;
#16812 = CARTESIAN_POINT ( 'NONE',  ( 139.5152310637605808, -1.999999999999978684, -21.71180489736090991 ) ) ;
#16813 = ORIENTED_EDGE ( 'NONE', *, *, #5294, .F. ) ;
#16814 = CARTESIAN_POINT ( 'NONE',  ( 12.50736435846123484, 8.573956625762026107, -15.12430548898761806 ) ) ;
#16815 = ORIENTED_EDGE ( 'NONE', *, *, #3202, .F. ) ;
#16816 = CARTESIAN_POINT ( 'NONE',  ( 17.05751464226099401, 1.788256342680895949, -18.14502383782993888 ) ) ;
#16817 = CARTESIAN_POINT ( 'NONE',  ( 137.0152310637606092, -1.999999999999979572, -6.958068083716895558 ) ) ;
#16818 = CARTESIAN_POINT ( 'NONE',  ( 159.5152310637604955, -9.999999999999998224, -11.28819510263909542 ) ) ;
#16819 = ORIENTED_EDGE ( 'NONE', *, *, #270, .F. ) ;
#16821 = ORIENTED_EDGE ( 'NONE', *, *, #30194, .F. ) ;
#16820 = CARTESIAN_POINT ( 'NONE',  ( -17.25000000000017053, 34.64101615137744972, -10.00000000000000000 ) ) ;
#16822 = DIRECTION ( 'NONE',  ( -0.9510565162951536422, 0.000000000000000000, -0.3090169943749472292 ) ) ;
#16823 = CARTESIAN_POINT ( 'NONE',  ( 11.05541542350396256, 17.68942290035798237, -17.91468072056456862 ) ) ;
#16824 = EDGE_CURVE ( 'NONE', #13894, #30129, #2586, .T. ) ;
#16825 = VERTEX_POINT ( 'NONE', #23147 ) ;
#16826 = EDGE_CURVE ( 'NONE', #28576, #17347, #11530, .T. ) ;
#16827 = CARTESIAN_POINT ( 'NONE',  ( 35.54582861202835886, -21.17209281684672817, -18.49356017204852520 ) ) ;
#16828 = CARTESIAN_POINT ( 'NONE',  ( 17.18819971663578272, 0.8441372818425427749, -18.45219435416397502 ) ) ;
#16829 = EDGE_CURVE ( 'NONE', #23355, #22122, #20844, .T. ) ;
#16830 = VECTOR ( 'NONE', #3386, 1000.000000000000000 ) ;
#16831 = CARTESIAN_POINT ( 'NONE',  ( 174.5152310637603819, -9.999999999999994671, -4.391296821672111328 ) ) ;
#16832 = CARTESIAN_POINT ( 'NONE',  ( 10.02031722384195156, 12.01814620627372143, -16.67932286086919902 ) ) ;
#16833 = EDGE_CURVE ( 'NONE', #27200, #22368, #21575, .T. ) ;
#16834 = CARTESIAN_POINT ( 'NONE',  ( 31.24625831705917278, -7.622123577322120980, -17.00257116200763008 ) ) ;
#16835 = ORIENTED_EDGE ( 'NONE', *, *, #26597, .F. ) ;
#16836 = DIRECTION ( 'NONE',  ( -0.8090169943749474513, -2.183098979609982436E-16, -0.5877852522924731371 ) ) ;
#16837 = CARTESIAN_POINT ( 'NONE',  ( 19.47744964272635926, 1.166342761889149982, -14.46873920536258495 ) ) ;
#16838 = CARTESIAN_POINT ( 'NONE',  ( 17.65840769916877662, 9.384080434346836697, -15.74689851229248738 ) ) ;
#16839 = ORIENTED_EDGE ( 'NONE', *, *, #20441, .F. ) ;
#16840 = DIRECTION ( 'NONE',  ( -2.698458740408365879E-16, 1.000000000000000000, 0.000000000000000000 ) ) ;
#16841 = EDGE_LOOP ( 'NONE', ( #22676, #12055, #23926, #2069 ) ) ;
#16842 = EDGE_LOOP ( 'NONE', ( #16017, #13608, #14692, #19364 ) ) ;
#16843 = VECTOR ( 'NONE', #6657, 1000.000000000000000 ) ;
#16844 = DIRECTION ( 'NONE',  ( 0.5877852522924731371, 1.586114251531760728E-16, 0.8090169943749474513 ) ) ;
#16845 = VECTOR ( 'NONE', #1344, 1000.000000000000000 ) ;
#16846 = CARTESIAN_POINT ( 'NONE',  ( 149.5152310637605524, -1.999999999999976241, -11.28819510263909542 ) ) ;
#16847 = DIRECTION ( 'NONE',  ( -2.698458740408365879E-16, 1.000000000000000000, 0.000000000000000000 ) ) ;
#16848 = CARTESIAN_POINT ( 'NONE',  ( 175.7287565553229456, -9.999999999999971578, 3.500000000000003109 ) ) ;
#16849 = AXIS2_PLACEMENT_3D ( 'NONE', #12162, #14592, #14288 ) ;
#16850 = CARTESIAN_POINT ( 'NONE',  ( 176.1922820468852819, -9.999999999999994671, -10.74328820663507678 ) ) ;
#16851 = VECTOR ( 'NONE', #7553, 1000.000000000000000 ) ;
#16852 = CARTESIAN_POINT ( 'NONE',  ( 9.695397291186985456, 17.42102709130404747, -17.08803885907851594 ) ) ;
#16853 = CARTESIAN_POINT ( 'NONE',  ( 28.61166709039449785, -6.781025521995295513, -16.93684798036101213 ) ) ;
#16854 = CARTESIAN_POINT ( 'NONE',  ( 21.92441584138004984, 2.204866226087792924, -14.79409581392398110 ) ) ;
#16856 = ORIENTED_EDGE ( 'NONE', *, *, #25973, .F. ) ;
#16855 = CARTESIAN_POINT ( 'NONE',  ( 35.21546461977369091, -21.68794239832507742, -20.90642333977985956 ) ) ;
#16857 = LINE ( 'NONE', #26185, #20733 ) ;
#16858 = DIRECTION ( 'NONE',  ( 0.000000000000000000, 0.000000000000000000, 1.000000000000000000 ) ) ;
#16859 = DIRECTION ( 'NONE',  ( -2.698458740408365879E-16, 1.000000000000000000, -0.000000000000000000 ) ) ;
#16860 = CARTESIAN_POINT ( 'NONE',  ( -13.00000000000000178, 1.592040838891559293E-15, 15.00000000000000000 ) ) ;
#16861 = CARTESIAN_POINT ( 'NONE',  ( 19.52227536296714305, 7.868296793410291201, -18.00468392081665669 ) ) ;
#16862 = LINE ( 'NONE', #14107, #12969 ) ;
#16863 = CARTESIAN_POINT ( 'NONE',  ( 10.33813570737955700, 18.38610344077106973, -17.89676158639688452 ) ) ;
#16864 = DIRECTION ( 'NONE',  ( -1.000000000000000000, 0.000000000000000000, 0.000000000000000000 ) ) ;
#16865 = DIRECTION ( 'NONE',  ( 1.000000000000000000, 0.000000000000000000, -5.782411586589357392E-17 ) ) ;
#16866 = ADVANCED_FACE ( 'NONE', ( #7397 ), #16912, .T. ) ;
#16867 = VECTOR ( 'NONE', #6665, 1000.000000000000000 ) ;
#16868 = CARTESIAN_POINT ( 'NONE',  ( 15.93484470893836935, 6.939319753835953009, -14.67888072223970752 ) ) ;
#16869 = EDGE_CURVE ( 'NONE', #10367, #29995, #7908, .T. ) ;
#16870 = EDGE_CURVE ( 'NONE', #2694, #10208, #5779, .T. ) ;
#16871 = CARTESIAN_POINT ( 'NONE',  ( 26.36605488913174611, -12.34709378291890758, -12.75955235896099005 ) ) ;
#16872 = ORIENTED_EDGE ( 'NONE', *, *, #27045, .T. ) ;
#16873 = CARTESIAN_POINT ( 'NONE',  ( 35.24964364652129234, -20.84149066036063047, -20.16262864730545346 ) ) ;
#16874 = CARTESIAN_POINT ( 'NONE',  ( 23.66523006742493251, -0.7244823556979478330, -15.35173719993635011 ) ) ;
#16875 = CIRCLE ( 'NONE', #17342, 139.8897274573438096 ) ;
#16876 = CARTESIAN_POINT ( 'NONE',  ( 19.79871159306781436, 4.571585941193342606, -15.48227718036497080 ) ) ;
#16877 = AXIS2_PLACEMENT_3D ( 'NONE', #15002, #12721, #17159 ) ;
#16878 = CARTESIAN_POINT ( 'NONE',  ( 29.51995068812739476, -6.211492405346085377, -16.93985997890334261 ) ) ;
#16879 = ORIENTED_EDGE ( 'NONE', *, *, #7407, .T. ) ;
#16880 = CARTESIAN_POINT ( 'NONE',  ( 20.00000000000017053, 27.64101615137744972, 10.00000000000000178 ) ) ;
#16881 = CARTESIAN_POINT ( 'NONE',  ( 133.7287565553229172, -1.999999999999988010, -33.50000000000000000 ) ) ;
#16882 = CARTESIAN_POINT ( 'NONE',  ( 153.6922820468853388, -1.999999999999975353, -15.07341522555727309 ) ) ;
#16883 = AXIS2_PLACEMENT_3D ( 'NONE', #17285, #10565, #10258 ) ;
#16884 = CARTESIAN_POINT ( 'NONE',  ( 175.7287565553229456, -9.999999999999971578, 3.500000000000003109 ) ) ;
#16885 = CARTESIAN_POINT ( 'NONE',  ( 33.30032953382602301, -10.37518355935928938, -17.98954529685971337 ) ) ;
#16886 = AXIS2_PLACEMENT_3D ( 'NONE', #19258, #5078, #16822 ) ;
#16887 = CARTESIAN_POINT ( 'NONE',  ( 12.76959483864652611, 7.631811206235384226, -14.91530316759754982 ) ) ;
#16888 = VECTOR ( 'NONE', #12081, 1000.000000000000000 ) ;
#16889 = CYLINDRICAL_SURFACE ( 'NONE', #23450, 2.100000000000000977 ) ;
#16890 = CARTESIAN_POINT ( 'NONE',  ( 133.6922820468854241, -1.999999999999981348, -0.6060766987539614181 ) ) ;
#16891 = CARTESIAN_POINT ( 'NONE',  ( 13.11714404544056656, 8.568033937426095648, -15.91706119101506545 ) ) ;
#16892 = LINE ( 'NONE', #18882, #478 ) ;
#16893 = CARTESIAN_POINT ( 'NONE',  ( 172.0152310637604103, -9.999999999999996447, -8.721423840594312082 ) ) ;
#16894 = VERTEX_POINT ( 'NONE', #10188 ) ;
#16895 = DIRECTION ( 'NONE',  ( 1.000000000000000000, 4.440892098500622217E-16, 0.000000000000000000 ) ) ;
#16896 = EDGE_CURVE ( 'NONE', #2945, #28540, #2899, .T. ) ;
#16897 = EDGE_CURVE ( 'NONE', #6558, #8041, #5170, .T. ) ;
#16898 = DIRECTION ( 'NONE',  ( -0.9510565162951536422, -2.566386769018988323E-16, 0.3090169943749475623 ) ) ;
#16899 = VERTEX_POINT ( 'NONE', #19053 ) ;
#16900 = EDGE_CURVE ( 'NONE', #4823, #23552, #5626, .T. ) ;
#16901 = EDGE_LOOP ( 'NONE', ( #9616, #3945, #26704, #8066 ) ) ;
#16902 = EDGE_CURVE ( 'NONE', #17958, #10367, #7757, .T. ) ;
#16903 = CARTESIAN_POINT ( 'NONE',  ( 11.25771276049011327, 8.953580691464267716, -17.22628983894280807 ) ) ;
#16904 = CARTESIAN_POINT ( 'NONE',  ( 27.60672911170952304, -4.775276709060196190, -16.23362067418393195 ) ) ;
#16905 = CARTESIAN_POINT ( 'NONE',  ( 24.30592326428028827, -5.273034306582022879, -19.67074064463221106 ) ) ;
#16906 = AXIS2_PLACEMENT_3D ( 'NONE', #14068, #21250, #12088 ) ;
#16907 = LINE ( 'NONE', #3490, #10639 ) ;
#16908 = CARTESIAN_POINT ( 'NONE',  ( 132.0152310637605808, -10.00000000000000711, -15.61832212156129351 ) ) ;
#16909 = CYLINDRICAL_SURFACE ( 'NONE', #11794, 3.000000000000002665 ) ;
#16910 = VECTOR ( 'NONE', #10059, 1000.000000000000000 ) ;
#16911 = EDGE_LOOP ( 'NONE', ( #27671, #24967, #8250, #13669 ) ) ;
#16912 = PLANE ( 'NONE',  #6469 ) ;
#16913 = DIRECTION ( 'NONE',  ( 1.000000000000000000, 0.000000000000000000, 0.000000000000000000 ) ) ;
#16914 = CARTESIAN_POINT ( 'NONE',  ( 164.7287565553229172, -4.999999999999973355, -16.50000000000000000 ) ) ;
#16915 = DIRECTION ( 'NONE',  ( 0.5877852522924731371, 1.586114251531760728E-16, 0.8090169943749474513 ) ) ;
#16916 = DIRECTION ( 'NONE',  ( -2.698458740408365879E-16, 1.000000000000000000, 0.000000000000000000 ) ) ;
#16917 = CARTESIAN_POINT ( 'NONE',  ( 10.49225533350670858, 16.35939020308235925, -17.32643665990597981 ) ) ;
#16918 = EDGE_CURVE ( 'NONE', #5616, #18859, #29014, .T. ) ;
#16919 = PLANE ( 'NONE',  #20875 ) ;
#16920 = CARTESIAN_POINT ( 'NONE',  ( 32.77977724007769211, -11.13765286058784554, -18.71157503069099448 ) ) ;
#16921 = ORIENTED_EDGE ( 'NONE', *, *, #21862, .T. ) ;
#16922 = CARTESIAN_POINT ( 'NONE',  ( 13.37720302390605553, 7.624891072754538257, -15.70979247928349132 ) ) ;
#16923 = LINE ( 'NONE', #9899, #18280 ) ;
#16924 = VECTOR ( 'NONE', #29507, 1000.000000000000000 ) ;
#16925 = CARTESIAN_POINT ( 'NONE',  ( 21.40051611374530793, -0.1690565882708310874, -20.18282279970310000 ) ) ;
#16926 = CARTESIAN_POINT ( 'NONE',  ( 12.86729516143382845, 9.515644835462770956, -16.11619563230584973 ) ) ;
#16927 = FACE_BOUND ( 'NONE', #15805, .T. ) ;
#16928 = VERTEX_POINT ( 'NONE', #14906 ) ;
#16929 = ORIENTED_EDGE ( 'NONE', *, *, #11687, .T. ) ;
#16930 = AXIS2_PLACEMENT_3D ( 'NONE', #369, #7525, #21566 ) ;
#16931 = CARTESIAN_POINT ( 'NONE',  ( 10.07879545831710999, 15.66271422494645904, -16.43741374977755143 ) ) ;
#16932 = DIRECTION ( 'NONE',  ( -0.5877852522924731371, 0.000000000000000000, 0.8090169943749474513 ) ) ;
#16933 = CARTESIAN_POINT ( 'NONE',  ( 9.649959050778257108, 17.62941265384766254, -17.56860460898032628 ) ) ;
#16934 = CARTESIAN_POINT ( 'NONE',  ( 171.1922820468853672, -9.999999999999994671, -30.91696583120936026 ) ) ;
#16935 = EDGE_LOOP ( 'NONE', ( #7443, #15176, #9826, #28772 ) ) ;
#16936 = EDGE_CURVE ( 'NONE', #14997, #19874, #24250, .T. ) ;
#16937 = FACE_OUTER_BOUND ( 'NONE', #15098, .T. ) ;
#16938 = ORIENTED_EDGE ( 'NONE', *, *, #25610, .F. ) ;
#16939 = EDGE_CURVE ( 'NONE', #4559, #27662, #28554, .T. ) ;
#16940 = CARTESIAN_POINT ( 'NONE',  ( 12.07790154976966868, 9.144051220271959934, -16.66639656463015839 ) ) ;
#16941 = ORIENTED_EDGE ( 'NONE', *, *, #6263, .T. ) ;
#16942 = VECTOR ( 'NONE', #788, 1000.000000000000000 ) ;
#16943 = CARTESIAN_POINT ( 'NONE',  ( 34.08234396701924851, -12.11069646272769162, -20.88346212624082909 ) ) ;
#16944 = CARTESIAN_POINT ( 'NONE',  ( 16.19004574127830054, 9.516462436566445859, -20.03842800660303070 ) ) ;
#16945 = CARTESIAN_POINT ( 'NONE',  ( 15.30534275580653869, 10.60631812597827839, -15.20037037882373987 ) ) ;
#16946 = VERTEX_POINT ( 'NONE', #601 ) ;
#16947 = CARTESIAN_POINT ( 'NONE',  ( 130.7287565553229172, -4.999999999999983125, -30.76635726929465875 ) ) ;
#16948 = VERTEX_POINT ( 'NONE', #24398 ) ;
#16949 = CARTESIAN_POINT ( 'NONE',  ( 34.18187006836440389, -11.68445768601494628, -19.79758194388510972 ) ) ;
#16950 = SHAPE_DEFINITION_REPRESENTATION ( #22776, #19847 ) ;
#16951 = CARTESIAN_POINT ( 'NONE',  ( 18.98834166481877972, 4.258514017552020192, -15.11364409576566459 ) ) ;
#16952 = CARTESIAN_POINT ( 'NONE',  ( 17.21692058948253035, 4.245457944912791604, -14.13226496128363863 ) ) ;
#16953 = CIRCLE ( 'NONE', #6223, 2.000000000000000000 ) ;
#16954 = ORIENTED_EDGE ( 'NONE', *, *, #8271, .T. ) ;
#16955 = DIRECTION ( 'NONE',  ( 0.000000000000000000, 0.000000000000000000, -1.000000000000000000 ) ) ;
#16956 = FACE_BOUND ( 'NONE', #24569, .T. ) ;
#16957 = VECTOR ( 'NONE', #5807, 1000.000000000000000 ) ;
#16958 = VERTEX_POINT ( 'NONE', #9886 ) ;
#16959 = EDGE_CURVE ( 'NONE', #26148, #4081, #3495, .T. ) ;
#16960 = DIRECTION ( 'NONE',  ( 0.5877852522924731371, 0.000000000000000000, 0.8090169943749474513 ) ) ;
#16961 = DIRECTION ( 'NONE',  ( 0.000000000000000000, 0.000000000000000000, 1.000000000000000000 ) ) ;
#16962 = VECTOR ( 'NONE', #10532, 1000.000000000000000 ) ;
#16963 = CARTESIAN_POINT ( 'NONE',  ( 162.0152310637604955, -9.999999999999998224, -15.61832212156129707 ) ) ;
#16964 = CARTESIAN_POINT ( 'NONE',  ( 162.0152310637604387, -9.999999999999998224, -8.721423840594312082 ) ) ;
#16965 = CARTESIAN_POINT ( 'NONE',  ( 12.14726737398757095, 10.08919500705755645, -15.36430154580878593 ) ) ;
#16966 = CARTESIAN_POINT ( 'NONE',  ( 151.1922820468853956, -4.999999999999976907, -13.59645775552055902 ) ) ;
#16967 = VERTEX_POINT ( 'NONE', #7607 ) ;
#16968 = CARTESIAN_POINT ( 'NONE',  ( 143.6922820468853956, -1.999999999999978684, -0.6060766987539614181 ) ) ;
#16969 = ORIENTED_EDGE ( 'NONE', *, *, #19315, .T. ) ;
#16970 = CARTESIAN_POINT ( 'NONE',  ( 12.43696608443014284, 8.546664718661613591, -15.18012293544581226 ) ) ;
#16971 = ORIENTED_EDGE ( 'NONE', *, *, #15971, .T. ) ;
#16972 = AXIS2_PLACEMENT_3D ( 'NONE', #20079, #8914, #18230 ) ;
#16973 = CARTESIAN_POINT ( 'NONE',  ( 20.29966856415212817, 4.923229158599749411, -18.85509502865480869 ) ) ;
#16974 = DIRECTION ( 'NONE',  ( 0.9510565162951536422, 0.000000000000000000, -0.3090169943749475623 ) ) ;
#16975 = CARTESIAN_POINT ( 'NONE',  ( 5.000000000000006217, 2.220446049250313870E-15, -25.03750572909317285 ) ) ;
#16976 = DIRECTION ( 'NONE',  ( -0.9510565162951536422, -2.566386769018988816E-16, -0.3090169943749472292 ) ) ;
#16977 = VERTEX_POINT ( 'NONE', #9736 ) ;
#16978 = DIRECTION ( 'NONE',  ( 0.000000000000000000, 0.000000000000000000, -1.000000000000000000 ) ) ;
#16979 = CARTESIAN_POINT ( 'NONE',  ( 12.82818608578791064, 9.559270667424515366, -16.14272081857926366 ) ) ;
#16980 = ORIENTED_EDGE ( 'NONE', *, *, #20240, .F. ) ;
#16981 = VECTOR ( 'NONE', #932, 1000.000000000000000 ) ;
#16982 = CARTESIAN_POINT ( 'NONE',  ( 33.26400919001463308, -11.80307911188568148, -18.11217348381727632 ) ) ;
#16983 = CARTESIAN_POINT ( 'NONE',  ( 21.64656857049893901, 5.639188926465734220, -17.17864421186117951 ) ) ;
#16984 = DIRECTION ( 'NONE',  ( -2.698458740408365879E-16, 1.000000000000000000, 0.000000000000000000 ) ) ;
#16985 = CARTESIAN_POINT ( 'NONE',  ( 16.38240814442996651, 6.370603895193741373, -13.89573738210111919 ) ) ;
#16986 = ORIENTED_EDGE ( 'NONE', *, *, #19852, .T. ) ;
#16987 = DIRECTION ( 'NONE',  ( -0.5877852522924731371, 0.000000000000000000, 0.8090169943749474513 ) ) ;
#16988 = SURFACE_SIDE_STYLE ('',( #26621 ) ) ;
#16989 = VECTOR ( 'NONE', #2908, 1000.000000000000000 ) ;
#16990 = CARTESIAN_POINT ( 'NONE',  ( 20.86695504291294156, -3.984745147917406971, -17.88565525751875995 ) ) ;
#16991 = CARTESIAN_POINT ( 'NONE',  ( 17.86202776125589153, 5.750484210099715554, -19.07881598002096268 ) ) ;
#16992 = ORIENTED_EDGE ( 'NONE', *, *, #22203, .F. ) ;
#16993 = DIRECTION ( 'NONE',  ( -1.000000000000000000, 0.000000000000000000, 0.000000000000000000 ) ) ;
#16994 = ORIENTED_EDGE ( 'NONE', *, *, #20511, .F. ) ;
#16995 = EDGE_LOOP ( 'NONE', ( #9611, #13969, #1532, #4265 ) ) ;
#16996 = DIRECTION ( 'NONE',  ( -2.698458740408365879E-16, 1.000000000000000000, 0.000000000000000000 ) ) ;
#16997 = LINE ( 'NONE', #538, #27007 ) ;
#16998 = EDGE_CURVE ( 'NONE', #1088, #19198, #3347, .T. ) ;
#16999 = EDGE_CURVE ( 'NONE', #23759, #28590, #5322, .T. ) ;
#17000 = CARTESIAN_POINT ( 'NONE',  ( 2.644994884459111795, -7.710515798486395234, -0.08224679563973184837 ) ) ;
#17001 = VECTOR ( 'NONE', #29097, 1000.000000000000000 ) ;
#17002 = DIRECTION ( 'NONE',  ( -2.698458740408365879E-16, 1.000000000000000000, -0.000000000000000000 ) ) ;
#17003 = EDGE_CURVE ( 'NONE', #10176, #28903, #26091, .T. ) ;
#17004 = CARTESIAN_POINT ( 'NONE',  ( 169.5152310637604671, -4.999999999999971578, -1.881997125516404380E-14 ) ) ;
#17005 = EDGE_CURVE ( 'NONE', #28689, #3516, #12323, .T. ) ;
#17006 = CARTESIAN_POINT ( 'NONE',  ( 11.48249212886396897, 9.228508165798535501, -15.85668214399537845 ) ) ;
#17007 = CIRCLE ( 'NONE', #22880, 12.50000000000000000 ) ;
#17008 = CARTESIAN_POINT ( 'NONE',  ( 28.49100808714443289, -10.93160309251996765, -13.65156567797833631 ) ) ;
#17009 = CARTESIAN_POINT ( 'NONE',  ( 27.20456514074317056, -5.347416052021189081, -13.22196079581408235 ) ) ;
#17011 = ORIENTED_EDGE ( 'NONE', *, *, #15789, .F. ) ;
#17010 = CARTESIAN_POINT ( 'NONE',  ( 32.54305136433941215, -11.03529315477374517, -18.08112484791816499 ) ) ;
#17012 = DIRECTION ( 'NONE',  ( 1.000000000000000000, 2.220446049250312686E-15, 0.000000000000000000 ) ) ;
#17013 = DIRECTION ( 'NONE',  ( -0.8090169943749474513, -2.183098979609982436E-16, -0.5877852522924731371 ) ) ;
#17014 = CARTESIAN_POINT ( 'NONE',  ( 134.5152310637605524, -1.999999999999980460, -13.05155085951650840 ) ) ;
#17015 = FACE_OUTER_BOUND ( 'NONE', #15345, .T. ) ;
#17016 = CARTESIAN_POINT ( 'NONE',  ( 6.938893903907228378E-15, 60.00000000000000711, -1.040834085586084257E-14 ) ) ;
#17017 = CARTESIAN_POINT ( 'NONE',  ( 167.0152310637605524, -1.999999999999970468, -32.93883019725009120 ) ) ;
#17018 = CARTESIAN_POINT ( 'NONE',  ( 19.38992137333195842, 2.881095379261479739, -20.30776781288435373 ) ) ;
#17019 = ORIENTED_EDGE ( 'NONE', *, *, #26018, .F. ) ;
#17020 = CARTESIAN_POINT ( 'NONE',  ( 153.6922820468853672, -1.999999999999975797, -9.266330736598359152 ) ) ;
#17021 = CARTESIAN_POINT ( 'NONE',  ( 10.72145343393089512, 16.62815948516130504, -15.95392576598924350 ) ) ;
#17022 = DIRECTION ( 'NONE',  ( 0.9510565162951535312, 2.566386769018988816E-16, -0.3090169943749475623 ) ) ;
#17023 = FACE_OUTER_BOUND ( 'NONE', #5989, .T. ) ;
#17024 = CARTESIAN_POINT ( 'NONE',  ( 19.83745040964868522, -2.306422872736943575, -14.39351019504378293 ) ) ;
#17025 = CARTESIAN_POINT ( 'NONE',  ( 30.21326039400183561, -7.476461571224066738, -17.86537319528562051 ) ) ;
#17026 = ORIENTED_EDGE ( 'NONE', *, *, #12035, .T. ) ;
#17027 = CARTESIAN_POINT ( 'NONE',  ( 32.67186286342521839, -11.06527230177895227, -18.43913201350460440 ) ) ;
#17028 = VECTOR ( 'NONE', #4616, 1000.000000000000000 ) ;
#17029 = CARTESIAN_POINT ( 'NONE',  ( 25.72346593501046996, -2.209713236584236018, -16.07608620281017053 ) ) ;
#17030 = CARTESIAN_POINT ( 'NONE',  ( 19.42159491456138554, 2.195880709831018684, -14.63272625841335106 ) ) ;
#17031 = AXIS2_PLACEMENT_3D ( 'NONE', #23461, #28382, #7437 ) ;
#17032 = EDGE_LOOP ( 'NONE', ( #494, #13738, #27832, #5224 ) ) ;
#17033 = LINE ( 'NONE', #10304, #12820 ) ;
#17034 = ORIENTED_EDGE ( 'NONE', *, *, #19173, .T. ) ;
#17035 = ADVANCED_FACE ( 'NONE', ( #738 ), #10033, .T. ) ;
#17036 = DIRECTION ( 'NONE',  ( 0.000000000000000000, 0.000000000000000000, -1.000000000000000000 ) ) ;
#17037 = DIRECTION ( 'NONE',  ( 1.000000000000000000, 0.000000000000000000, 0.000000000000000000 ) ) ;
#17038 = ADVANCED_FACE ( 'NONE', ( #3198 ), #12476, .T. ) ;
#17039 = EDGE_CURVE ( 'NONE', #14997, #18781, #8200, .T. ) ;
#17040 = DIRECTION ( 'NONE',  ( 0.000000000000000000, 0.000000000000000000, -1.000000000000000000 ) ) ;
#17041 = EDGE_CURVE ( 'NONE', #14797, #2212, #17511, .T. ) ;
#17042 = CARTESIAN_POINT ( 'NONE',  ( -4.000000000000003553, 1.557668341133518153, -2.290303434304242547 ) ) ;
#17043 = CARTESIAN_POINT ( 'NONE',  ( 33.28625081342995884, -10.37305140221732991, -17.94975064729133862 ) ) ;
#17044 = VECTOR ( 'NONE', #23353, 1000.000000000000000 ) ;
#17045 = CARTESIAN_POINT ( 'NONE',  ( 10.07879545831710999, 15.66271422494645904, -16.43741374977755143 ) ) ;
#17046 = VECTOR ( 'NONE', #29566, 1000.000000000000000 ) ;
#17047 = DIRECTION ( 'NONE',  ( 1.000000000000000000, 4.440892098500623203E-16, 0.000000000000000000 ) ) ;
#17048 = CARTESIAN_POINT ( 'NONE',  ( 79.91207320562929795, -4.999999999999995559, 58.05951968496736981 ) ) ;
#17049 = CARTESIAN_POINT ( 'NONE',  ( 12.06596557120094992, 9.177570865404522493, -16.67295095431955332 ) ) ;
#17050 = CARTESIAN_POINT ( 'NONE',  ( 136.1922820468854241, -10.00000000000000533, -19.40354224447947473 ) ) ;
#17051 = DIRECTION ( 'NONE',  ( -0.5877852522924731371, -1.586114251531760235E-16, 0.8090169943749474513 ) ) ;
#17052 = VERTEX_POINT ( 'NONE', #10946 ) ;
#17053 = CARTESIAN_POINT ( 'NONE',  ( 138.6922820468854525, -10.00000000000000533, -17.92658477444275533 ) ) ;
#17054 = CARTESIAN_POINT ( 'NONE',  ( 149.5152310637606092, -4.999999999999976907, -28.60870317832789667 ) ) ;
#17055 = CARTESIAN_POINT ( 'NONE',  ( 12.74999999999999822, 7.511012776518213930E-16, -5.000000000000000888 ) ) ;
#17056 = ORIENTED_EDGE ( 'NONE', *, *, #5713, .T. ) ;
#17057 = ORIENTED_EDGE ( 'NONE', *, *, #24563, .T. ) ;
#17058 = ORIENTED_EDGE ( 'NONE', *, *, #6601, .F. ) ;
#17059 = CARTESIAN_POINT ( 'NONE',  ( 12.60230244812736800, 7.534144488243946114, -16.30820540178382316 ) ) ;
#17060 = ORIENTED_EDGE ( 'NONE', *, *, #29864, .F. ) ;
#17061 = CARTESIAN_POINT ( 'NONE',  ( 24.24519292511275737, -8.489478586693508078, -18.02380513063773648 ) ) ;
#17062 = CARTESIAN_POINT ( 'NONE',  ( 26.86433939054618492, -2.362129714094441724, -16.96571632802953644 ) ) ;
#17063 = DIRECTION ( 'NONE',  ( -0.8090169943749474513, -2.183098979609982436E-16, 0.5877852522924731371 ) ) ;
#17064 = CARTESIAN_POINT ( 'NONE',  ( 174.5152310637604103, -9.999999999999994671, -2.627941064794695691 ) ) ;
#17065 = DIRECTION ( 'NONE',  ( -2.698458740408365879E-16, 1.000000000000000000, 0.000000000000000000 ) ) ;
#17066 = AXIS2_PLACEMENT_3D ( 'NONE', #17050, #15344, #8339 ) ;
#17067 = DIRECTION ( 'NONE',  ( 0.5877852522924731371, 1.586114251531760728E-16, 0.8090169943749474513 ) ) ;
#17068 = DIRECTION ( 'NONE',  ( 0.5877852522924731371, 0.000000000000000000, 0.8090169943749474513 ) ) ;
#17069 = CARTESIAN_POINT ( 'NONE',  ( -1.310841663519413114, -1.387778780781445676E-16, 5.000000000000000888 ) ) ;
#17070 = EDGE_CURVE ( 'NONE', #2926, #4706, #3637, .T. ) ;
#17071 = CARTESIAN_POINT ( 'NONE',  ( 171.1922820468853672, -9.999999999999994671, -28.06379628232387802 ) ) ;
#17072 = CARTESIAN_POINT ( 'NONE',  ( 127.1715206774213840, -4.999999999999983125, -92.39551812325976243 ) ) ;
#17073 = EDGE_CURVE ( 'NONE', #29440, #12783, #15217, .T. ) ;
#17074 = EDGE_CURVE ( 'NONE', #5150, #25448, #25147, .T. ) ;
#17075 = ADVANCED_FACE ( 'NONE', ( #22100 ), #17663, .T. ) ;
#17076 = VECTOR ( 'NONE', #28080, 1000.000000000000000 ) ;
#17077 = CARTESIAN_POINT ( 'NONE',  ( 10.47300640208398370, 16.44766825625507778, -17.33439677017039671 ) ) ;
#17078 = CARTESIAN_POINT ( 'NONE',  ( 35.54287943964028784, -22.15884374752674546, -18.65915260879160797 ) ) ;
#17079 = ORIENTED_EDGE ( 'NONE', *, *, #26474, .T. ) ;
#17080 = VECTOR ( 'NONE', #2202, 999.9999999999998863 ) ;
#17081 = CARTESIAN_POINT ( 'NONE',  ( 8.944584683310379702, 16.95159276115599667, -17.92015940598198753 ) ) ;
#17082 = CARTESIAN_POINT ( 'NONE',  ( 96.02733224039648974, -4.999999999999991118, -69.76794072354836374 ) ) ;
#17083 = CARTESIAN_POINT ( 'NONE',  ( 24.00918528248616468, -0.5066965781341161712, -13.81223085940890627 ) ) ;
#17084 = CARTESIAN_POINT ( 'NONE',  ( 12.83226850357503501, 9.540548187773516986, -16.14103259455261608 ) ) ;
#17085 = FACE_BOUND ( 'NONE', #7419, .T. ) ;
#17086 = VERTEX_POINT ( 'NONE', #26867 ) ;
#17087 = CARTESIAN_POINT ( 'NONE',  ( 11.47310491742633687, 9.268236560789974376, -15.86081749295074594 ) ) ;
#17088 = CARTESIAN_POINT ( 'NONE',  ( 162.0152310637604671, -9.999999999999998224, -17.38167787843871182 ) ) ;
#17089 = CARTESIAN_POINT ( 'NONE',  ( 12.23783994716398560, 8.515526397163364791, -15.33449341356891615 ) ) ;
#17090 = CYLINDRICAL_SURFACE ( 'NONE', #23271, 5.000000000000000000 ) ;
#17091 = VERTEX_POINT ( 'NONE', #22409 ) ;
#17092 = DIRECTION ( 'NONE',  ( -0.9510565162951536422, 0.000000000000000000, -0.3090169943749472292 ) ) ;
#17093 = ORIENTED_EDGE ( 'NONE', *, *, #1661, .T. ) ;
#17094 = CARTESIAN_POINT ( 'NONE',  ( 12.40302661446015264, 8.678734247659738443, -16.45371344743900366 ) ) ;
#17095 = ORIENTED_EDGE ( 'NONE', *, *, #9341, .T. ) ;
#17096 = CARTESIAN_POINT ( 'NONE',  ( 35.74526169011073762, -19.57556970876266433, -21.38945728569726867 ) ) ;
#17097 = CARTESIAN_POINT ( 'NONE',  ( 27.26129135193747999, -10.77754955263135095, -18.64424489656416739 ) ) ;
#17098 = CARTESIAN_POINT ( 'NONE',  ( 13.52175692814481067, 9.804829593628518580, -15.59458061523717909 ) ) ;
#17099 = LINE ( 'NONE', #10220, #23318 ) ;
#17100 = LINE ( 'NONE', #26427, #3048 ) ;
#17101 = VECTOR ( 'NONE', #17195, 1000.000000000000000 ) ;
#17102 = APPLICATION_PROTOCOL_DEFINITION ( 'draft international standard', 'automotive_design', 1998, #17667 ) ;
#17103 = ORIENTED_EDGE ( 'NONE', *, *, #26527, .F. ) ;
#17104 = CARTESIAN_POINT ( 'NONE',  ( 19.79871159306781436, 4.571585941193342606, -15.48227718036497080 ) ) ;
#17105 = AXIS2_PLACEMENT_3D ( 'NONE', #4296, #22922, #25647 ) ;
#17106 = CARTESIAN_POINT ( 'NONE',  ( 16.57956996521092918, 4.788269978297743812, -19.71382457362092566 ) ) ;
#17107 = DIRECTION ( 'NONE',  ( -0.5877852522924731371, -1.586114251531760728E-16, -0.8090169943749474513 ) ) ;
#17108 = CARTESIAN_POINT ( 'NONE',  ( 0.6543461111163458854, 4.241015250120808489, -0.1391502195351409232 ) ) ;
#17109 = ADVANCED_FACE ( 'NONE', ( #15365 ), #27022, .T. ) ;
#17110 = ADVANCED_FACE ( 'NONE', ( #8508 ), #19797, .T. ) ;
#17111 = CYLINDRICAL_SURFACE ( 'NONE', #13548, 5.000000000000006217 ) ;
#17112 = FACE_OUTER_BOUND ( 'NONE', #12287, .T. ) ;
#17113 = LINE ( 'NONE', #5522, #7759 ) ;
#17114 = EDGE_LOOP ( 'NONE', ( #7676, #23916, #19900, #1524, #17477 ) ) ;
#17115 = FACE_OUTER_BOUND ( 'NONE', #25970, .T. ) ;
#17116 = CARTESIAN_POINT ( 'NONE',  ( 12.26306961015461461, 9.515005556349402482, -15.31970085818224980 ) ) ;
#17118 = VECTOR ( 'NONE', #2683, 999.9999999999998863 ) ;
#17117 = DIRECTION ( 'NONE',  ( 0.5877852522924731371, 0.000000000000000000, 0.8090169943749474513 ) ) ;
#17119 = CARTESIAN_POINT ( 'NONE',  ( 6.385173589811359740, -5.000000000000015987, 19.65154363936862936 ) ) ;
#17120 = ORIENTED_EDGE ( 'NONE', *, *, #9372, .T. ) ;
#17121 = VECTOR ( 'NONE', #28662, 1000.000000000000000 ) ;
#17122 = CARTESIAN_POINT ( 'NONE',  ( 11.47464782381437587, 9.261287281732329291, -15.86016978468419936 ) ) ;
#17123 = ORIENTED_EDGE ( 'NONE', *, *, #30222, .T. ) ;
#17124 = CARTESIAN_POINT ( 'NONE',  ( 18.39947282702827991, 3.040288584705510999, -19.58888106367123427 ) ) ;
#17125 = DIRECTION ( 'NONE',  ( 0.9510565162951535312, 2.566386769018988816E-16, -0.3090169943749475623 ) ) ;
#17126 = CARTESIAN_POINT ( 'NONE',  ( 8.000000000000010658, 4.618802153517005848, -5.000000000000000888 ) ) ;
#17127 = FACE_OUTER_BOUND ( 'NONE', #25851, .T. ) ;
#17128 = VERTEX_POINT ( 'NONE', #27332 ) ;
#17129 = DIRECTION ( 'NONE',  ( 0.3090169943749472292, 8.338696094057992503E-17, -0.9510565162951536422 ) ) ;
#17130 = ORIENTED_EDGE ( 'NONE', *, *, #29204, .F. ) ;
#17131 = CARTESIAN_POINT ( 'NONE',  ( 11.92449941057312124, 13.70369295321711256, -16.51642704783386506 ) ) ;
#17132 = EDGE_LOOP ( 'NONE', ( #30072, #25304, #261, #23833 ) ) ;
#17133 = CARTESIAN_POINT ( 'NONE',  ( 36.49521523454778560, -20.94471372247522467, -19.05937150832556526 ) ) ;
#17134 = CARTESIAN_POINT ( 'NONE',  ( 15.93484470893836935, 6.939319753835953009, -14.67888072223970752 ) ) ;
#17135 = ORIENTED_EDGE ( 'NONE', *, *, #21722, .T. ) ;
#17136 = ORIENTED_EDGE ( 'NONE', *, *, #21098, .F. ) ;
#17137 = DIRECTION ( 'NONE',  ( 0.000000000000000000, 0.000000000000000000, -1.000000000000000000 ) ) ;
#17138 = CARTESIAN_POINT ( 'NONE',  ( 15.84550288711180777, 10.06862660282224731, -14.00251831694083826 ) ) ;
#17139 = ORIENTED_EDGE ( 'NONE', *, *, #21094, .F. ) ;
#17140 = CARTESIAN_POINT ( 'NONE',  ( 6.938893903907228378E-15, 60.00000000000000711, -1.040834085586084257E-14 ) ) ;
#17141 = EDGE_CURVE ( 'NONE', #29995, #20158, #22251, .T. ) ;
#17142 = CARTESIAN_POINT ( 'NONE',  ( 19.87821071931953298, -1.530402839103173651, -15.12151443550766494 ) ) ;
#17143 = CARTESIAN_POINT ( 'NONE',  ( 19.77208840006000656, -0.3814412559078061982, -20.24210485642555568 ) ) ;
#17144 = VERTEX_POINT ( 'NONE', #1359 ) ;
#17145 = CARTESIAN_POINT ( 'NONE',  ( 25.00000000000000000, 0.000000000000000000, 0.000000000000000000 ) ) ;
#17146 = EDGE_LOOP ( 'NONE', ( #30017, #28525 ) ) ;
#17147 = DIRECTION ( 'NONE',  ( 0.000000000000000000, 0.000000000000000000, -1.000000000000000000 ) ) ;
#17148 = EDGE_CURVE ( 'NONE', #23355, #13222, #24706, .T. ) ;
#17149 = PLANE ( 'NONE',  #15268 ) ;
#17150 = DIRECTION ( 'NONE',  ( -2.207829878515935943E-16, -1.000000000000000000, -0.000000000000000000 ) ) ;
#17151 = DIRECTION ( 'NONE',  ( 0.9510565162951535312, 2.566386769018988816E-16, -0.3090169943749475623 ) ) ;
#17152 = VECTOR ( 'NONE', #2668, 1000.000000000000000 ) ;
#17153 = FACE_OUTER_BOUND ( 'NONE', #16419, .T. ) ;
#17154 = CARTESIAN_POINT ( 'NONE',  ( 11.47327446659168615, 9.267463859335506982, -15.86074700677745852 ) ) ;
#17155 = CARTESIAN_POINT ( 'NONE',  ( 29.74223563811278481, -10.39579538818624549, -13.90533736129563813 ) ) ;
#17156 = CARTESIAN_POINT ( 'NONE',  ( 24.59824444495380646, -5.013944910511990649, -19.70109713935865514 ) ) ;
#17158 = ORIENTED_EDGE ( 'NONE', *, *, #10382, .T. ) ;
#17157 = CARTESIAN_POINT ( 'NONE',  ( 32.48283477683061449, -11.02614750807341260, -17.91093295056291979 ) ) ;
#17159 = DIRECTION ( 'NONE',  ( -1.000000000000000000, -4.440892098500622217E-16, 0.000000000000000000 ) ) ;
#17160 = FACE_BOUND ( 'NONE', #19248, .T. ) ;
#17161 = CARTESIAN_POINT ( 'NONE',  ( -2.000000000000008882, 3.464101615137750390, -2.450000000000000622 ) ) ;
#17162 = CARTESIAN_POINT ( 'NONE',  ( 142.2287565553230309, -1.999999999999978018, -20.83012701892220164 ) ) ;
#17163 = FACE_OUTER_BOUND ( 'NONE', #7239, .T. ) ;
#17165 = EDGE_LOOP ( 'NONE', ( #26155, #8358, #23868, #17912, #8398 ) ) ;
#17164 = CARTESIAN_POINT ( 'NONE',  ( 17.55424633453837302, 0.6138019359854992585, -14.89346452969079060 ) ) ;
#17166 = VERTEX_POINT ( 'NONE', #13386 ) ;
#17167 = DIRECTION ( 'NONE',  ( 0.000000000000000000, 0.000000000000000000, 1.000000000000000000 ) ) ;
#17168 = CARTESIAN_POINT ( 'NONE',  ( 12.21210587983259366, 9.791837354264822935, -15.33748854281299323 ) ) ;
#17169 = CARTESIAN_POINT ( 'NONE',  ( 174.7287565553228887, -1.999999999999969358, -16.50000000000000355 ) ) ;
#17170 = FACE_OUTER_BOUND ( 'NONE', #18783, .T. ) ;
#17171 = ORIENTED_EDGE ( 'NONE', *, *, #11992, .F. ) ;
#17172 = CARTESIAN_POINT ( 'NONE',  ( 20.24985932600369409, 3.694099309552050237, -20.13309853732883781 ) ) ;
#17173 = CARTESIAN_POINT ( 'NONE',  ( 15.23446545079332815, 2.143032791470029341, -16.75203451335420368 ) ) ;
#17174 = ORIENTED_EDGE ( 'NONE', *, *, #12511, .T. ) ;
#17175 = CARTESIAN_POINT ( 'NONE',  ( 34.11209566957792561, -15.73109017586260272, -19.92372960426217787 ) ) ;
#17176 = EDGE_CURVE ( 'NONE', #29938, #7935, #18665, .T. ) ;
#17177 = ORIENTED_EDGE ( 'NONE', *, *, #28836, .F. ) ;
#17178 = CARTESIAN_POINT ( 'NONE',  ( 22.80194228990702143, -6.214338098008789224, -14.16187805771452801 ) ) ;
#17179 = EDGE_CURVE ( 'NONE', #21366, #19068, #18113, .T. ) ;
#17180 = VECTOR ( 'NONE', #7314, 1000.000000000000000 ) ;
#17181 = CARTESIAN_POINT ( 'NONE',  ( 26.10879525372914145, -2.341005984040549937, -13.07697618282131913 ) ) ;
#17182 = EDGE_LOOP ( 'NONE', ( #5778, #1385, #3437, #1728 ) ) ;
#17183 = CARTESIAN_POINT ( 'NONE',  ( 24.14317479683219858, -6.286850201977149055, -18.60698471650063723 ) ) ;
#17184 = AXIS2_PLACEMENT_3D ( 'NONE', #20640, #30023, #27713 ) ;
#17185 = VECTOR ( 'NONE', #8800, 1000.000000000000000 ) ;
#17186 = PLANE ( 'NONE',  #14747 ) ;
#17187 = ORIENTED_EDGE ( 'NONE', *, *, #17366, .T. ) ;
#17188 = FACE_OUTER_BOUND ( 'NONE', #5081, .T. ) ;
#17189 = DIRECTION ( 'NONE',  ( -0.000000000000000000, 1.000000000000000000, 0.000000000000000000 ) ) ;
#17190 = DIRECTION ( 'NONE',  ( -1.110223024625156540E-16, 0.000000000000000000, -1.000000000000000000 ) ) ;
#17191 = CARTESIAN_POINT ( 'NONE',  ( 13.51621490077814691, 9.019785729699995258, -14.32023381125561556 ) ) ;
#17192 = CARTESIAN_POINT ( 'NONE',  ( 33.24108837279852224, -10.36619216719171632, -17.82210672427467912 ) ) ;
#17193 = CARTESIAN_POINT ( 'NONE',  ( 9.917712295358372288, 16.40146214360271770, -16.50402730409559027 ) ) ;
#17194 = VECTOR ( 'NONE', #15105, 1000.000000000000000 ) ;
#17195 = DIRECTION ( 'NONE',  ( 0.5877852522924731371, 1.586114251531760728E-16, 0.8090169943749474513 ) ) ;
#17196 = DIRECTION ( 'NONE',  ( -0.5877852522924731371, 0.000000000000000000, 0.8090169943749474513 ) ) ;
#17197 = CARTESIAN_POINT ( 'NONE',  ( 12.02685106364323531, 9.321538569219327997, -16.69182734290254899 ) ) ;
#17198 = LINE ( 'NONE', #27599, #17537 ) ;
#17199 = CARTESIAN_POINT ( 'NONE',  ( 138.6922820468854525, -1.999999999999979128, -15.07341522555727309 ) ) ;
#17200 = ORIENTED_EDGE ( 'NONE', *, *, #20775, .T. ) ;
#17201 = LINE ( 'NONE', #21930, #8080 ) ;
#17202 = LINE ( 'NONE', #12460, #24921 ) ;
#17203 = CARTESIAN_POINT ( 'NONE',  ( 159.5152310637604955, -9.999999999999998224, -21.71180489736091346 ) ) ;
#17205 = EDGE_LOOP ( 'NONE', ( #19946, #11767, #29793, #26110 ) ) ;
#17204 = VECTOR ( 'NONE', #3795, 1000.000000000000000 ) ;
#17206 = ORIENTED_EDGE ( 'NONE', *, *, #14822, .T. ) ;
#17207 = VERTEX_POINT ( 'NONE', #8359 ) ;
#17208 = CARTESIAN_POINT ( 'NONE',  ( 11.26737699260669778, 8.919714795263022467, -17.22149591130980184 ) ) ;
#17209 = EDGE_CURVE ( 'NONE', #30129, #27390, #1514, .T. ) ;
#17210 = CARTESIAN_POINT ( 'NONE',  ( 12.86846089198198584, 5.826474397738612865, -17.89591831848172276 ) ) ;
#17211 = EDGE_CURVE ( 'NONE', #22328, #23642, #24856, .T. ) ;
#17212 = CARTESIAN_POINT ( 'NONE',  ( 24.38930386813997586, -0.5518329404549096040, -18.38842912410832753 ) ) ;
#17213 = DIRECTION ( 'NONE',  ( 0.5877852522924731371, 1.586114251531760728E-16, -0.8090169943749474513 ) ) ;
#17214 = CARTESIAN_POINT ( 'NONE',  ( 141.1922820468854241, -10.00000000000000533, -4.936203717676158398 ) ) ;
#17215 = EDGE_CURVE ( 'NONE', #17767, #846, #22568, .T. ) ;
#17216 = LINE ( 'NONE', #17660, #4030 ) ;
#17217 = ORIENTED_EDGE ( 'NONE', *, *, #9626, .F. ) ;
#17218 = CARTESIAN_POINT ( 'NONE',  ( 167.0152310637605240, -4.999999999999972466, -1.854241549900776098E-14 ) ) ;
#17219 = DIRECTION ( 'NONE',  ( -0.9510565162951536422, -2.566386769018988816E-16, -0.3090169943749472292 ) ) ;
#17220 = CARTESIAN_POINT ( 'NONE',  ( 161.1922820468853104, -1.999999999999973577, -2.083034168790677043 ) ) ;
#17221 = EDGE_LOOP ( 'NONE', ( #2188, #23391, #25586, #13427, #29556 ) ) ;
#17222 = CARTESIAN_POINT ( 'NONE',  ( 133.6922820468854241, -10.00000000000000711, -17.92658477444275533 ) ) ;
#17223 = CARTESIAN_POINT ( 'NONE',  ( 137.0152310637606092, -10.00000000000000533, -15.61832212156129351 ) ) ;
#17224 = VECTOR ( 'NONE', #8167, 1000.000000000000000 ) ;
#17225 = CARTESIAN_POINT ( 'NONE',  ( 13.12595734265553205, 8.571888915454989544, -15.91003987120930319 ) ) ;
#17226 = CARTESIAN_POINT ( 'NONE',  ( 33.59450136257035524, -12.41883169790769692, -18.71738141962731561 ) ) ;
#17227 = ORIENTED_EDGE ( 'NONE', *, *, #6947, .T. ) ;
#17228 = CARTESIAN_POINT ( 'NONE',  ( 9.090073284221231731, 16.28436349189565391, -17.07021669716791124 ) ) ;
#17229 = CARTESIAN_POINT ( 'NONE',  ( 26.72181814967143509, -3.137724904577397389, -15.69709663067708050 ) ) ;
#17230 = CARTESIAN_POINT ( 'NONE',  ( 12.50804596317817463, 11.02747407808666580, -16.27511002087113567 ) ) ;
#17231 = FACE_BOUND ( 'NONE', #1475, .T. ) ;
#17232 = EDGE_CURVE ( 'NONE', #17842, #2137, #8652, .T. ) ;
#17233 = ORIENTED_EDGE ( 'NONE', *, *, #6410, .T. ) ;
#17234 = LINE ( 'NONE', #14928, #6264 ) ;
#17235 = CARTESIAN_POINT ( 'NONE',  ( 11.46877092736959014, 9.288109543210406827, -15.86260999805022820 ) ) ;
#17236 = CARTESIAN_POINT ( 'NONE',  ( 149.5152310637605240, -10.00000000000000178, -2.627941064794695691 ) ) ;
#17237 = ORIENTED_EDGE ( 'NONE', *, *, #487, .F. ) ;
#17238 = DIRECTION ( 'NONE',  ( -1.000000000000000000, 0.000000000000000000, -0.000000000000000000 ) ) ;
#17239 = ORIENTED_EDGE ( 'NONE', *, *, #3645, .T. ) ;
#17240 = CARTESIAN_POINT ( 'NONE',  ( 12.03309083968702886, 9.293808706017943067, -16.68917936036902105 ) ) ;
#17241 = ORIENTED_EDGE ( 'NONE', *, *, #2859, .F. ) ;
#17242 = CARTESIAN_POINT ( 'NONE',  ( 17.83966564144121136, 6.109271821037239647, -21.09843361817607388 ) ) ;
#17243 = CARTESIAN_POINT ( 'NONE',  ( 13.44640266258695327, 6.638963897028184569, -16.15403403936744198 ) ) ;
#17244 = ADVANCED_FACE ( 'NONE', ( #15675 ), #25009, .T. ) ;
#17245 = DIRECTION ( 'NONE',  ( 1.000000000000000000, 0.000000000000000000, -0.000000000000000000 ) ) ;
#17246 = EDGE_CURVE ( 'NONE', #29174, #11438, #1964, .T. ) ;
#17247 = ORIENTED_EDGE ( 'NONE', *, *, #9834, .F. ) ;
#17248 = EDGE_CURVE ( 'NONE', #17495, #14294, #11390, .T. ) ;
#17249 = ADVANCED_FACE ( 'NONE', ( #28229 ), #6682, .T. ) ;
#17250 = CARTESIAN_POINT ( 'NONE',  ( 36.54859195715578579, -22.18450706271777406, -18.40832622446962930 ) ) ;
#17251 = SHAPE_DEFINITION_REPRESENTATION ( #19567, #11460 ) ;
#17252 = CARTESIAN_POINT ( 'NONE',  ( 17.63088349262504551, 4.212901655933308120, -18.95607689789294170 ) ) ;
#17253 = CARTESIAN_POINT ( 'NONE',  ( 17.32873655921053313, 10.26331207550778579, -16.20725374984683143 ) ) ;
#17254 = CARTESIAN_POINT ( 'NONE',  ( 172.0152310637603819, -1.999999999999970912, -0.06116980274991495881 ) ) ;
#17255 = DIRECTION ( 'NONE',  ( -1.110223024625156540E-16, 0.000000000000000000, -1.000000000000000000 ) ) ;
#17256 = CARTESIAN_POINT ( 'NONE',  ( 169.7287565553229456, -1.999999999999970024, -25.16025403784440329 ) ) ;
#17257 = CYLINDRICAL_SURFACE ( 'NONE', #22354, 5.000000000000000888 ) ;
#17258 = LINE ( 'NONE', #7949, #29246 ) ;
#17259 = CARTESIAN_POINT ( 'NONE',  ( 173.6922820468853388, -1.999999999999970468, -23.73366926340167282 ) ) ;
#17260 = VECTOR ( 'NONE', #8172, 1000.000000000000000 ) ;
#17261 = CARTESIAN_POINT ( 'NONE',  ( 12.27679999902766284, 9.495116139066881900, -15.31073721177884650 ) ) ;
#17262 = CARTESIAN_POINT ( 'NONE',  ( -4.000000000000008882, 6.928203230275508773, 0.000000000000000000 ) ) ;
#17263 = ORIENTED_EDGE ( 'NONE', *, *, #8325, .F. ) ;
#17264 = CARTESIAN_POINT ( 'NONE',  ( 13.06581296851301310, -5.000000000000014211, 40.21243747300340488 ) ) ;
#17265 = ORIENTED_EDGE ( 'NONE', *, *, #7571, .F. ) ;
#17266 = CARTESIAN_POINT ( 'NONE',  ( 12.13006862794127017, 8.527244997094612700, -15.41586291625151972 ) ) ;
#17267 = ORIENTED_EDGE ( 'NONE', *, *, #5505, .T. ) ;
#17268 = CARTESIAN_POINT ( 'NONE',  ( 10.68417091768239047, 8.977850322645869241, -16.40447401652228621 ) ) ;
#17269 = DIRECTION ( 'NONE',  ( -0.9510565162951536422, -2.566386769018988816E-16, -0.3090169943749472292 ) ) ;
#17270 = VECTOR ( 'NONE', #27857, 1000.000000000000000 ) ;
#17271 = DIRECTION ( 'NONE',  ( -1.000000000000000000, 0.000000000000000000, 0.000000000000000000 ) ) ;
#17272 = B_SPLINE_CURVE_WITH_KNOTS ( 'NONE', 3,
 ( #2621, #7189, #19079, #25808, #4890, #2325 ),
 .UNSPECIFIED., .F., .F.,
 ( 4, 2, 4 ),
 ( 0.002336974151641511756, 0.003500975885716454961, 0.004664977619791398598 ),
 .UNSPECIFIED. ) ;
#17273 = DIRECTION ( 'NONE',  ( -0.9510565162951536422, -2.566386769018988816E-16, -0.3090169943749472292 ) ) ;
#17274 = ORIENTED_EDGE ( 'NONE', *, *, #24186, .T. ) ;
#17275 = CARTESIAN_POINT ( 'NONE',  ( 12.83210864641033844, 9.541281304504437344, -16.14109870176968897 ) ) ;
#17276 = CARTESIAN_POINT ( 'NONE',  ( 34.56382110058589774, -12.26799042007339757, -18.94768870749412315 ) ) ;
#17277 = CARTESIAN_POINT ( 'NONE',  ( 19.25048709941964376, 7.441878894999256921, -18.84525011105569803 ) ) ;
#17278 = ORIENTED_EDGE ( 'NONE', *, *, #27935, .F. ) ;
#17279 = EDGE_CURVE ( 'NONE', #15139, #15020, #26708, .T. ) ;
#17280 = LINE ( 'NONE', #12849, #8170 ) ;
#17281 = CARTESIAN_POINT ( 'NONE',  ( 19.85388831290292799, 7.668379621071204078, -15.62993620635094061 ) ) ;
#17282 = ADVANCED_FACE ( 'NONE', ( #25444 ), #2118, .T. ) ;
#17283 = DIRECTION ( 'NONE',  ( -0.8090169943749474513, -2.183098979609982436E-16, -0.5877852522924731371 ) ) ;
#17284 = ADVANCED_FACE ( 'NONE', ( #2416 ), #18572, .T. ) ;
#17285 = CARTESIAN_POINT ( 'NONE',  ( 0.000000000000000000, 0.000000000000000000, 15.00000000000000000 ) ) ;
#17286 = FILL_AREA_STYLE ('',( #19573 ) ) ;
#17287 = CARTESIAN_POINT ( 'NONE',  ( 26.68443370873975340, -2.140902173977853540, -15.79004130932784555 ) ) ;
#17288 = CARTESIAN_POINT ( 'NONE',  ( 17.82019932507133930, 1.781282266713458240, -14.47200660618688417 ) ) ;
#17289 = CIRCLE ( 'NONE', #20206, 4.000000000000000000 ) ;
#17290 = ORIENTED_EDGE ( 'NONE', *, *, #16054, .F. ) ;
#17291 = ORIENTED_EDGE ( 'NONE', *, *, #26650, .F. ) ;
#17292 = DIRECTION ( 'NONE',  ( 0.3090169943749475623, 8.338696094058001131E-17, 0.9510565162951536422 ) ) ;
#17293 = CARTESIAN_POINT ( 'NONE',  ( 16.95959666478115224, -5.000000000000013323, -52.19627145232931298 ) ) ;
#17294 = CARTESIAN_POINT ( 'NONE',  ( -6.686525924292791245, 5.377136764700170879, -4.683279549040157086 ) ) ;
#17295 = CARTESIAN_POINT ( 'NONE',  ( -7.999999999999998224, -0.7805016046291067822, -5.000000000000001776 ) ) ;
#17296 = PLANE ( 'NONE',  #5597 ) ;
#17297 = CARTESIAN_POINT ( 'NONE',  ( 11.43229926783177497, 9.455373222906182207, -15.87769231223556332 ) ) ;
#17298 = CARTESIAN_POINT ( 'NONE',  ( 27.33932411720343936, -8.205422078888220838, -18.29166945089792407 ) ) ;
#17299 = CARTESIAN_POINT ( 'NONE',  ( 22.33774198005919587, -7.088069534354142220, -17.87445411435389886 ) ) ;
#17300 = ORIENTED_EDGE ( 'NONE', *, *, #680, .F. ) ;
#17301 = CARTESIAN_POINT ( 'NONE',  ( 134.5152310637605808, -4.999999999999980460, -19.94844914048349338 ) ) ;
#17302 = CARTESIAN_POINT ( 'NONE',  ( 157.0152310637604671, -10.00000000000000000, -8.721423840594312082 ) ) ;
#17303 = CARTESIAN_POINT ( 'NONE',  ( -0.3263565795980836737, 4.430380094434250182, -0.2484800633750045007 ) ) ;
#17304 = DIRECTION ( 'NONE',  ( -1.110223024625156540E-16, 0.000000000000000000, -1.000000000000000000 ) ) ;
#17305 = VECTOR ( 'NONE', #6728, 1000.000000000000000 ) ;
#17306 = FACE_OUTER_BOUND ( 'NONE', #17722, .T. ) ;
#17307 = DIRECTION ( 'NONE',  ( 0.3090169943749472292, 8.338696094057992503E-17, -0.9510565162951536422 ) ) ;
#17308 = CARTESIAN_POINT ( 'NONE',  ( 15.44629794785920218, 3.545610805586186132, -16.71614555938632307 ) ) ;
#17309 = EDGE_LOOP ( 'NONE', ( #14957, #15811, #14892, #25642 ) ) ;
#17310 = FACE_OUTER_BOUND ( 'NONE', #12803, .T. ) ;
#17311 = CARTESIAN_POINT ( 'NONE',  ( 12.27694278248960558, 9.494486990809335225, -15.31067620760345527 ) ) ;
#17312 = CARTESIAN_POINT ( 'NONE',  ( 32.12153525177792091, -10.97127362787143312, -16.88978156643115724 ) ) ;
#17313 = DIRECTION ( 'NONE',  ( -1.000000000000000000, -4.440892098500622217E-16, 0.000000000000000000 ) ) ;
#17314 = CARTESIAN_POINT ( 'NONE',  ( 25.57370974413349884, -0.4222200280313516685, -16.88676729435558599 ) ) ;
#17315 = CARTESIAN_POINT ( 'NONE',  ( 159.5152310637605240, -4.999999999999974243, -30.37205893520531319 ) ) ;
#17316 = CARTESIAN_POINT ( 'NONE',  ( 21.20591713499851849, 2.664298913801621538, -19.97344039048299891 ) ) ;
#17317 = EDGE_LOOP ( 'NONE', ( #5108, #20652, #10323, #9649 ) ) ;
#17318 = ADVANCED_FACE ( 'NONE', ( #23301 ), #23459, .T. ) ;
#17319 = CARTESIAN_POINT ( 'NONE',  ( 35.54859390953724585, -22.18451583373416014, -16.94733705004010460 ) ) ;
#17320 =( LENGTH_UNIT ( ) NAMED_UNIT ( * ) SI_UNIT ( .MILLI., .METRE. ) );
#17321 = CARTESIAN_POINT ( 'NONE',  ( 25.21061150575720333, -3.342243121390650717, -18.67481654970342930 ) ) ;
#17322 = CARTESIAN_POINT ( 'NONE',  ( 25.18022790295009727, 0.7303485828293051485, -17.76052596840512621 ) ) ;
#17323 = CARTESIAN_POINT ( 'NONE',  ( 26.38113052396219516, -11.59678093645141672, -17.84452879788985769 ) ) ;
#17324 = VECTOR ( 'NONE', #15043, 1000.000000000000000 ) ;
#17325 = ORIENTED_EDGE ( 'NONE', *, *, #8071, .F. ) ;
#17326 = AXIS2_PLACEMENT_3D ( 'NONE', #18236, #27594, #17930 ) ;
#17327 = CARTESIAN_POINT ( 'NONE',  ( 136.1922820468854241, -10.00000000000000533, -13.59645775552055547 ) ) ;
#17328 = CARTESIAN_POINT ( 'NONE',  ( 129.5152310637605808, -10.00000000000000888, -11.28819510263909187 ) ) ;
#17329 = LINE ( 'NONE', #5750, #12543 ) ;
#17330 = CARTESIAN_POINT ( 'NONE',  ( 136.1922820468854241, -10.00000000000000533, -10.74328820663507322 ) ) ;
#17331 = CARTESIAN_POINT ( 'NONE',  ( 15.84550288711180777, 10.06862660282224731, -14.00251831694083826 ) ) ;
#17332 = EDGE_CURVE ( 'NONE', #7083, #29062, #16582, .T. ) ;
#17333 = CARTESIAN_POINT ( 'NONE',  ( 34.63381380623899020, -13.58242311684542081, -20.01117170570581649 ) ) ;
#17334 = CARTESIAN_POINT ( 'NONE',  ( 11.39177520167864266, 9.641221755901229429, -15.89445043910815336 ) ) ;
#17335 = AXIS2_PLACEMENT_3D ( 'NONE', #4696, #282, #28086 ) ;
#17336 = CARTESIAN_POINT ( 'NONE',  ( 63.44486372867152824, -29.99999999999998934, -17.99999999999998934 ) ) ;
#17337 = DIRECTION ( 'NONE',  ( 2.207829878515935943E-16, 1.000000000000000000, 0.000000000000000000 ) ) ;
#17338 = CARTESIAN_POINT ( 'NONE',  ( 13.14084490070201738, 8.578467993704791184, -15.89817422466314945 ) ) ;
#17339 = PLANE ( 'NONE',  #1966 ) ;
#17340 = DIRECTION ( 'NONE',  ( 1.000000000000000000, 4.440892098500623203E-16, 0.000000000000000000 ) ) ;
#17341 = ORIENTED_EDGE ( 'NONE', *, *, #16024, .T. ) ;
#17342 = AXIS2_PLACEMENT_3D ( 'NONE', #29772, #17937, #30062 ) ;
#17343 = CARTESIAN_POINT ( 'NONE',  ( 174.5152310637603819, -4.999999999999970690, -1.937508276747661261E-14 ) ) ;
#17344 = LINE ( 'NONE', #10325, #542 ) ;
#17345 = CONICAL_SURFACE ( 'NONE', #22234, 4.513000000000000789, 0.2131563744996338439 ) ;
#17346 = CARTESIAN_POINT ( 'NONE',  ( 163.6922820468853104, -9.999999999999998224, -9.266330736598359152 ) ) ;
#17347 = VERTEX_POINT ( 'NONE', #7280 ) ;
#17348 = ORIENTED_EDGE ( 'NONE', *, *, #13486, .T. ) ;
#17349 = CARTESIAN_POINT ( 'NONE',  ( 11.22197018571015725, 9.100068217651248403, -17.24240020332717904 ) ) ;
#17350 = EDGE_LOOP ( 'NONE', ( #23375, #2690, #726, #22091 ) ) ;
#17351 = VECTOR ( 'NONE', #23119, 1000.000000000000000 ) ;
#17352 = CARTESIAN_POINT ( 'NONE',  ( 13.03988341252192917, 6.056598437983586436, -18.79510648546616736 ) ) ;
#17353 = CARTESIAN_POINT ( 'NONE',  ( 26.46413748225140594, -13.10274310649288942, -15.24000415025259692 ) ) ;
#17354 = CARTESIAN_POINT ( 'NONE',  ( 139.5152310637606092, -1.999999999999978684, -11.28819510263909542 ) ) ;
#17355 = CARTESIAN_POINT ( 'NONE',  ( 131.1922820468854241, -1.999999999999981792, -2.083034168790677043 ) ) ;
#17356 = CARTESIAN_POINT ( 'NONE',  ( 149.7287565553230024, -10.00000000000000178, -16.50000000000000355 ) ) ;
#17357 = AXIS2_PLACEMENT_3D ( 'NONE', #22355, #15471, #3891 ) ;
#17358 = VERTEX_POINT ( 'NONE', #9547 ) ;
#17359 = CARTESIAN_POINT ( 'NONE',  ( 139.5152310637605808, -10.00000000000000533, -2.627941064794695691 ) ) ;
#17360 = LINE ( 'NONE', #10341, #28777 ) ;
#17361 = VECTOR ( 'NONE', #4146, 1000.000000000000000 ) ;
#17362 = DIRECTION ( 'NONE',  ( -2.698458740408365879E-16, 1.000000000000000000, 0.000000000000000000 ) ) ;
#17363 = CARTESIAN_POINT ( 'NONE',  ( 10.55189716074911921, 7.593251366112848899, 4.999999999999998224 ) ) ;
#17364 = CARTESIAN_POINT ( 'NONE',  ( 13.12278719711289732, 8.570488965836000617, -15.91256645732111430 ) ) ;
#17365 = EDGE_CURVE ( 'NONE', #25802, #19921, #25748, .T. ) ;
#17366 = EDGE_CURVE ( 'NONE', #23763, #22699, #4240, .T. ) ;
#17367 = CARTESIAN_POINT ( 'NONE',  ( 35.16668739017224965, -20.46881214373840763, -20.22602438870426766 ) ) ;
#17368 = ORIENTED_EDGE ( 'NONE', *, *, #24957, .F. ) ;
#17369 = CARTESIAN_POINT ( 'NONE',  ( 9.113211330545484046, 16.17824946203780456, -17.05444305708079966 ) ) ;
#17371 = ADVANCED_FACE ( 'NONE', ( #22863 ), #30233, .T. ) ;
#17370 = PRODUCT_DEFINITION_SHAPE ( 'NONE', 'NONE',  #30265 ) ;
#17372 = ADVANCED_FACE ( 'NONE', ( #27921, #8945, #18262 ), #15975, .T. ) ;
#17373 = CARTESIAN_POINT ( 'NONE',  ( 23.29338531092689735, -7.078548041224526521, -17.51562821661096336 ) ) ;
#17374 = CARTESIAN_POINT ( 'NONE',  ( 12.83388176712078810, 9.535019011556107316, -16.14022287234750408 ) ) ;
#17375 = FACE_BOUND ( 'NONE', #14325, .T. ) ;
#17376 = ORIENTED_EDGE ( 'NONE', *, *, #2681, .F. ) ;
#17377 = CARTESIAN_POINT ( 'NONE',  ( 154.5152310637605240, -10.00000000000000000, -11.28819510263909542 ) ) ;
#17378 = VECTOR ( 'NONE', #28938, 1000.000000000000000 ) ;
#17379 = CARTESIAN_POINT ( 'NONE',  ( 12.47535353872619446, 8.560407331872438519, -15.14977315560688176 ) ) ;
#17380 = LINE ( 'NONE', #19666, #20816 ) ;
#17381 = ORIENTED_EDGE ( 'NONE', *, *, #20705, .T. ) ;
#17382 = FACE_OUTER_BOUND ( 'NONE', #14371, .T. ) ;
#17383 = EDGE_LOOP ( 'NONE', ( #1708, #8275, #18981, #21119 ) ) ;
#17384 = CARTESIAN_POINT ( 'NONE',  ( 12.11773132146483789, 9.045882004348337446, -16.64348121447567053 ) ) ;
#17385 = ORIENTED_EDGE ( 'NONE', *, *, #6987, .F. ) ;
#17386 = VECTOR ( 'NONE', #27354, 1000.000000000000000 ) ;
#17387 = CARTESIAN_POINT ( 'NONE',  ( 19.44145409300831417, 9.016062086884520710, -15.75081756649476894 ) ) ;
#17388 = CARTESIAN_POINT ( 'NONE',  ( 18.58771872311928774, 0.01515834859250781048, -13.77226461354315035 ) ) ;
#17389 = VECTOR ( 'NONE', #30248, 1000.000000000000000 ) ;
#17390 = LINE ( 'NONE', #24427, #1396 ) ;
#17391 = ORIENTED_EDGE ( 'NONE', *, *, #18418, .F. ) ;
#17392 = CARTESIAN_POINT ( 'NONE',  ( 36.35800453371076202, -21.32829872614925648, -20.07395605779921155 ) ) ;
#17393 = CARTESIAN_POINT ( 'NONE',  ( 14.39533340154967433, 6.572929804808670617, -18.54476805420031837 ) ) ;
#17394 = VERTEX_POINT ( 'NONE', #20696 ) ;
#17395 = DIRECTION ( 'NONE',  ( 0.3090169943749475623, 8.338696094058001131E-17, 0.9510565162951536422 ) ) ;
#17396 = FACE_BOUND ( 'NONE', #1229, .T. ) ;
#17397 = AXIS2_PLACEMENT_3D ( 'NONE', #12386, #5687, #12840 ) ;
#17398 = DIRECTION ( 'NONE',  ( 0.000000000000000000, 0.000000000000000000, 1.000000000000000000 ) ) ;
#17399 = ADVANCED_FACE ( 'NONE', ( #27773 ), #2263, .T. ) ;
#17400 = CARTESIAN_POINT ( 'NONE',  ( 32.62126879184269512, -11.04717877266006987, -18.30218954475424908 ) ) ;
#17401 = LINE ( 'NONE', #10533, #10682 ) ;
#17402 = AXIS2_PLACEMENT_3D ( 'NONE', #26310, #7236, #25698 ) ;
#17403 = ORIENTED_EDGE ( 'NONE', *, *, #6915, .T. ) ;
#17404 = EDGE_CURVE ( 'NONE', #26448, #12211, #9395, .T. ) ;
#17405 = CARTESIAN_POINT ( 'NONE',  ( 14.57230909446801270, -5.000000000000013323, -44.84895579867345106 ) ) ;
#17406 = PRODUCT_DEFINITION_CONTEXT ( 'detailed design', #2103, 'design' ) ;
#17407 = ADVANCED_FACE ( 'NONE', ( #26512 ), #5288, .T. ) ;
#17408 = CARTESIAN_POINT ( 'NONE',  ( 11.95275185645256322, 10.98126796543430572, -15.44474055479659569 ) ) ;
#17409 = CARTESIAN_POINT ( 'NONE',  ( 151.1922820468853956, -10.00000000000000178, -13.59645775552055902 ) ) ;
#17410 = LINE ( 'NONE', #21692, #18300 ) ;
#17411 = EDGE_LOOP ( 'NONE', ( #4590, #1701, #4284, #17792 ) ) ;
#17412 = CARTESIAN_POINT ( 'NONE',  ( 12.49271550807400999, 8.567542729147559655, -15.13597632865050535 ) ) ;
#17413 = ORIENTED_EDGE ( 'NONE', *, *, #26567, .F. ) ;
#17414 = CARTESIAN_POINT ( 'NONE',  ( 11.57911078346310774, 7.697743364462890980, -15.81898674067912225 ) ) ;
#17415 = CARTESIAN_POINT ( 'NONE',  ( 169.5152310637604955, -1.999999999999970468, -19.94844914048349693 ) ) ;
#17416 = CARTESIAN_POINT ( 'NONE',  ( 10.55189716074911921, 7.593251366112849787, 9.999999999999998224 ) ) ;
#17417 = ORIENTED_EDGE ( 'NONE', *, *, #27590, .F. ) ;
#17418 = DIRECTION ( 'NONE',  ( 2.908569913943825554E-16, -1.000000000000000000, 0.000000000000000000 ) ) ;
#17419 = ORIENTED_EDGE ( 'NONE', *, *, #16733, .F. ) ;
#17420 = CARTESIAN_POINT ( 'NONE',  ( 12.83866652039362855, 9.525916288823983891, -16.13726486007240624 ) ) ;
#17421 = ORIENTED_EDGE ( 'NONE', *, *, #27590, .T. ) ;
#17422 = CARTESIAN_POINT ( 'NONE',  ( 36.10807049912983757, -19.20547750251314767, -19.41448258861096932 ) ) ;
#17423 = CARTESIAN_POINT ( 'NONE',  ( 18.76632379254337835, 6.868107169226369102, -19.55161205380106892 ) ) ;
#17424 = ORIENTED_EDGE ( 'NONE', *, *, #16415, .T. ) ;
#17425 = AXIS2_PLACEMENT_3D ( 'NONE', #16186, #14486, #11750 ) ;
#17426 = CARTESIAN_POINT ( 'NONE',  ( 132.0152310637605524, -4.999999999999982236, -34.70218595412750773 ) ) ;
#17427 = CARTESIAN_POINT ( 'NONE',  ( 32.57950401048368150, -10.91418750421072659, -13.94906786461360504 ) ) ;
#17428 = CARTESIAN_POINT ( 'NONE',  ( 158.6922820468853956, -1.999999999999974465, -23.73366926340167282 ) ) ;
#17429 = LINE ( 'NONE', #30003, #1103 ) ;
#17430 = CARTESIAN_POINT ( 'NONE',  ( 19.55718041265476970, -1.390565517676688900, -17.79492730709450754 ) ) ;
#17431 = CARTESIAN_POINT ( 'NONE',  ( 20.13453040791782911, -1.388291987844697317, -13.01173725324373009 ) ) ;
#17432 = VERTEX_POINT ( 'NONE', #19025 ) ;
#17433 = ORIENTED_EDGE ( 'NONE', *, *, #23052, .T. ) ;
#17434 = ORIENTED_EDGE ( 'NONE', *, *, #21639, .F. ) ;
#17435 = DIRECTION ( 'NONE',  ( 0.5877852522924731371, 1.586114251531760728E-16, -0.8090169943749474513 ) ) ;
#17436 = CARTESIAN_POINT ( 'NONE',  ( 6.938893903907228378E-15, 60.00000000000000711, -1.040834085586084257E-14 ) ) ;
#17437 = LINE ( 'NONE', #20038, #18194 ) ;
#17438 = CARTESIAN_POINT ( 'NONE',  ( 142.0152310637606092, -1.999999999999978018, -32.93883019725009120 ) ) ;
#17439 = CARTESIAN_POINT ( 'NONE',  ( 157.0152310637604955, -10.00000000000000000, -6.958068083716895558 ) ) ;
#17440 = EDGE_CURVE ( 'NONE', #13196, #3218, #23608, .T. ) ;
#17441 = EDGE_CURVE ( 'NONE', #24401, #25168, #28380, .T. ) ;
#17442 = CARTESIAN_POINT ( 'NONE',  ( 141.1922820468854525, -10.00000000000000533, -28.06379628232387446 ) ) ;
#17443 = VECTOR ( 'NONE', #11217, 1000.000000000000000 ) ;
#17444 = ADVANCED_FACE ( 'NONE', ( #9699 ), #709, .F. ) ;
#17445 = CARTESIAN_POINT ( 'NONE',  ( 11.44040408106239326, 9.418203516307107392, -15.87434068686103394 ) ) ;
#17446 = EDGE_CURVE ( 'NONE', #23239, #16280, #7436, .T. ) ;
#17447 = CARTESIAN_POINT ( 'NONE',  ( 16.77165338796101324, 10.12286561294300569, -15.51291369241808304 ) ) ;
#17448 = CARTESIAN_POINT ( 'NONE',  ( 26.69342817538273138, -7.978421288772274522, -19.59580293194042966 ) ) ;
#17449 = ORIENTED_EDGE ( 'NONE', *, *, #4362, .T. ) ;
#17450 = CARTESIAN_POINT ( 'NONE',  ( 137.0152310637605808, -10.00000000000000533, 1.702185954127501066 ) ) ;
#17451 = AXIS2_PLACEMENT_3D ( 'NONE', #11419, #4120, #20725 ) ;
#17452 = DIRECTION ( 'NONE',  ( 1.000000000000000000, 2.698458740408365879E-16, -1.110223024625156540E-16 ) ) ;
#17453 = PLANE ( 'NONE',  #2884 ) ;
#17454 = CARTESIAN_POINT ( 'NONE',  ( 138.6922820468854525, -1.999999999999979128, -32.39392330124607611 ) ) ;
#17455 = LINE ( 'NONE', #14403, #10252 ) ;
#17456 = DIRECTION ( 'NONE',  ( -0.9510565162951536422, 0.000000000000000000, -0.3090169943749472292 ) ) ;
#17457 = CARTESIAN_POINT ( 'NONE',  ( 19.18841159021359033, -2.222386543571284179, -18.22349448661670834 ) ) ;
#17458 = ORIENTED_EDGE ( 'NONE', *, *, #7943, .T. ) ;
#17459 = DIRECTION ( 'NONE',  ( 0.9510565162951535312, 2.566386769018988816E-16, -0.3090169943749475623 ) ) ;
#17460 = CARTESIAN_POINT ( 'NONE',  ( 12.27434273475605409, 9.502313893772186049, -15.31206391052669602 ) ) ;
#17461 = DIRECTION ( 'NONE',  ( 0.5877852522924731371, 0.000000000000000000, 0.8090169943749474513 ) ) ;
#17462 = DIRECTION ( 'NONE',  ( 0.000000000000000000, 0.000000000000000000, -1.000000000000000000 ) ) ;
#17463 = CARTESIAN_POINT ( 'NONE',  ( 19.02541433733466647, 1.263421280649871248, -13.57496312174407826 ) ) ;
#17464 = DIRECTION ( 'NONE',  ( 0.000000000000000000, 0.000000000000000000, 1.000000000000000000 ) ) ;
#17465 = ADVANCED_BREP_SHAPE_REPRESENTATION ( '', ( #11247, #13190 ), #21991 ) ;
#17466 = CARTESIAN_POINT ( 'NONE',  ( 20.44834407054411685, 8.573499863981592028, -15.78670165415130100 ) ) ;
#17467 = ORIENTED_EDGE ( 'NONE', *, *, #2497, .T. ) ;
#17468 = CARTESIAN_POINT ( 'NONE',  ( 12.74999999999999822, -1.387778780781445676E-16, 5.000000000000000888 ) ) ;
#17469 = CARTESIAN_POINT ( 'NONE',  ( 23.62051642037636157, -5.854316150849339984, -13.42181569741374503 ) ) ;
#17470 = CARTESIAN_POINT ( 'NONE',  ( 27.64697528205969590, -2.889103667904926898, -18.32829528246118755 ) ) ;
#17471 = EDGE_LOOP ( 'NONE', ( #23740, #11127, #27670, #2487, #20789 ) ) ;
#17472 = CARTESIAN_POINT ( 'NONE',  ( 27.01132674553606350, -11.00696853675122711, -18.49859303458091730 ) ) ;
#17473 = AXIS2_PLACEMENT_3D ( 'NONE', #19135, #9824, #12265 ) ;
#17474 = VERTEX_POINT ( 'NONE', #571 ) ;
#17475 = CARTESIAN_POINT ( 'NONE',  ( 157.2287565553229172, -10.00000000000000178, -3.509618943233403510 ) ) ;
#17476 = VECTOR ( 'NONE', #18901, 1000.000000000000000 ) ;
#17477 = ORIENTED_EDGE ( 'NONE', *, *, #16869, .T. ) ;
#17478 = ORIENTED_EDGE ( 'NONE', *, *, #25396, .F. ) ;
#17479 = LINE ( 'NONE', #710, #9735 ) ;
#17480 = DIRECTION ( 'NONE',  ( -2.908569913943825554E-16, 1.000000000000000000, -6.826925868028084042E-18 ) ) ;
#17481 = EDGE_CURVE ( 'NONE', #4723, #27841, #22089, .T. ) ;
#17482 = LINE ( 'NONE', #26832, #6075 ) ;
#17483 = CARTESIAN_POINT ( 'NONE',  ( 8.000000000000014211, -3.098204225878182783, -0.3157906771918849720 ) ) ;
#17484 = EDGE_CURVE ( 'NONE', #16280, #3964, #7877, .T. ) ;
#17485 = CARTESIAN_POINT ( 'NONE',  ( 25.76085037594245719, -3.206535967183471669, -15.98314152415894540 ) ) ;
#17486 = CARTESIAN_POINT ( 'NONE',  ( 149.5152310637605808, -1.999999999999975353, -30.37205893520531319 ) ) ;
#17487 = CARTESIAN_POINT ( 'NONE',  ( 36.52322468491136220, -22.07054534594105988, -19.04503427665075321 ) ) ;
#17488 = CARTESIAN_POINT ( 'NONE',  ( 9.916336358462064737, 16.40777236560037622, -16.50459729666445696 ) ) ;
#17489 = LINE ( 'NONE', #28684, #17101 ) ;
#17490 = CARTESIAN_POINT ( 'NONE',  ( 131.1922820468854241, -1.999999999999982236, -30.91696583120935671 ) ) ;
#17491 = CARTESIAN_POINT ( 'NONE',  ( 13.12489394565217005, 8.571418981294288031, -15.91088741739120671 ) ) ;
#17492 = DIRECTION ( 'NONE',  ( 1.000000000000000000, 0.000000000000000000, 0.000000000000000000 ) ) ;
#17493 = ORIENTED_EDGE ( 'NONE', *, *, #22205, .F. ) ;
#17494 = CARTESIAN_POINT ( 'NONE',  ( 154.5152310637605240, -4.999999999999975131, -11.28819510263909542 ) ) ;
#17495 = VERTEX_POINT ( 'NONE', #5443 ) ;
#17496 = VECTOR ( 'NONE', #197, 1000.000000000000000 ) ;
#17497 = CARTESIAN_POINT ( 'NONE',  ( 149.7287565553230309, -10.00000000000000178, -33.82050807568879947 ) ) ;
#17498 = CARTESIAN_POINT ( 'NONE',  ( 163.6922820468853104, -9.999999999999998224, -6.413161187712876909 ) ) ;
#17499 = CARTESIAN_POINT ( 'NONE',  ( 74.18800000000001660, 0.000000000000000000, 0.000000000000000000 ) ) ;
#17500 = ORIENTED_EDGE ( 'NONE', *, *, #28881, .T. ) ;
#17501 = EDGE_LOOP ( 'NONE', ( #6998, #22154, #26386, #4377, #3714, #1432 ) ) ;
#17502 = ORIENTED_EDGE ( 'NONE', *, *, #11041, .F. ) ;
#17503 = CARTESIAN_POINT ( 'NONE',  ( 8.944584764616054784, 16.95159238827779546, -17.91493351301869552 ) ) ;
#17504 = CARTESIAN_POINT ( 'NONE',  ( 13.09464261414706066, 5.717622835290344874, -15.96348941799783816 ) ) ;
#17505 = CARTESIAN_POINT ( 'NONE',  ( 28.96558774451377971, -5.053040458581501859, -15.93506438242870971 ) ) ;
#17506 = CARTESIAN_POINT ( 'NONE',  ( 175.7287565553229456, -4.999999999999970690, -33.50000000000000000 ) ) ;
#17507 = CARTESIAN_POINT ( 'NONE',  ( 157.0152310637605524, -9.999999999999998224, -34.70218595412750773 ) ) ;
#17508 = CARTESIAN_POINT ( 'NONE',  ( -4.683753385137379155E-14, -9.237604307034027684, -0.7145311798163362926 ) ) ;
#17509 = ADVANCED_FACE ( 'NONE', ( #9857 ), #17186, .T. ) ;
#17510 = ORIENTED_EDGE ( 'NONE', *, *, #23084, .T. ) ;
#17511 = LINE ( 'NONE', #24549, #21100 ) ;
#17512 = VERTEX_POINT ( 'NONE', #867 ) ;
#17513 = VECTOR ( 'NONE', #12341, 1000.000000000000000 ) ;
#17514 = DIRECTION ( 'NONE',  ( 1.000000000000000000, 0.000000000000000000, 0.000000000000000000 ) ) ;
#17515 = CARTESIAN_POINT ( 'NONE',  ( 153.6922820468853388, -4.999999999999976907, -17.92658477444275533 ) ) ;
#17516 = CARTESIAN_POINT ( 'NONE',  ( 149.5152310637605524, -10.00000000000000178, -11.28819510263909542 ) ) ;
#17517 = EDGE_CURVE ( 'NONE', #27580, #10204, #17033, .T. ) ;
#17518 = CARTESIAN_POINT ( 'NONE',  ( 13.12489394565217005, 8.571418981294288031, -15.91088741739120671 ) ) ;
#17519 = ORIENTED_EDGE ( 'NONE', *, *, #9721, .F. ) ;
#17520 = CARTESIAN_POINT ( 'NONE',  ( 35.54859390953724585, -22.18451583373416014, -18.19919658220850778 ) ) ;
#17521 = CARTESIAN_POINT ( 'NONE',  ( 10.40934825891211979, 10.23400028951819607, -16.51844484289298265 ) ) ;
#17522 = ORIENTED_EDGE ( 'NONE', *, *, #16517, .F. ) ;
#17523 = B_SPLINE_CURVE_WITH_KNOTS ( 'NONE', 3,
 ( #15186, #26833, #17483, #24518, #15335, #12037 ),
 .UNSPECIFIED., .F., .F.,
 ( 4, 2, 4 ),
 ( 0.008240550023493525833, 0.01057684187039405893, 0.01291313371729459203 ),
 .UNSPECIFIED. ) ;
#17524 = CARTESIAN_POINT ( 'NONE',  ( 24.66978787416869068, -0.3063955544261361963, -14.42797892638687784 ) ) ;
#17525 = CARTESIAN_POINT ( 'NONE',  ( 10.35864919943752405, 16.97212496474457311, -17.91550491156534974 ) ) ;
#17526 = FACE_BOUND ( 'NONE', #27940, .T. ) ;
#17527 = ORIENTED_EDGE ( 'NONE', *, *, #7405, .F. ) ;
#17528 = PLANE ( 'NONE',  #8553 ) ;
#17529 = CARTESIAN_POINT ( 'NONE',  ( 11.77869587587188249, 8.711114196793760200, -15.67004689359726299 ) ) ;
#17530 = CARTESIAN_POINT ( 'NONE',  ( 160.0000000000000284, -9.999999999999973355, -17.99999999999998934 ) ) ;
#17531 = VERTEX_POINT ( 'NONE', #21309 ) ;
#17532 = CARTESIAN_POINT ( 'NONE',  ( 133.6922820468854241, -10.00000000000000711, -9.266330736598357376 ) ) ;
#17533 = ORIENTED_EDGE ( 'NONE', *, *, #20617, .F. ) ;
#17534 = AXIS2_PLACEMENT_3D ( 'NONE', #18646, #16198, #2336 ) ;
#17535 = CARTESIAN_POINT ( 'NONE',  ( 13.10707286029108865, 8.563798077496334926, -15.92507172258792281 ) ) ;
#17536 = EDGE_LOOP ( 'NONE', ( #9492, #27914, #19618, #7115, #22777 ) ) ;
#17537 = VECTOR ( 'NONE', #11372, 1000.000000000000114 ) ;
#17538 = CARTESIAN_POINT ( 'NONE',  ( 18.23272808550097679, 0.7689261898593379163, -20.18852386690180367 ) ) ;
#17539 = CARTESIAN_POINT ( 'NONE',  ( 19.58395429099637752, 5.031901065175194532, -13.05446103591450147 ) ) ;
#17540 = VECTOR ( 'NONE', #25408, 1000.000000000000000 ) ;
#17541 = CARTESIAN_POINT ( 'NONE',  ( 156.1922820468854241, -4.999999999999975131, -28.06379628232387802 ) ) ;
#17542 = ORIENTED_EDGE ( 'NONE', *, *, #3281, .F. ) ;
#17543 = AXIS2_PLACEMENT_3D ( 'NONE', #11540, #16277, #6393 ) ;
#17544 = CARTESIAN_POINT ( 'NONE',  ( 36.54859390953724585, -22.18451583373416014, -17.99055332684694974 ) ) ;
#17545 = ITEM_DEFINED_TRANSFORMATION ( 'NONE', 'NONE', #6354,  #13190 ) ;
#17546 = EDGE_CURVE ( 'NONE', #21674, #21255, #3019, .T. ) ;
#17547 = ADVANCED_FACE ( 'NONE', ( #23764 ), #1027, .T. ) ;
#17548 = CARTESIAN_POINT ( 'NONE',  ( 16.09764958744793262, 8.143416238145906760, -19.84970969296679044 ) ) ;
#17549 = CARTESIAN_POINT ( 'NONE',  ( 171.1922820468853388, -1.999999999999970024, -19.40354224447947828 ) ) ;
#17550 = VECTOR ( 'NONE', #28359, 1000.000000000000000 ) ;
#17551 = FACE_OUTER_BOUND ( 'NONE', #23559, .T. ) ;
#17552 = AXIS2_PLACEMENT_3D ( 'NONE', #26339, #24050, #3149 ) ;
#17553 = ORIENTED_EDGE ( 'NONE', *, *, #4868, .F. ) ;
#17554 = EDGE_LOOP ( 'NONE', ( #26806, #22286, #6136, #24478 ) ) ;
#17555 = DIRECTION ( 'NONE',  ( -2.698458740408365879E-16, 1.000000000000000000, 0.000000000000000000 ) ) ;
#17556 = CARTESIAN_POINT ( 'NONE',  ( 32.74314609665832165, -11.10724048739539782, -18.62249297335446840 ) ) ;
#17557 = AXIS2_PLACEMENT_3D ( 'NONE', #17963, #27336, #29642 ) ;
#17558 = CARTESIAN_POINT ( 'NONE',  ( 166.1922820468853104, -1.999999999999972689, -4.936203717676158398 ) ) ;
#17559 = LINE ( 'NONE', #27226, #12437 ) ;
#17560 = CARTESIAN_POINT ( 'NONE',  ( 11.05541548581436118, 17.68942261459453036, -17.91440211708152574 ) ) ;
#17561 = CARTESIAN_POINT ( 'NONE',  ( 5.354491962338135735, -6.146186931204433712, -4.931901280394558107 ) ) ;
#17562 = EDGE_LOOP ( 'NONE', ( #9604, #16255, #25770, #13994, #20747, #20454 ) ) ;
#17563 = FACE_OUTER_BOUND ( 'NONE', #17205, .T. ) ;
#17564 = ORIENTED_EDGE ( 'NONE', *, *, #12252, .F. ) ;
#17565 = CARTESIAN_POINT ( 'NONE',  ( 11.03967536873724242, 8.192193740582544237, -16.19303379925286279 ) ) ;
#17566 = CARTESIAN_POINT ( 'NONE',  ( 175.7287565553229456, -9.999999999999994671, -4.785595155761523500 ) ) ;
#17567 = CARTESIAN_POINT ( 'NONE',  ( 146.1922820468854525, -1.999999999999977129, -22.25671179336496053 ) ) ;
#17568 = ORIENTED_EDGE ( 'NONE', *, *, #3915, .T. ) ;
#17569 = LINE ( 'NONE', #10707, #11998 ) ;
#17570 = ORIENTED_EDGE ( 'NONE', *, *, #1168, .F. ) ;
#17571 = CARTESIAN_POINT ( 'NONE',  ( 12.83257874964047929, 9.539242390270068483, -16.14089537112711525 ) ) ;
#17572 = VECTOR ( 'NONE', #26533, 1000.000000000000000 ) ;
#17573 = CARTESIAN_POINT ( 'NONE',  ( 34.64580997985590471, -12.63631557036062247, -18.97247631304233195 ) ) ;
#17574 = CARTESIAN_POINT ( 'NONE',  ( 21.94319337455657859, -4.318501116253552041, -18.82930321547734920 ) ) ;
#17575 = ORIENTED_EDGE ( 'NONE', *, *, #23600, .F. ) ;
#17576 = VERTEX_POINT ( 'NONE', #7723 ) ;
#17577 = DIRECTION ( 'NONE',  ( 1.000000000000000000, 2.698458740408365879E-16, -1.110223024625156540E-16 ) ) ;
#17578 = CARTESIAN_POINT ( 'NONE',  ( 18.68520274485960542, 10.62608585526774441, -17.78552708330943588 ) ) ;
#17579 = DIRECTION ( 'NONE',  ( -2.698458740408365879E-16, 1.000000000000000000, 0.000000000000000000 ) ) ;
#17580 = DIRECTION ( 'NONE',  ( -1.000000000000000000, -2.207829878515935943E-16, 0.000000000000000000 ) ) ;
#17581 = SHAPE_REPRESENTATION_RELATIONSHIP ( 'NONE' , 'NONE' ,  #18708, #18930 ) ;
#17582 = EDGE_CURVE ( 'NONE', #12464, #19711, #25906, .T. ) ;
#17583 = PRESENTATION_LAYER_ASSIGNMENT (  '', '', ( #14170 ) ) ;
#17584 = CARTESIAN_POINT ( 'NONE',  ( 21.55249387529322647, -4.041031698679099726, -14.19001464829599435 ) ) ;
#17585 = EDGE_CURVE ( 'NONE', #19419, #24258, #26208, .T. ) ;
#17586 = CARTESIAN_POINT ( 'NONE',  ( 17.18298215709098287, 1.908350159885260799, -18.42911670940388902 ) ) ;
#17587 = EDGE_CURVE ( 'NONE', #18177, #10339, #11355, .T. ) ;
#17588 = ORIENTED_EDGE ( 'NONE', *, *, #12554, .T. ) ;
#17589 = CARTESIAN_POINT ( 'NONE',  ( 133.6922820468854241, -1.999999999999980904, 2.247092850131519715 ) ) ;
#17590 = DIRECTION ( 'NONE',  ( 0.3090169943749475623, 8.338696094058001131E-17, 0.9510565162951536422 ) ) ;
#17591 = LINE ( 'NONE', #22487, #1166 ) ;
#17592 = VECTOR ( 'NONE', #20088, 1000.000000000000000 ) ;
#17593 = CARTESIAN_POINT ( 'NONE',  ( 152.2287565553230309, -10.00000000000000178, -29.49038105676660493 ) ) ;
#17594 = CARTESIAN_POINT ( 'NONE',  ( 13.54327048257564314, -5.000000000000014211, 41.68190060373459005 ) ) ;
#17595 = VECTOR ( 'NONE', #851, 999.9999999999998863 ) ;
#17596 = PLANE ( 'NONE',  #8525 ) ;
#17597 = CARTESIAN_POINT ( 'NONE',  ( 11.22146363488324283, 9.102391324313689580, -17.24260967991309101 ) ) ;
#17598 = CARTESIAN_POINT ( 'NONE',  ( 10.17605321708455257, 15.21667774575863419, -16.39719424528293246 ) ) ;
#17599 = CARTESIAN_POINT ( 'NONE',  ( 30.58006126958193249, -8.114715823802763239, -15.12008790671442426 ) ) ;
#17600 = VERTEX_POINT ( 'NONE', #19316 ) ;
#17601 = DIRECTION ( 'NONE',  ( 0.000000000000000000, 0.000000000000000000, -1.000000000000000000 ) ) ;
#17602 = CARTESIAN_POINT ( 'NONE',  ( 144.5152310637606092, -1.999999999999977129, -19.94844914048349693 ) ) ;
#17603 = DIRECTION ( 'NONE',  ( 1.000000000000000000, 0.000000000000000000, 0.000000000000000000 ) ) ;
#17604 = CARTESIAN_POINT ( 'NONE',  ( 131.1922820468854241, -10.00000000000000888, -13.59645775552055547 ) ) ;
#17605 = DIRECTION ( 'NONE',  ( -0.5877852522924731371, 0.000000000000000000, 0.8090169943749474513 ) ) ;
#17606 = SURFACE_STYLE_FILL_AREA ( #26646 ) ;
#17607 = CARTESIAN_POINT ( 'NONE',  ( 21.69765170278760280, -5.035756590920279940, -14.89200278627170881 ) ) ;
#17608 = ORIENTED_EDGE ( 'NONE', *, *, #24775, .F. ) ;
#17609 = CARTESIAN_POINT ( 'NONE',  ( 163.6922820468853388, -4.999999999999973355, -15.07341522555727664 ) ) ;
#17610 = CARTESIAN_POINT ( 'NONE',  ( 12.27690927615027583, 9.494639109526119114, -15.31069018153633721 ) ) ;
#17611 = LINE ( 'NONE', #26652, #323 ) ;
#17612 = PLANE ( 'NONE',  #29364 ) ;
#17613 = CARTESIAN_POINT ( 'NONE',  ( 26.85315702054868936, -3.432285194908070380, -17.01323758698984889 ) ) ;
#17614 = DIRECTION ( 'NONE',  ( -0.5877852522924731371, -1.586114251531760728E-16, -0.8090169943749474513 ) ) ;
#17615 = CARTESIAN_POINT ( 'NONE',  ( 17.78670086218314239, 4.747145650100266678, -21.23922340053293212 ) ) ;
#17616 = VERTEX_POINT ( 'NONE', #26365 ) ;
#17617 = DIRECTION ( 'NONE',  ( 0.000000000000000000, -2.775557561562890735E-17, 1.000000000000000000 ) ) ;
#17618 = SURFACE_STYLE_USAGE ( .BOTH. , #10147 ) ;
#17619 = CARTESIAN_POINT ( 'NONE',  ( 28.48873154519036888, -4.568419848414010609, -17.42663535687301035 ) ) ;
#17620 = CARTESIAN_POINT ( 'NONE',  ( 23.77355757633466382, -7.879698323813751237, -13.16654918938113283 ) ) ;
#17621 = EDGE_CURVE ( 'NONE', #1987, #4875, #14725, .T. ) ;
#17622 = EDGE_CURVE ( 'NONE', #7797, #25128, #12439, .T. ) ;
#17623 = ORIENTED_EDGE ( 'NONE', *, *, #11245, .T. ) ;
#17624 = EDGE_CURVE ( 'NONE', #11448, #28119, #13050, .T. ) ;
#17625 = ADVANCED_FACE ( 'NONE', ( #27295 ), #10765, .T. ) ;
#17626 = LINE ( 'NONE', #2376, #16586 ) ;
#17627 = VERTEX_POINT ( 'NONE', #24975 ) ;
#17628 = FACE_OUTER_BOUND ( 'NONE', #10648, .T. ) ;
#17629 = CARTESIAN_POINT ( 'NONE',  ( 175.7287565553229456, -4.999999999999970690, 3.500000000000003109 ) ) ;
#17630 = DIRECTION ( 'NONE',  ( 0.5877852522924731371, 1.586114251531760728E-16, 0.8090169943749474513 ) ) ;
#17631 = LINE ( 'NONE', #1324, #17260 ) ;
#17632 = AXIS2_PLACEMENT_3D ( 'NONE', #3974, #9124, #1855 ) ;
#17633 = FACE_BOUND ( 'NONE', #18471, .T. ) ;
#17634 = CARTESIAN_POINT ( 'NONE',  ( 23.80376867147650444, -3.845223433682474212, -14.48388124448521452 ) ) ;
#17635 = CARTESIAN_POINT ( 'NONE',  ( 16.94700227795405212, 10.49100606271714931, -14.51747230701220559 ) ) ;
#17636 = CARTESIAN_POINT ( 'NONE',  ( 34.83580697690636185, -15.48987143388560384, -21.11455094357481244 ) ) ;
#17637 = CARTESIAN_POINT ( 'NONE',  ( 120.6264357055466689, -4.999999999999984901, -87.64023554178400843 ) ) ;
#17638 = CARTESIAN_POINT ( 'NONE',  ( 10.43540724046455992, 14.02724713458965233, -16.28994223329847202 ) ) ;
#17639 = LINE ( 'NONE', #13218, #11255 ) ;
#17640 = CARTESIAN_POINT ( 'NONE',  ( 9.661883064511089358, 16.25482662032373327, -17.91571053624716470 ) ) ;
#17641 = DIRECTION ( 'NONE',  ( -0.8090169943749474513, -2.183098979609982436E-16, 0.5877852522924731371 ) ) ;
#17642 = FACE_OUTER_BOUND ( 'NONE', #27151, .T. ) ;
#17643 = CARTESIAN_POINT ( 'NONE',  ( 11.46877092736959014, 9.288109543210406827, -15.86260999805022820 ) ) ;
#17644 = ORIENTED_EDGE ( 'NONE', *, *, #612, .T. ) ;
#17645 = LINE ( 'NONE', #6215, #12450 ) ;
#17646 = CARTESIAN_POINT ( 'NONE',  ( 161.1922820468853672, -1.999999999999973133, -22.25671179336496053 ) ) ;
#17647 = VECTOR ( 'NONE', #2535, 1000.000000000000000 ) ;
#17648 = CARTESIAN_POINT ( 'NONE',  ( 174.7287565553229172, -1.999999999999968914, -25.16025403784440329 ) ) ;
#17649 = ORIENTED_EDGE ( 'NONE', *, *, #11031, .T. ) ;
#17650 = CARTESIAN_POINT ( 'NONE',  ( 8.944584683310379702, 16.95159276115599667, -17.98596209335946128 ) ) ;
#17651 = CARTESIAN_POINT ( 'NONE',  ( 31.38423252821215570, -10.20947814759437655, -16.80760986317607930 ) ) ;
#17652 = ORIENTED_EDGE ( 'NONE', *, *, #5676, .T. ) ;
#17653 = CARTESIAN_POINT ( 'NONE',  ( 25.97279949409942290, -11.71600155862194015, -18.85018042282848683 ) ) ;
#17654 = EDGE_CURVE ( 'NONE', #26426, #2723, #17918, .T. ) ;
#17655 = CARTESIAN_POINT ( 'NONE',  ( 27.85014272824177795, -5.137623357037004013, -13.74226875356335320 ) ) ;
#17656 = CARTESIAN_POINT ( 'NONE',  ( 172.7287565553229456, -3.999999999999989786, -41.50000000000000711 ) ) ;
#17657 = PLANE ( 'NONE',  #24315 ) ;
#17658 = AXIS2_PLACEMENT_3D ( 'NONE', #13084, #24853, #1511 ) ;
#17659 = ADVANCED_FACE ( 'NONE', ( #29284 ), #29755, .T. ) ;
#17660 = CARTESIAN_POINT ( 'NONE',  ( 139.5152310637605808, -10.00000000000000533, -30.37205893520530964 ) ) ;
#17661 = ADVANCED_FACE ( 'NONE', ( #17628 ), #15179, .T. ) ;
#17662 = ORIENTED_EDGE ( 'NONE', *, *, #3348, .T. ) ;
#17663 = CYLINDRICAL_SURFACE ( 'NONE', #26482, 5.000000000000000888 ) ;
#17664 = DIRECTION ( 'NONE',  ( 0.3090169943749475623, 8.338696094058001131E-17, 0.9510565162951536422 ) ) ;
#17665 = VERTEX_POINT ( 'NONE', #19920 ) ;
#17666 = VECTOR ( 'NONE', #27658, 1000.000000000000000 ) ;
#17667 = APPLICATION_CONTEXT ( 'automotive_design' ) ;
#17668 = CARTESIAN_POINT ( 'NONE',  ( 142.2287565553230309, -4.999999999999979572, -12.16987298107780013 ) ) ;
#17669 = LINE ( 'NONE', #29643, #8468 ) ;
#17670 = CARTESIAN_POINT ( 'NONE',  ( 12.02841764901576838, 9.314357472305010432, -16.69117924060192948 ) ) ;
#17671 = CARTESIAN_POINT ( 'NONE',  ( 33.23735339574943026, -11.79161913663336314, -18.04114522998021997 ) ) ;
#17672 = VERTEX_POINT ( 'NONE', #19760 ) ;
#17673 = CARTESIAN_POINT ( 'NONE',  ( 9.132840175088396961, 16.08822907886823472, -17.04632583937691592 ) ) ;
#17674 = VERTEX_POINT ( 'NONE', #3906 ) ;
#17675 = AXIS2_PLACEMENT_3D ( 'NONE', #10488, #12934, #6529 ) ;
#17676 = CARTESIAN_POINT ( 'NONE',  ( 24.14158683625483803, -3.940216521628096658, -13.50644477367014673 ) ) ;
#17677 = CARTESIAN_POINT ( 'NONE',  ( 17.21732962576914616, 11.43796928512929867, -12.64914394394206454 ) ) ;
#17678 = FACE_BOUND ( 'NONE', #556, .T. ) ;
#17679 = ADVANCED_FACE ( 'NONE', ( #24363 ), #29128, .T. ) ;
#17680 = VERTEX_POINT ( 'NONE', #1777 ) ;
#17681 = LINE ( 'NONE', #27037, #18316 ) ;
#17682 = CARTESIAN_POINT ( 'NONE',  ( 11.69419402147360110, 8.800013620902292999, -15.72776802682527730 ) ) ;
#17683 = CARTESIAN_POINT ( 'NONE',  ( 13.38537325061315286, -5.000000000000014211, 41.19594289235809015 ) ) ;
#17684 = VERTEX_POINT ( 'NONE', #29602 ) ;
#17685 = DIRECTION ( 'NONE',  ( 0.9510565162951535312, 2.566386769018988816E-16, -0.3090169943749475623 ) ) ;
#17686 = VERTEX_POINT ( 'NONE', #4055 ) ;
#17687 = CARTESIAN_POINT ( 'NONE',  ( 9.661883135045433946, 16.25482629684424296, -17.91562380025844803 ) ) ;
#17688 = ORIENTED_EDGE ( 'NONE', *, *, #12414, .T. ) ;
#17689 = CARTESIAN_POINT ( 'NONE',  ( 14.60232135752762517, 2.980368010496468933, -17.13315712471359475 ) ) ;
#17690 = CARTESIAN_POINT ( 'NONE',  ( 19.51424001318473245, 7.885341048999412017, -19.79681821819610832 ) ) ;
#17691 = DIRECTION ( 'NONE',  ( 0.000000000000000000, 2.775557561562890735E-17, -1.000000000000000000 ) ) ;
#17692 = DIRECTION ( 'NONE',  ( 1.000000000000000000, 2.698458740408365879E-16, -1.110223024625156540E-16 ) ) ;
#17693 = CARTESIAN_POINT ( 'NONE',  ( 19.07848178107829540, -2.338951347401693859, -17.85627120065723616 ) ) ;
#17694 = VECTOR ( 'NONE', #28947, 1000.000000000000000 ) ;
#17695 = DIRECTION ( 'NONE',  ( 0.000000000000000000, 0.000000000000000000, -1.000000000000000000 ) ) ;
#17696 = PLANE ( 'NONE',  #8880 ) ;
#17697 = ORIENTED_EDGE ( 'NONE', *, *, #8578, .F. ) ;
#17698 = DIRECTION ( 'NONE',  ( 0.000000000000000000, 0.000000000000000000, 1.000000000000000000 ) ) ;
#17699 = CARTESIAN_POINT ( 'NONE',  ( 32.58918748260075660, -11.04229556371213583, -18.21152344180378080 ) ) ;
#17700 = CARTESIAN_POINT ( 'NONE',  ( 0.000000000000000000, -1.178949249685215417, -2.041999999999998483 ) ) ;
#17701 = ORIENTED_EDGE ( 'NONE', *, *, #16659, .T. ) ;
#17702 = ORIENTED_EDGE ( 'NONE', *, *, #10827, .F. ) ;
#17703 = DIRECTION ( 'NONE',  ( 0.9510565162951536422, 0.000000000000000000, -0.3090169943749475623 ) ) ;
#17704 = PRODUCT_DEFINITION_CONTEXT ( 'detailed design', #16700, 'design' ) ;
#17705 = CARTESIAN_POINT ( 'NONE',  ( 12.51736351114195500, 9.636405190433555035, -15.11633598780129439 ) ) ;
#17706 = CARTESIAN_POINT ( 'NONE',  ( 35.09535884372434111, -21.14837076832613860, -21.10414782775458420 ) ) ;
#17707 = EDGE_CURVE ( 'NONE', #30082, #22823, #6042, .T. ) ;
#17708 = SHAPE_REPRESENTATION ( 'pedal', ( #13190 ), #24415 ) ;
#17709 = CARTESIAN_POINT ( 'NONE',  ( 149.7287565553230309, -4.999999999999977796, -33.82050807568879947 ) ) ;
#17710 = ORIENTED_EDGE ( 'NONE', *, *, #23765, .T. ) ;
#17711 = CARTESIAN_POINT ( 'NONE',  ( 12.93612603019711571, 8.763434079353435990, -14.78257486846209368 ) ) ;
#17712 = ADVANCED_FACE ( 'NONE', ( #29453 ), #22674, .T. ) ;
#17713 = ORIENTED_EDGE ( 'NONE', *, *, #9583, .F. ) ;
#17714 = CARTESIAN_POINT ( 'NONE',  ( 10.62817821613907476, 9.230418211344437296, -16.42795095778131298 ) ) ;
#17715 = CARTESIAN_POINT ( 'NONE',  ( 172.2287565553229456, -1.999999999999969358, -29.49038105676660493 ) ) ;
#17716 = CARTESIAN_POINT ( 'NONE',  ( 138.6922820468854525, -4.999999999999980460, -26.58683881228715506 ) ) ;
#17717 = DIRECTION ( 'NONE',  ( -0.5877852522924731371, -1.586114251531760728E-16, -0.8090169943749474513 ) ) ;
#17718 = ORIENTED_EDGE ( 'NONE', *, *, #29961, .F. ) ;
#17719 = CARTESIAN_POINT ( 'NONE',  ( 12.88201729092779857, 9.522117202545773651, -16.10446439827067167 ) ) ;
#17720 = CARTESIAN_POINT ( 'NONE',  ( 32.96976325559394638, -10.97479806523316448, -15.05356414682637833 ) ) ;
#17721 = CARTESIAN_POINT ( 'NONE',  ( 23.16390915794477223, 2.882539813099532555, -14.99485278278146438 ) ) ;
#17722 = EDGE_LOOP ( 'NONE', ( #15963, #24658, #22585, #26773 ) ) ;
#17723 = ORIENTED_EDGE ( 'NONE', *, *, #15376, .F. ) ;
#17724 = DIRECTION ( 'NONE',  ( -0.5877852522924731371, -1.586114251531760728E-16, -0.8090169943749474513 ) ) ;
#17725 = LINE ( 'NONE', #6144, #18445 ) ;
#17726 = CARTESIAN_POINT ( 'NONE',  ( 139.7287565553230309, -1.999999999999978684, -33.82050807568879947 ) ) ;
#17727 = CARTESIAN_POINT ( 'NONE',  ( 26.00956027078203192, -8.595392566010074731, -19.46287731774799212 ) ) ;
#17728 = CARTESIAN_POINT ( 'NONE',  ( 18.10326352236751646, 1.905885860032081158, -14.21403189877281825 ) ) ;
#17729 = ORIENTED_EDGE ( 'NONE', *, *, #12212, .F. ) ;
#17730 = ORIENTED_EDGE ( 'NONE', *, *, #8325, .T. ) ;
#17731 = CARTESIAN_POINT ( 'NONE',  ( 146.1922820468854241, -4.999999999999978684, -13.59645775552055902 ) ) ;
#17732 = LINE ( 'NONE', #1588, #15542 ) ;
#17733 = AXIS2_PLACEMENT_3D ( 'NONE', #16167, #13313, #25940 ) ;
#17734 = LINE ( 'NONE', #17877, #23091 ) ;
#17735 = LINE ( 'NONE', #8878, #14464 ) ;
#17736 = LINE ( 'NONE', #29414, #20887 ) ;
#17737 = LINE ( 'NONE', #13316, #4635 ) ;
#17738 = UNCERTAINTY_MEASURE_WITH_UNIT (LENGTH_MEASURE( 1.000000000000000082E-05 ), #18528, 'distance_accuracy_value', 'NONE');
#17739 = CARTESIAN_POINT ( 'NONE',  ( 11.32192133241855103, 8.753083428987814330, -17.19257025691282337 ) ) ;
#17740 = EDGE_LOOP ( 'NONE', ( #25024, #701, #20597, #25392 ) ) ;
#17741 = CARTESIAN_POINT ( 'NONE',  ( 10.33811693838771717, 18.38618951776012267, -17.91664992932185996 ) ) ;
#17742 = CARTESIAN_POINT ( 'NONE',  ( 144.5152310637605808, -1.999999999999977129, -30.37205893520530964 ) ) ;
#17743 = EDGE_CURVE ( 'NONE', #30193, #3398, #15029, .T. ) ;
#17744 = EDGE_CURVE ( 'NONE', #11783, #19520, #8471, .T. ) ;
#17745 = ORIENTED_EDGE ( 'NONE', *, *, #7202, .F. ) ;
#17746 = CARTESIAN_POINT ( 'NONE',  ( 152.0152310637605524, -1.999999999999974909, -26.04193191628311155 ) ) ;
#17747 = CARTESIAN_POINT ( 'NONE',  ( 134.5152310637605524, -1.999999999999980460, -4.391296821672111328 ) ) ;
#17748 = VERTEX_POINT ( 'NONE', #5745 ) ;
#17749 = CARTESIAN_POINT ( 'NONE',  ( 146.1922820468854241, -1.999999999999977573, -10.74328820663507678 ) ) ;
#17750 = EDGE_CURVE ( 'NONE', #25132, #27772, #24818, .T. ) ;
#17751 = CARTESIAN_POINT ( 'NONE',  ( 134.7287565553230024, -4.999999999999982236, -33.82050807568879947 ) ) ;
#17752 = LINE ( 'NONE', #27110, #13227 ) ;
#17753 = EDGE_CURVE ( 'NONE', #11968, #1963, #15326, .T. ) ;
#17755 = ORIENTED_EDGE ( 'NONE', *, *, #13412, .F. ) ;
#17754 = CARTESIAN_POINT ( 'NONE',  ( 20.39549844898813191, -2.061726703908969505, -13.85117726305786512 ) ) ;
#17756 = ORIENTED_EDGE ( 'NONE', *, *, #1039, .T. ) ;
#17757 = CARTESIAN_POINT ( 'NONE',  ( 144.5152310637605808, -1.999999999999977573, -11.28819510263909542 ) ) ;
#17758 = CARTESIAN_POINT ( 'NONE',  ( 15.36220012886423447, 10.89358938796158149, -12.84895098869522201 ) ) ;
#17759 = CARTESIAN_POINT ( 'NONE',  ( 146.1922820468854241, -1.999999999999977129, -10.74328820663507678 ) ) ;
#17760 = DIRECTION ( 'NONE',  ( 0.5877852522924731371, 0.000000000000000000, 0.8090169943749474513 ) ) ;
#17761 = CARTESIAN_POINT ( 'NONE',  ( 27.78884322698630882, -6.380937659459246625, -17.89340433249687834 ) ) ;
#17762 = VECTOR ( 'NONE', #15492, 1000.000000000000000 ) ;
#17763 = LINE ( 'NONE', #1463, #13511 ) ;
#17764 = CARTESIAN_POINT ( 'NONE',  ( 19.88777865313588222, 4.107626486979258473, -13.29018489620430721 ) ) ;
#17765 = EDGE_LOOP ( 'NONE', ( #2326, #1319, #16086, #13028 ) ) ;
#17766 = DIRECTION ( 'NONE',  ( -2.698458740408365879E-16, 1.000000000000000000, 0.000000000000000000 ) ) ;
#17767 = VERTEX_POINT ( 'NONE', #22069 ) ;
#17768 = CARTESIAN_POINT ( 'NONE',  ( 18.16551323082808267, 7.152368624112494189, -14.07085781252208712 ) ) ;
#17769 = CARTESIAN_POINT ( 'NONE',  ( 23.88957251509086888, -3.236156964677408876, -12.29669325917074829 ) ) ;
#17770 = ORIENTED_EDGE ( 'NONE', *, *, #4777, .T. ) ;
#17771 = CARTESIAN_POINT ( 'NONE',  ( 157.0152310637604955, -4.999999999999975131, -1.743219247438260128E-14 ) ) ;
#17772 = DIRECTION ( 'NONE',  ( 1.000000000000000000, 2.698458740408365879E-16, -1.110223024625156540E-16 ) ) ;
#17773 = LINE ( 'NONE', #17629, #13645 ) ;
#17774 = DIRECTION ( 'NONE',  ( -0.5877852522924731371, -1.586114251531760235E-16, 0.8090169943749474513 ) ) ;
#17775 = CARTESIAN_POINT ( 'NONE',  ( 9.885273420212257633, -5.000000000000015099, 30.42374326586335798 ) ) ;
#17776 = VECTOR ( 'NONE', #2347, 1000.000000000000000 ) ;
#17777 = DIRECTION ( 'NONE',  ( -2.698458740408365879E-16, 1.000000000000000000, 0.000000000000000000 ) ) ;
#17778 = CARTESIAN_POINT ( 'NONE',  ( 25.68863286643039601, -3.692565893519352827, -17.49701707463368550 ) ) ;
#17779 = DIRECTION ( 'NONE',  ( 0.5877852522924731371, 1.586114251531760728E-16, -0.8090169943749474513 ) ) ;
#17780 = CARTESIAN_POINT ( 'NONE',  ( 35.69176435403931436, -19.33523451612313693, -21.37328632439622922 ) ) ;
#17781 = FACE_OUTER_BOUND ( 'NONE', #3550, .T. ) ;
#17782 = CARTESIAN_POINT ( 'NONE',  ( 12.49428694376680049, 8.568214790255201052, -15.13472557389765072 ) ) ;
#17783 = EDGE_CURVE ( 'NONE', #7245, #3516, #13207, .T. ) ;
#17784 = PLANE ( 'NONE',  #19535 ) ;
#17785 = CARTESIAN_POINT ( 'NONE',  ( 23.24172714540143048, -5.000000000000011546, -71.53068101092122788 ) ) ;
#17786 = EDGE_CURVE ( 'NONE', #4321, #9967, #3602, .T. ) ;
#17787 = EDGE_CURVE ( 'NONE', #1554, #26475, #8324, .T. ) ;
#17788 = CARTESIAN_POINT ( 'NONE',  ( 9.661901852922078149, 16.25474045427587200, -17.91339448853296901 ) ) ;
#17789 = CARTESIAN_POINT ( 'NONE',  ( 146.1922820468854525, -10.00000000000000178, -30.91696583120935671 ) ) ;
#17790 = DIRECTION ( 'NONE',  ( -1.110223024625156540E-16, 0.000000000000000000, -1.000000000000000000 ) ) ;
#17791 = CARTESIAN_POINT ( 'NONE',  ( 11.45661370752365116, 9.343864103108954211, -15.86763743611193789 ) ) ;
#17792 = ORIENTED_EDGE ( 'NONE', *, *, #19476, .F. ) ;
#17793 = CARTESIAN_POINT ( 'NONE',  ( 137.0152310637605524, -1.999999999999980016, -0.06116980274991495881 ) ) ;
#17794 = CARTESIAN_POINT ( 'NONE',  ( 172.0152310637604103, -1.999999999999970468, -8.721423840594312082 ) ) ;
#17795 = CARTESIAN_POINT ( 'NONE',  ( 14.03850921439652311, 8.975161913830900673, -15.18271992443145635 ) ) ;
#17796 = VERTEX_POINT ( 'NONE', #6946 ) ;
#17797 = CARTESIAN_POINT ( 'NONE',  ( 16.49632153860815720, 9.003283391651189405, -13.22380011606493788 ) ) ;
#17798 = CARTESIAN_POINT ( 'NONE',  ( 35.88008189734257769, -20.18124548360443882, -21.42481968387543390 ) ) ;
#17799 = CARTESIAN_POINT ( 'NONE',  ( 17.49446177548951553, 10.34313653870878547, -20.19723249710358104 ) ) ;
#17800 = CARTESIAN_POINT ( 'NONE',  ( 28.12627659338356878, -5.062120396530918498, -14.05642262879015369 ) ) ;
#17801 = DIRECTION ( 'NONE',  ( -0.9510565162951536422, -2.566386769018988816E-16, -0.3090169943749472292 ) ) ;
#17802 = FACE_OUTER_BOUND ( 'NONE', #28146, .T. ) ;
#17803 = CIRCLE ( 'NONE', #10484, 3.000000000000002665 ) ;
#17804 = CARTESIAN_POINT ( 'NONE',  ( 132.2287565553230309, -4.999999999999981348, -29.49038105676660848 ) ) ;
#17805 = CARTESIAN_POINT ( 'NONE',  ( 21.97327598498023704, 3.176719406474355800, -15.71098195781089046 ) ) ;
#17806 = ORIENTED_EDGE ( 'NONE', *, *, #18448, .T. ) ;
#17807 = CARTESIAN_POINT ( 'NONE',  ( 163.6922820468853672, -1.999999999999972244, -26.58683881228715862 ) ) ;
#17808 = CARTESIAN_POINT ( 'NONE',  ( 149.5152310637604955, -4.999999999999976907, -1.659952520591373388E-14 ) ) ;
#17809 = DIRECTION ( 'NONE',  ( -0.9510565162951536422, -2.566386769018988323E-16, 0.3090169943749475623 ) ) ;
#17810 = CARTESIAN_POINT ( 'NONE',  ( 130.7287565553229172, -10.00000000000000888, -22.10610323145025902 ) ) ;
#17811 = VECTOR ( 'NONE', #20867, 1000.000000000000000 ) ;
#17812 = CARTESIAN_POINT ( 'NONE',  ( 12.03055882466574289, 9.304755949677762317, -16.69027714870545864 ) ) ;
#17813 = CARTESIAN_POINT ( 'NONE',  ( 35.19403856461168090, -19.59168648217519504, -19.20845343762490032 ) ) ;
#17814 = ORIENTED_EDGE ( 'NONE', *, *, #29403, .F. ) ;
#17815 = CIRCLE ( 'NONE', #15403, 9.000000000000007105 ) ;
#17816 = CARTESIAN_POINT ( 'NONE',  ( 9.114604345319493817, 16.17186091871610287, -17.05386699646955861 ) ) ;
#17817 = EDGE_CURVE ( 'NONE', #16514, #21374, #79, .T. ) ;
#17818 = EDGE_CURVE ( 'NONE', #10508, #17512, #7958, .T. ) ;
#17819 = STYLED_ITEM ( 'NONE', ( #20980 ), #21231 ) ;
#17820 = CARTESIAN_POINT ( 'NONE',  ( 28.16462234717350199, -5.661059359726887230, -16.30864077692347536 ) ) ;
#17821 = ADVANCED_FACE ( 'NONE', ( #11213 ), #8437, .T. ) ;
#17822 = CARTESIAN_POINT ( 'NONE',  ( 12.86812980024498643, 9.515982172609518841, -16.11553281326163045 ) ) ;
#17823 = DIRECTION ( 'NONE',  ( -2.698458740408365879E-16, 1.000000000000000000, 0.000000000000000000 ) ) ;
#17824 = ADVANCED_FACE ( 'NONE', ( #6494 ), #16392, .T. ) ;
#17825 = ORIENTED_EDGE ( 'NONE', *, *, #22532, .F. ) ;
#17826 = PLANE ( 'NONE',  #2249 ) ;
#17827 = ORIENTED_EDGE ( 'NONE', *, *, #28100, .F. ) ;
#17828 = FACE_OUTER_BOUND ( 'NONE', #2282, .T. ) ;
#17829 = CARTESIAN_POINT ( 'NONE',  ( 144.7287565553229740, -1.999999999999978018, 0.8205080756887930260 ) ) ;
#17830 = CARTESIAN_POINT ( 'NONE',  ( 162.0152310637605524, -9.999999999999998224, -32.93883019725009120 ) ) ;
#17831 = ORIENTED_EDGE ( 'NONE', *, *, #13208, .F. ) ;
#17832 = CARTESIAN_POINT ( 'NONE',  ( 9.661883795922106444, 16.25482326597959926, -17.91529654610192424 ) ) ;
#17833 = CARTESIAN_POINT ( 'NONE',  ( 16.15008960989130671, 4.591438144365319829, -20.60273134265763062 ) ) ;
#17834 = CARTESIAN_POINT ( 'NONE',  ( 19.44145409300831417, 9.016062086884520710, -15.75081756649476894 ) ) ;
#17835 = CARTESIAN_POINT ( 'NONE',  ( 15.00000000000000000, 0.000000000000000000, 0.000000000000000000 ) ) ;
#17836 = ORIENTED_EDGE ( 'NONE', *, *, #18578, .T. ) ;
#17837 = DIRECTION ( 'NONE',  ( -0.5877852522924731371, -1.586114251531760235E-16, 0.8090169943749474513 ) ) ;
#17838 = AXIS2_PLACEMENT_3D ( 'NONE', #1121, #3399, #16978 ) ;
#17839 = CARTESIAN_POINT ( 'NONE',  ( 23.66601916330066402, 2.199037240492611733, -18.57254039386976885 ) ) ;
#17840 = CARTESIAN_POINT ( 'NONE',  ( 24.00000000000017053, 34.64101615137744972, 14.00000000000000178 ) ) ;
#17841 = CARTESIAN_POINT ( 'NONE',  ( 142.0152310637605524, -1.999999999999978462, -8.721423840594312082 ) ) ;
#17842 = VERTEX_POINT ( 'NONE', #8763 ) ;
#17843 = VERTEX_POINT ( 'NONE', #23118 ) ;
#17844 = DIRECTION ( 'NONE',  ( 0.9510565162951536422, 0.000000000000000000, -0.3090169943749475623 ) ) ;
#17845 = CARTESIAN_POINT ( 'NONE',  ( 35.18065281855160720, -20.53155141575438591, -20.22037173032050461 ) ) ;
#17846 = CARTESIAN_POINT ( 'NONE',  ( 16.40801556695141628, -5.000000000000013323, 50.49867938812164425 ) ) ;
#17847 = VERTEX_POINT ( 'NONE', #15784 ) ;
#17848 = DIRECTION ( 'NONE',  ( -6.938893903907227392E-16, 0.000000000000000000, -1.000000000000000000 ) ) ;
#17849 = VECTOR ( 'NONE', #9500, 1000.000000000000000 ) ;
#17850 = EDGE_CURVE ( 'NONE', #4159, #6652, #22826, .T. ) ;
#17851 = CARTESIAN_POINT ( 'NONE',  ( 12.25364105430271700, 9.519861518574414205, -15.32652744092241726 ) ) ;
#17852 = CARTESIAN_POINT ( 'NONE',  ( 35.54859390953724585, -23.18451583373416014, -16.11276402859391510 ) ) ;
#17853 = EDGE_CURVE ( 'NONE', #24692, #13894, #1928, .T. ) ;
#17854 = ORIENTED_EDGE ( 'NONE', *, *, #10161, .T. ) ;
#17855 = AXIS2_PLACEMENT_3D ( 'NONE', #5496, #14782, #19669 ) ;
#17856 = CARTESIAN_POINT ( 'NONE',  ( 13.00000000000000178, 1.592040838891559293E-15, -18.00000000000000000 ) ) ;
#17857 = CONICAL_SURFACE ( 'NONE', #9558, 8.000000000000007105, 1.047197551196596077 ) ;
#17858 = CARTESIAN_POINT ( 'NONE',  ( 10.66363677402306287, 9.067800744973538940, -16.41328759676781246 ) ) ;
#17859 = LINE ( 'NONE', #15428, #25386 ) ;
#17860 = DIRECTION ( 'NONE',  ( -2.698458740408365879E-16, 1.000000000000000000, 0.000000000000000000 ) ) ;
#17861 = VERTEX_POINT ( 'NONE', #20517 ) ;
#17862 = CARTESIAN_POINT ( 'NONE',  ( 12.86796368952119174, 9.515911916162036022, -16.11566496612908139 ) ) ;
#17863 = CARTESIAN_POINT ( 'NONE',  ( 33.25614251967556356, -10.36847857886694868, -17.86465469861353483 ) ) ;
#17864 = CARTESIAN_POINT ( 'NONE',  ( 21.40051611374530793, -0.1690565882708310874, -20.18282279970310000 ) ) ;
#17865 = VERTEX_POINT ( 'NONE', #4796 ) ;
#17866 = CARTESIAN_POINT ( 'NONE',  ( 131.1922820468854241, -1.999999999999982236, -4.936203717676158398 ) ) ;
#17867 = CARTESIAN_POINT ( 'NONE',  ( -4.000000000000003553, 1.557668341133489953, -0.1596965656957523294 ) ) ;
#17868 = DIRECTION ( 'NONE',  ( -0.8090169943749474513, -2.183098979609982436E-16, -0.5877852522924731371 ) ) ;
#17869 = CARTESIAN_POINT ( 'NONE',  ( 23.54468722040186890, -6.934586491718037315, -13.40271233150634878 ) ) ;
#17870 = CARTESIAN_POINT ( 'NONE',  ( 24.72855373928933531, -1.476844508782828802, -20.15487193605729033 ) ) ;
#17871 = VECTOR ( 'NONE', #14814, 1000.000000000000000 ) ;
#17872 = ORIENTED_EDGE ( 'NONE', *, *, #29751, .F. ) ;
#17873 = EDGE_CURVE ( 'NONE', #4960, #1409, #27736, .T. ) ;
#17874 = FACE_OUTER_BOUND ( 'NONE', #28376, .T. ) ;
#17875 = VECTOR ( 'NONE', #28479, 1000.000000000000000 ) ;
#17876 = CARTESIAN_POINT ( 'NONE',  ( 168.6922820468853956, -9.999999999999996447, -32.39392330124607611 ) ) ;
#17877 = CARTESIAN_POINT ( 'NONE',  ( 138.6922820468854525, -10.00000000000000533, -6.413161187712876909 ) ) ;
#17878 = CARTESIAN_POINT ( 'NONE',  ( 172.0152310637604955, -9.999999999999994671, -34.70218595412750773 ) ) ;
#17879 =( BOUNDED_SURFACE ( )  B_SPLINE_SURFACE ( 3, 3, ( 
 ( #18762, #158, #26249, #7025, #2909, #7175, #23811, #7616, #2751, #23346, #609, #21194, #14470, #16466, #9291, #2460, #5336, #28270, #16920, #11735, #23969, #25793, #2606, #21052, #20894, #28418, #5, #12038, #25632, #9896, #16315, #18616, #9436, #28115, #25943, #26099, #4874, #23496, #16624, #11881, #9594, #5024, #14315, #23650, #21352, #19064, #458, #9744, #7472, #16775, #5178, #26403, #3503, #17367, #22111, #14917, #26874, #905, #12333, #10351, #29021, #7915, #24556, #17078, #5482, #12793, #14765, #8365, #17520, #24106, #8057, #26714, #5939, #3206, #5786, #15069, #22257, #26553 ),
 ( #3354, #10495, #3648, #1365, #19356, #12484, #12641, #19656, #21808, #15223, #19807, #12943, #24407, #24257, #17671, #10655, #21959, #5637, #29337, #10197, #19967, #19509, #1213, #745, #27028, #17226, #10043, #6083, #15379, #1071, #28883, #3058, #29169, #21647, #8208, #28717, #7765, #1672, #13252, #9101, #20116, #15981, #20259, #6692, #2125, #15827, #17813, #25308, #4101, #27626, #29645, #22419, #27186, #18429, #11105, #11396, #6239, #27779, #8662, #15685, #15534, #6844, #11257, #3801, #25156, #8515, #13698, #29496, #24713, #20703, #13091, #8811, #8954, #24866, #17967, #20411, #22572, #3953 ),
 ( #22721, #27340, #30091, #29803, #1523, #10806, #10952, #6394, #20559, #25014, #13394, #22868, #1825, #29944, #18119, #23022, #27484, #6538, #4249, #13544, #1977, #18270, #4398, #4990, #16132, #28233, #12154, #9554, #5141, #30239, #14431, #23157, #14136, #16433, #28386, #9704, #20856, #19030, #11997, #21313, #28533, #422, #16589, #9251, #23774, #28077, #25590, #11699, #18579, #14281, #25755, #4837, #25454, #18875, #272, #7286, #25913, #4544, #2271, #23464, #7133, #7441, #4684, #23614, #2422, #11847, #2710, #16743, #9401, #18730, #2574, #13978, #23308, #21015, #26066, #13834, #2870, #21469 ),
 ( #19176, #11541, #27927, #577, #6989, #16278, #9863, #120, #21158, #17192, #26836, #17043, #16885, #8025, #874, #28846, #22078, #26215, #26678, #7582, #19622, #3614, #1033, #5907, #21618, #15189, #14583, #5601, #7884, #19766, #1180, #12301, #10461, #3464, #12754, #19930, #29136, #17333, #715, #24521, #19473, #26371, #3177, #10008, #5755, #26519, #14880, #5299, #10314, #21920, #28988, #15037, #23933, #3025, #24225, #3325, #8175, #5450, #24369, #24074, #12604, #17487, #12906, #10162, #22220, #1329, #10621, #19322, #28682, #12448, #7731, #14731, #21773, #13509, #27140, #15338, #24827, #25272 ),
 ( #24675, #27303, #15945, #1940, #27451, #13215, #10776, #4211, #17927, #25121, #1637, #6357, #26992, #22382, #13661, #15651, #6651, #1486, #22985, #22539, #20225, #20085, #2088, #15794, #8333, #20374, #13058, #18235, #3765, #11365, #4359, #29296, #13359, #22836, #29461, #3916, #24983, #10916, #11222, #6203, #17636, #4066, #22684, #29611, #20525, #8479, #17780, #29764, #15496, #6049, #29912, #8627, #1785, #11071, #8921, #8773, #18088, #6503, #27593, #13946, #4959, #9215, #23580, #20977, #28201, #11962, #18999, #6805, #13799, #87, #28043, #18542, #14249, #7258, #390, #14098, #11663, #5107 ),
 ( #2544, #4805, #2836, #16095, #9368, #18698, #2677, #30206, #21130, #6958, #16399, #11815, #21279, #23275, #2390, #7099, #25723, #23431, #241, #16246, #9676, #4510, #30055, #28356, #27897, #25421, #25558, #16712, #7412, #9518, #18840, #23125, #16556, #26033, #14398, #25880, #4653, #2236, #23739, #20670, #9065, #18390, #27745, #11506, #20822, #26333, #10842, #12122, #29377, #19146, #21437, #9975, #7551, #8401, #5567, #28503, #17706, #16855, #27067, #14846, #23898, #19438, #22464, #13132, #28810, #688, #6122, #1562, #26183, #29532, #24905, #19290, #15420, #10127, #5416, #17852, #7848, #8549 ),
 ( #5263, #12565, #26486, #997, #24044, #24754, #28647, #549, #17157, #24189, #17010, #3840, #14551, #2995, #21884, #12271, #27228, #20150, #21589, #3290, #10278, #6278, #7698, #20009, #15571, #9830, #14701, #3142, #12417, #21733, #836, #11436, #25499, #2317, #20298, #27381, #4289, #11297, #22759, #27822, #20746, #13878, #27668, #25199, #18624, #4588, #13591, #27526, #12, #18012, #11587, #1871, #13736, #1707, #30135, #2018, #20901, #11150, #20452, #8850, #6731, #10990, #15869, #15725, #9299, #18165, #29686, #23200, #27972, #6581, #6433, #16178, #29845, #6889, #20601, #22915, #23063, #29984 ) ),
 .UNSPECIFIED., .T., .F., .F. ) 
 B_SPLINE_SURFACE_WITH_KNOTS ( ( 4, 3, 4 ),
 ( 4, 2, 2, 2, 2, 2, 2, 2, 2, 2, 2, 2, 2, 2, 2, 2, 2, 2, 2, 2, 2, 2, 2, 2, 2, 2, 2, 2, 2, 2, 2, 2, 2, 2, 2, 2, 2, 2, 4 ),
 ( 0.000000000000000000, 0.5000000000000000000, 1.000000000000000000 ),
 ( 0.000000000000000000, 0.1003381136405422785, 0.1505071704608134109, 0.1755916988709489979, 0.1881339630760167636, 0.1944050951785506465, 0.2006762272810845571, 0.2086934065084689038, 0.2167105857358532783, 0.2327449441906219718, 0.2648136611001593588, 0.2968823780096967457, 0.3129167364644654947, 0.3209339156918498137, 0.3289510949192341882, 0.3346579968240730452, 0.3403648987289118466, 0.3517787025385894495, 0.3746063101579446553, 0.4202615253966550668, 0.5115719558740758899, 0.6028823863514967130, 0.6485376015902071245, 0.6713652092095623303, 0.6827790130192399332, 0.6941928168289175360, 0.7036545619149295883, 0.7131163070009416405, 0.7320397971729657449, 0.7698867775170139538, 0.8077337578610621627, 0.8266572480330862671, 0.8361189931190984304, 0.8455807382051104826, 0.8552319420672911399, 0.8648831459294716861, 0.8841855536538327787, 0.9227903691025551858, 1.000000000000000000 ),
 .UNSPECIFIED. ) 
 GEOMETRIC_REPRESENTATION_ITEM ( )  RATIONAL_B_SPLINE_SURFACE ( (
 ( 1.000000000000000000, 1.000000000000000000, 1.000000000000000000, 1.000000000000000000, 1.000000000000000000, 1.000000000000000000, 1.000000000000000000, 1.000000000000000000, 1.000000000000000000, 1.000000000000000000, 1.000000000000000000, 1.000000000000000000, 1.000000000000000000, 1.000000000000000000, 1.000000000000000000, 1.000000000000000000, 1.000000000000000000, 1.000000000000000000, 1.000000000000000000, 1.000000000000000000, 1.000000000000000000, 1.000000000000000000, 1.000000000000000000, 1.000000000000000000, 1.000000000000000000, 1.000000000000000000, 1.000000000000000000, 1.000000000000000000, 1.000000000000000000, 1.000000000000000000, 1.000000000000000000, 1.000000000000000000, 1.000000000000000000, 1.000000000000000000, 1.000000000000000000, 1.000000000000000000, 1.000000000000000000, 1.000000000000000000, 1.000000000000000000, 1.000000000000000000, 1.000000000000000000, 1.000000000000000000, 1.000000000000000000, 1.000000000000000000, 1.000000000000000000, 1.000000000000000000, 1.000000000000000000, 1.000000000000000000, 1.000000000000000000, 1.000000000000000000, 1.000000000000000000, 1.000000000000000000, 1.000000000000000000, 1.000000000000000000, 1.000000000000000000, 1.000000000000000000, 1.000000000000000000, 1.000000000000000000, 1.000000000000000000, 1.000000000000000000, 1.000000000000000000, 1.000000000000000000, 1.000000000000000000, 1.000000000000000000, 1.000000000000000000, 1.000000000000000000, 1.000000000000000000, 1.000000000000000000, 1.000000000000000000, 1.000000000000000000, 1.000000000000000000, 1.000000000000000000, 1.000000000000000000, 1.000000000000000000, 1.000000000000000000, 1.000000000000000000, 1.000000000000000000, 1.000000000000000000),
 ( 0.3333333333333333703, 0.3333333333333333703, 0.3333333333333333703, 0.3333333333333333703, 0.3333333333333333703, 0.3333333333333333703, 0.3333333333333333703, 0.3333333333333333703, 0.3333333333333333703, 0.3333333333333333703, 0.3333333333333333703, 0.3333333333333333703, 0.3333333333333333703, 0.3333333333333333703, 0.3333333333333333703, 0.3333333333333333703, 0.3333333333333333703, 0.3333333333333333703, 0.3333333333333333703, 0.3333333333333333703, 0.3333333333333333703, 0.3333333333333333703, 0.3333333333333333703, 0.3333333333333333703, 0.3333333333333333703, 0.3333333333333333703, 0.3333333333333333703, 0.3333333333333333703, 0.3333333333333333703, 0.3333333333333333703, 0.3333333333333333703, 0.3333333333333333703, 0.3333333333333333703, 0.3333333333333333703, 0.3333333333333333703, 0.3333333333333333703, 0.3333333333333333703, 0.3333333333333333703, 0.3333333333333333703, 0.3333333333333333703, 0.3333333333333333703, 0.3333333333333333703, 0.3333333333333333703, 0.3333333333333333703, 0.3333333333333333703, 0.3333333333333333703, 0.3333333333333333703, 0.3333333333333333703, 0.3333333333333333703, 0.3333333333333333703, 0.3333333333333333703, 0.3333333333333333703, 0.3333333333333333703, 0.3333333333333333703, 0.3333333333333333703, 0.3333333333333333703, 0.3333333333333333703, 0.3333333333333333703, 0.3333333333333333703, 0.3333333333333333703, 0.3333333333333333703, 0.3333333333333333703, 0.3333333333333333703, 0.3333333333333333703, 0.3333333333333333703, 0.3333333333333333703, 0.3333333333333333703, 0.3333333333333333703, 0.3333333333333333703, 0.3333333333333333703, 0.3333333333333333703, 0.3333333333333333703, 0.3333333333333333703, 0.3333333333333333703, 0.3333333333333333703, 0.3333333333333333703, 0.3333333333333333703, 0.3333333333333333703),
 ( 0.3333333333333333703, 0.3333333333333333703, 0.3333333333333333703, 0.3333333333333333703, 0.3333333333333333703, 0.3333333333333333703, 0.3333333333333333703, 0.3333333333333333703, 0.3333333333333333703, 0.3333333333333333703, 0.3333333333333333703, 0.3333333333333333703, 0.3333333333333333703, 0.3333333333333333703, 0.3333333333333333703, 0.3333333333333333703, 0.3333333333333333703, 0.3333333333333333703, 0.3333333333333333703, 0.3333333333333333703, 0.3333333333333333703, 0.3333333333333333703, 0.3333333333333333703, 0.3333333333333333703, 0.3333333333333333703, 0.3333333333333333703, 0.3333333333333333703, 0.3333333333333333703, 0.3333333333333333703, 0.3333333333333333703, 0.3333333333333333703, 0.3333333333333333703, 0.3333333333333333703, 0.3333333333333333703, 0.3333333333333333703, 0.3333333333333333703, 0.3333333333333333703, 0.3333333333333333703, 0.3333333333333333703, 0.3333333333333333703, 0.3333333333333333703, 0.3333333333333333703, 0.3333333333333333703, 0.3333333333333333703, 0.3333333333333333703, 0.3333333333333333703, 0.3333333333333333703, 0.3333333333333333703, 0.3333333333333333703, 0.3333333333333333703, 0.3333333333333333703, 0.3333333333333333703, 0.3333333333333333703, 0.3333333333333333703, 0.3333333333333333703, 0.3333333333333333703, 0.3333333333333333703, 0.3333333333333333703, 0.3333333333333333703, 0.3333333333333333703, 0.3333333333333333703, 0.3333333333333333703, 0.3333333333333333703, 0.3333333333333333703, 0.3333333333333333703, 0.3333333333333333703, 0.3333333333333333703, 0.3333333333333333703, 0.3333333333333333703, 0.3333333333333333703, 0.3333333333333333703, 0.3333333333333333703, 0.3333333333333333703, 0.3333333333333333703, 0.3333333333333333703, 0.3333333333333333703, 0.3333333333333333703, 0.3333333333333333703),
 ( 1.000000000000000000, 1.000000000000000000, 1.000000000000000000, 1.000000000000000000, 1.000000000000000000, 1.000000000000000000, 1.000000000000000000, 1.000000000000000000, 1.000000000000000000, 1.000000000000000000, 1.000000000000000000, 1.000000000000000000, 1.000000000000000000, 1.000000000000000000, 1.000000000000000000, 1.000000000000000000, 1.000000000000000000, 1.000000000000000000, 1.000000000000000000, 1.000000000000000000, 1.000000000000000000, 1.000000000000000000, 1.000000000000000000, 1.000000000000000000, 1.000000000000000000, 1.000000000000000000, 1.000000000000000000, 1.000000000000000000, 1.000000000000000000, 1.000000000000000000, 1.000000000000000000, 1.000000000000000000, 1.000000000000000000, 1.000000000000000000, 1.000000000000000000, 1.000000000000000000, 1.000000000000000000, 1.000000000000000000, 1.000000000000000000, 1.000000000000000000, 1.000000000000000000, 1.000000000000000000, 1.000000000000000000, 1.000000000000000000, 1.000000000000000000, 1.000000000000000000, 1.000000000000000000, 1.000000000000000000, 1.000000000000000000, 1.000000000000000000, 1.000000000000000000, 1.000000000000000000, 1.000000000000000000, 1.000000000000000000, 1.000000000000000000, 1.000000000000000000, 1.000000000000000000, 1.000000000000000000, 1.000000000000000000, 1.000000000000000000, 1.000000000000000000, 1.000000000000000000, 1.000000000000000000, 1.000000000000000000, 1.000000000000000000, 1.000000000000000000, 1.000000000000000000, 1.000000000000000000, 1.000000000000000000, 1.000000000000000000, 1.000000000000000000, 1.000000000000000000, 1.000000000000000000, 1.000000000000000000, 1.000000000000000000, 1.000000000000000000, 1.000000000000000000, 1.000000000000000000),
 ( 0.3333333333333333703, 0.3333333333333333703, 0.3333333333333333703, 0.3333333333333333703, 0.3333333333333333703, 0.3333333333333333703, 0.3333333333333333703, 0.3333333333333333703, 0.3333333333333333703, 0.3333333333333333703, 0.3333333333333333703, 0.3333333333333333703, 0.3333333333333333703, 0.3333333333333333703, 0.3333333333333333703, 0.3333333333333333703, 0.3333333333333333703, 0.3333333333333333703, 0.3333333333333333703, 0.3333333333333333703, 0.3333333333333333703, 0.3333333333333333703, 0.3333333333333333703, 0.3333333333333333703, 0.3333333333333333703, 0.3333333333333333703, 0.3333333333333333703, 0.3333333333333333703, 0.3333333333333333703, 0.3333333333333333703, 0.3333333333333333703, 0.3333333333333333703, 0.3333333333333333703, 0.3333333333333333703, 0.3333333333333333703, 0.3333333333333333703, 0.3333333333333333703, 0.3333333333333333703, 0.3333333333333333703, 0.3333333333333333703, 0.3333333333333333703, 0.3333333333333333703, 0.3333333333333333703, 0.3333333333333333703, 0.3333333333333333703, 0.3333333333333333703, 0.3333333333333333703, 0.3333333333333333703, 0.3333333333333333703, 0.3333333333333333703, 0.3333333333333333703, 0.3333333333333333703, 0.3333333333333333703, 0.3333333333333333703, 0.3333333333333333703, 0.3333333333333333703, 0.3333333333333333703, 0.3333333333333333703, 0.3333333333333333703, 0.3333333333333333703, 0.3333333333333333703, 0.3333333333333333703, 0.3333333333333333703, 0.3333333333333333703, 0.3333333333333333703, 0.3333333333333333703, 0.3333333333333333703, 0.3333333333333333703, 0.3333333333333333703, 0.3333333333333333703, 0.3333333333333333703, 0.3333333333333333703, 0.3333333333333333703, 0.3333333333333333703, 0.3333333333333333703, 0.3333333333333333703, 0.3333333333333333703, 0.3333333333333333703),
 ( 0.3333333333333333703, 0.3333333333333333703, 0.3333333333333333703, 0.3333333333333333703, 0.3333333333333333703, 0.3333333333333333703, 0.3333333333333333703, 0.3333333333333333703, 0.3333333333333333703, 0.3333333333333333703, 0.3333333333333333703, 0.3333333333333333703, 0.3333333333333333703, 0.3333333333333333703, 0.3333333333333333703, 0.3333333333333333703, 0.3333333333333333703, 0.3333333333333333703, 0.3333333333333333703, 0.3333333333333333703, 0.3333333333333333703, 0.3333333333333333703, 0.3333333333333333703, 0.3333333333333333703, 0.3333333333333333703, 0.3333333333333333703, 0.3333333333333333703, 0.3333333333333333703, 0.3333333333333333703, 0.3333333333333333703, 0.3333333333333333703, 0.3333333333333333703, 0.3333333333333333703, 0.3333333333333333703, 0.3333333333333333703, 0.3333333333333333703, 0.3333333333333333703, 0.3333333333333333703, 0.3333333333333333703, 0.3333333333333333703, 0.3333333333333333703, 0.3333333333333333703, 0.3333333333333333703, 0.3333333333333333703, 0.3333333333333333703, 0.3333333333333333703, 0.3333333333333333703, 0.3333333333333333703, 0.3333333333333333703, 0.3333333333333333703, 0.3333333333333333703, 0.3333333333333333703, 0.3333333333333333703, 0.3333333333333333703, 0.3333333333333333703, 0.3333333333333333703, 0.3333333333333333703, 0.3333333333333333703, 0.3333333333333333703, 0.3333333333333333703, 0.3333333333333333703, 0.3333333333333333703, 0.3333333333333333703, 0.3333333333333333703, 0.3333333333333333703, 0.3333333333333333703, 0.3333333333333333703, 0.3333333333333333703, 0.3333333333333333703, 0.3333333333333333703, 0.3333333333333333703, 0.3333333333333333703, 0.3333333333333333703, 0.3333333333333333703, 0.3333333333333333703, 0.3333333333333333703, 0.3333333333333333703, 0.3333333333333333703),
 ( 1.000000000000000000, 1.000000000000000000, 1.000000000000000000, 1.000000000000000000, 1.000000000000000000, 1.000000000000000000, 1.000000000000000000, 1.000000000000000000, 1.000000000000000000, 1.000000000000000000, 1.000000000000000000, 1.000000000000000000, 1.000000000000000000, 1.000000000000000000, 1.000000000000000000, 1.000000000000000000, 1.000000000000000000, 1.000000000000000000, 1.000000000000000000, 1.000000000000000000, 1.000000000000000000, 1.000000000000000000, 1.000000000000000000, 1.000000000000000000, 1.000000000000000000, 1.000000000000000000, 1.000000000000000000, 1.000000000000000000, 1.000000000000000000, 1.000000000000000000, 1.000000000000000000, 1.000000000000000000, 1.000000000000000000, 1.000000000000000000, 1.000000000000000000, 1.000000000000000000, 1.000000000000000000, 1.000000000000000000, 1.000000000000000000, 1.000000000000000000, 1.000000000000000000, 1.000000000000000000, 1.000000000000000000, 1.000000000000000000, 1.000000000000000000, 1.000000000000000000, 1.000000000000000000, 1.000000000000000000, 1.000000000000000000, 1.000000000000000000, 1.000000000000000000, 1.000000000000000000, 1.000000000000000000, 1.000000000000000000, 1.000000000000000000, 1.000000000000000000, 1.000000000000000000, 1.000000000000000000, 1.000000000000000000, 1.000000000000000000, 1.000000000000000000, 1.000000000000000000, 1.000000000000000000, 1.000000000000000000, 1.000000000000000000, 1.000000000000000000, 1.000000000000000000, 1.000000000000000000, 1.000000000000000000, 1.000000000000000000, 1.000000000000000000, 1.000000000000000000, 1.000000000000000000, 1.000000000000000000, 1.000000000000000000, 1.000000000000000000, 1.000000000000000000, 1.000000000000000000) ) ) 
 REPRESENTATION_ITEM ( '' )  SURFACE ( )  );
#17880 = DIRECTION ( 'NONE',  ( -0.9510565162951536422, -2.566386769018988323E-16, 0.3090169943749475623 ) ) ;
#17881 = CARTESIAN_POINT ( 'NONE',  ( 0.000000000000000000, 0.000000000000000000, 15.00000000000000000 ) ) ;
#17882 = CARTESIAN_POINT ( 'NONE',  ( 12.94178543664954972, 7.512178771719595360, -16.05074886939826939 ) ) ;
#17883 = CARTESIAN_POINT ( 'NONE',  ( 12.49957999542663600, 8.570517509188613658, -15.13050969259218981 ) ) ;
#17884 = CARTESIAN_POINT ( 'NONE',  ( 28.35369828010231785, -12.30166555976806464, -13.00196782638265169 ) ) ;
#17885 = EDGE_LOOP ( 'NONE', ( #16755, #27388, #15538, #8812 ) ) ;
#17886 = FACE_OUTER_BOUND ( 'NONE', #5465, .T. ) ;
#17887 = FACE_BOUND ( 'NONE', #16326, .T. ) ;
#17888 = ORIENTED_EDGE ( 'NONE', *, *, #1892, .T. ) ;
#17889 = CARTESIAN_POINT ( 'NONE',  ( 9.641566850259106758, 17.66790035518494051, -17.86107206016944460 ) ) ;
#17890 = VECTOR ( 'NONE', #14330, 1000.000000000000000 ) ;
#17891 = LINE ( 'NONE', #16479, #413 ) ;
#17892 = CARTESIAN_POINT ( 'NONE',  ( 143.6922820468853956, -10.00000000000000533, 2.247092850131519715 ) ) ;
#17893 = DIRECTION ( 'NONE',  ( 1.000000000000000000, 2.698458740408365879E-16, -1.110223024625156540E-16 ) ) ;
#17895 = ORIENTED_EDGE ( 'NONE', *, *, #10343, .T. ) ;
#17894 = CARTESIAN_POINT ( 'NONE',  ( 24.66978787416869068, -0.3063955544261361963, -14.42797892638687784 ) ) ;
#17896 = EDGE_LOOP ( 'NONE', ( #6701, #22213, #27423, #1993 ) ) ;
#17897 = DIRECTION ( 'NONE',  ( -0.9510565162951536422, -2.566386769018988323E-16, 0.3090169943749475623 ) ) ;
#17898 = CARTESIAN_POINT ( 'NONE',  ( 12.78959314398258940, 9.756708335562493062, -14.89936416525698526 ) ) ;
#17899 = VECTOR ( 'NONE', #20917, 1000.000000000000000 ) ;
#17900 = CARTESIAN_POINT ( 'NONE',  ( 180.7287565553229456, -3.999999999999989786, 0.5000000000000029976 ) ) ;
#17901 = PLANE ( 'NONE',  #23465 ) ;
#17902 = ORIENTED_EDGE ( 'NONE', *, *, #24531, .T. ) ;
#17903 = CARTESIAN_POINT ( 'NONE',  ( 26.87257363757477435, -3.324124212371978082, -16.68573618535388547 ) ) ;
#17904 = CARTESIAN_POINT ( 'NONE',  ( 0.000000000000000000, 5.051668046482832750E-16, -4.000000000000000000 ) ) ;
#17905 = CARTESIAN_POINT ( 'NONE',  ( 24.18628427323349328, -0.8779346998738073449, -17.06787597161793357 ) ) ;
#17906 = ORIENTED_EDGE ( 'NONE', *, *, #23807, .T. ) ;
#17907 = DIRECTION ( 'NONE',  ( -2.698458740408365879E-16, 1.000000000000000000, 0.000000000000000000 ) ) ;
#17908 = EDGE_LOOP ( 'NONE', ( #24162, #1264, #6510, #24053 ) ) ;
#17909 = CARTESIAN_POINT ( 'NONE',  ( 25.74126694659371495, -13.30326880535473322, -17.45270501867052104 ) ) ;
#17910 = CARTESIAN_POINT ( 'NONE',  ( 29.62334656761623819, -11.49549692320935890, -13.92735753183835712 ) ) ;
#17911 = VERTEX_POINT ( 'NONE', #23420 ) ;
#17912 = ORIENTED_EDGE ( 'NONE', *, *, #29655, .T. ) ;
#17913 = EDGE_CURVE ( 'NONE', #6453, #5386, #2537, .T. ) ;
#17914 = EDGE_CURVE ( 'NONE', #7269, #653, #29904, .T. ) ;
#17915 = CARTESIAN_POINT ( 'NONE',  ( 29.66490191837812773, -8.365349891895018430, -17.62461620872172574 ) ) ;
#17916 = EDGE_CURVE ( 'NONE', #18174, #2968, #27890, .T. ) ;
#17917 = AXIS2_PLACEMENT_3D ( 'NONE', #10360, #26263, #5187 ) ;
#17918 = LINE ( 'NONE', #22212, #16239 ) ;
#17919 = VERTEX_POINT ( 'NONE', #16085 ) ;
#17920 = DIRECTION ( 'NONE',  ( 0.3090169943749472292, 8.338696094057992503E-17, -0.9510565162951536422 ) ) ;
#17921 = AXIS2_PLACEMENT_3D ( 'NONE', #20763, #20469, #11010 ) ;
#17922 = LINE ( 'NONE', #27298, #25263 ) ;
#17923 = DIRECTION ( 'NONE',  ( -0.5877852522924731371, -1.586114251531760728E-16, -0.8090169943749474513 ) ) ;
#17924 = DIRECTION ( 'NONE',  ( -1.000000000000000000, 0.000000000000000000, -0.000000000000000000 ) ) ;
#17925 = CARTESIAN_POINT ( 'NONE',  ( 25.85400256215867643, -3.413040292952954413, -16.90843739280879277 ) ) ;
#17926 = CARTESIAN_POINT ( 'NONE',  ( 19.82332968365342296, 2.432204761014481242, -19.52120720162773537 ) ) ;
#17928 = VERTEX_POINT ( 'NONE', #25410 ) ;
#17927 = CARTESIAN_POINT ( 'NONE',  ( 32.57905638361870615, -9.615828745292011703, -17.95267489271534700 ) ) ;
#17929 = VECTOR ( 'NONE', #28762, 1000.000000000000000 ) ;
#17930 = DIRECTION ( 'NONE',  ( 0.000000000000000000, 0.000000000000000000, -1.000000000000000000 ) ) ;
#17931 = CARTESIAN_POINT ( 'NONE',  ( 11.47155695691762212, 9.275332456566969697, -15.86145787682774078 ) ) ;
#17932 = FACE_OUTER_BOUND ( 'NONE', #10960, .T. ) ;
#17933 = DIRECTION ( 'NONE',  ( 1.000000000000000000, 0.000000000000000000, 0.000000000000000000 ) ) ;
#17934 = CARTESIAN_POINT ( 'NONE',  ( 13.66828981435543078, 8.811555337407297017, -15.47779131845255307 ) ) ;
#17935 = PLANE ( 'NONE',  #5373 ) ;
#17936 = ORIENTED_EDGE ( 'NONE', *, *, #18210, .F. ) ;
#17937 = DIRECTION ( 'NONE',  ( -0.000000000000000000, -0.000000000000000000, -1.000000000000000000 ) ) ;
#17938 = CARTESIAN_POINT ( 'NONE',  ( 12.43696608443014284, 8.546664718661613591, -15.18012293544581226 ) ) ;
#17939 = ORIENTED_EDGE ( 'NONE', *, *, #15965, .T. ) ;
#17940 = DIRECTION ( 'NONE',  ( 0.5877852522924731371, 1.586114251531760728E-16, 0.8090169943749474513 ) ) ;
#17941 = LINE ( 'NONE', #27316, #20042 ) ;
#17942 = AXIS2_PLACEMENT_3D ( 'NONE', #3811, #4110, #24570 ) ;
#17943 = DIRECTION ( 'NONE',  ( -2.698458740408365879E-16, 1.000000000000000000, 0.000000000000000000 ) ) ;
#17944 = ORIENTED_EDGE ( 'NONE', *, *, #3951, .T. ) ;
#17945 = CARTESIAN_POINT ( 'NONE',  ( 8.946690830082905777, 16.94193370358561879, -17.78270686867927708 ) ) ;
#17946 = CARTESIAN_POINT ( 'NONE',  ( 31.95629010954621663, -10.29636179124881679, -18.42443288805318247 ) ) ;
#17947 = VECTOR ( 'NONE', #15055, 1000.000000000000000 ) ;
#17948 = CARTESIAN_POINT ( 'NONE',  ( 19.77504133826384347, 1.335633644655777053, -20.04176789066487530 ) ) ;
#17949 = CARTESIAN_POINT ( 'NONE',  ( 26.09074415779471323, -5.786596670875995940, -12.76770422508296932 ) ) ;
#17950 = LINE ( 'NONE', #6382, #16011 ) ;
#17951 = AXIS2_PLACEMENT_3D ( 'NONE', #1660, #8503, #22245 ) ;
#17952 = DIRECTION ( 'NONE',  ( 0.5877852522924731371, 0.000000000000000000, 0.8090169943749474513 ) ) ;
#17953 = CARTESIAN_POINT ( 'NONE',  ( 25.20506945179333513, 0.8918220058822420304, -17.26233558910082166 ) ) ;
#17954 = ADVANCED_FACE ( 'NONE', ( #25552 ), #4646, .T. ) ;
#17955 = VECTOR ( 'NONE', #27963, 999.9999999999998863 ) ;
#17956 = ADVANCED_FACE ( 'NONE', ( #8912 ), #25111, .T. ) ;
#17957 = ADVANCED_FACE ( 'NONE', ( #18228 ), #13792, .T. ) ;
#17958 = VERTEX_POINT ( 'NONE', #15937 ) ;
#17959 = EDGE_CURVE ( 'NONE', #19510, #6258, #24554, .T. ) ;
#17960 = CARTESIAN_POINT ( 'NONE',  ( 158.6922820468853388, -1.999999999999974021, -6.413161187712876909 ) ) ;
#17962 = ORIENTED_EDGE ( 'NONE', *, *, #30234, .T. ) ;
#17961 = CYLINDRICAL_SURFACE ( 'NONE', #16052, 8.000000000000000000 ) ;
#17963 = CARTESIAN_POINT ( 'NONE',  ( 420.0000000000002274, 34.64101615137744972, 10.00000000000000178 ) ) ;
#17964 = CARTESIAN_POINT ( 'NONE',  ( 0.000000000000000000, 0.000000000000000000, -2.450000000000000178 ) ) ;
#17965 = PLANE ( 'NONE',  #20935 ) ;
#17966 = EDGE_LOOP ( 'NONE', ( #6444, #15307, #19730, #22351 ) ) ;
#17967 = CARTESIAN_POINT ( 'NONE',  ( 35.54859390953724585, -21.18451583373416014, -16.94733705004010105 ) ) ;
#17968 = AXIS2_PLACEMENT_3D ( 'NONE', #1659, #10937, #22404 ) ;
#17969 = ORIENTED_EDGE ( 'NONE', *, *, #17005, .F. ) ;
#17970 = CARTESIAN_POINT ( 'NONE',  ( 12.75399582221978889, 7.624919616107145970, -14.92773571455457216 ) ) ;
#17971 = EDGE_LOOP ( 'NONE', ( #21513, #21388, #20686, #16336 ) ) ;
#17972 = CARTESIAN_POINT ( 'NONE',  ( 25.97256211245905533, -8.171536508395311316, -18.54953510021574559 ) ) ;
#17973 = DIRECTION ( 'NONE',  ( -1.110223024625156540E-16, 0.000000000000000000, -1.000000000000000000 ) ) ;
#17974 = CARTESIAN_POINT ( 'NONE',  ( 10.35864917552468611, 16.97212507441191320, -17.91611982430173455 ) ) ;
#17975 = CARTESIAN_POINT ( 'NONE',  ( 130.7287565553229456, -10.00000000000000888, -13.44584919360586284 ) ) ;
#17976 = VECTOR ( 'NONE', #6079, 1000.000000000000000 ) ;
#17977 = ORIENTED_EDGE ( 'NONE', *, *, #14480, .F. ) ;
#17978 = LINE ( 'NONE', #15077, #7584 ) ;
#17979 = CARTESIAN_POINT ( 'NONE',  ( 12.71834232392635045, 8.667191563245470576, -14.95615232649864090 ) ) ;
#17980 = DIRECTION ( 'NONE',  ( -0.9510565162951536422, -2.566386769018988323E-16, 0.3090169943749475623 ) ) ;
#17981 = ORIENTED_EDGE ( 'NONE', *, *, #4600, .T. ) ;
#17982 = CARTESIAN_POINT ( 'NONE',  ( -7.999999999999998224, -0.7805016046291078924, 1.123165688059202250E-15 ) ) ;
#17983 = ORIENTED_EDGE ( 'NONE', *, *, #20922, .T. ) ;
#17984 = CARTESIAN_POINT ( 'NONE',  ( 9.661885998671275289, 16.25481316389105402, -17.91482063482849441 ) ) ;
#17985 = VERTEX_POINT ( 'NONE', #30046 ) ;
#17986 = CARTESIAN_POINT ( 'NONE',  ( 25.05533511103952904, -1.369129923259265524, -16.98221401193426416 ) ) ;
#17987 = CARTESIAN_POINT ( 'NONE',  ( 22.35254782987788147, 5.884919045556002537, -15.62344653218675283 ) ) ;
#17988 = VECTOR ( 'NONE', #30177, 1000.000000000000000 ) ;
#17989 = CARTESIAN_POINT ( 'NONE',  ( 2.500000000000000444, -1.178949249685215417, 2.042000000000002036 ) ) ;
#17990 = ORIENTED_EDGE ( 'NONE', *, *, #23562, .T. ) ;
#17991 = PLANE ( 'NONE',  #15214 ) ;
#17992 = VECTOR ( 'NONE', #5215, 1000.000000000000000 ) ;
#17993 = CARTESIAN_POINT ( 'NONE',  ( 19.18841159021359033, -2.222386543571284179, -18.22349448661670834 ) ) ;
#17994 = ADVANCED_FACE ( 'NONE', ( #19281 ), #26325, .F. ) ;
#17995 = ADVANCED_FACE ( 'NONE', ( #5100 ), #17149, .T. ) ;
#17996 = EDGE_CURVE ( 'NONE', #23960, #1065, #28638, .T. ) ;
#17997 = ORIENTED_EDGE ( 'NONE', *, *, #10522, .T. ) ;
#17998 = VECTOR ( 'NONE', #15677, 1000.000000000000000 ) ;
#17999 = FACE_OUTER_BOUND ( 'NONE', #4270, .T. ) ;
#18000 = EDGE_CURVE ( 'NONE', #14962, #2433, #186, .T. ) ;
#18001 = DIRECTION ( 'NONE',  ( 0.000000000000000000, 0.000000000000000000, 1.000000000000000000 ) ) ;
#18002 = ORIENTED_EDGE ( 'NONE', *, *, #14652, .T. ) ;
#18003 = VERTEX_POINT ( 'NONE', #10119 ) ;
#18004 = CARTESIAN_POINT ( 'NONE',  ( 130.7287565553229456, -4.999999999999983125, 3.500000000000003109 ) ) ;
#18005 = CARTESIAN_POINT ( 'NONE',  ( 33.47012763672258728, -12.84706786418751534, -19.72967806864707541 ) ) ;
#18006 = FACE_OUTER_BOUND ( 'NONE', #20174, .T. ) ;
#18007 = EDGE_LOOP ( 'NONE', ( #22554, #1423, #8307, #23403 ) ) ;
#18008 = ORIENTED_EDGE ( 'NONE', *, *, #27650, .F. ) ;
#18009 = CARTESIAN_POINT ( 'NONE',  ( 141.1922820468854525, -1.999999999999978684, -30.91696583120935671 ) ) ;
#18010 = CARTESIAN_POINT ( 'NONE',  ( 30.43753979984721525, -10.17066761781405937, -14.50402091508011537 ) ) ;
#18011 = CARTESIAN_POINT ( 'NONE',  ( 12.24557421509628519, 9.516296637964343219, -15.33295685416265286 ) ) ;
#18012 = CARTESIAN_POINT ( 'NONE',  ( 35.07504771885155037, -20.05712364337910714, -20.21480690768607857 ) ) ;
#18013 = AXIS2_PLACEMENT_3D ( 'NONE', #24926, #29860, #27992 ) ;
#18014 = AXIS2_PLACEMENT_3D ( 'NONE', #29840, #2156, #23057 ) ;
#18015 = ORIENTED_EDGE ( 'NONE', *, *, #11656, .T. ) ;
#18016 = FACE_OUTER_BOUND ( 'NONE', #6943, .T. ) ;
#18017 = VECTOR ( 'NONE', #9177, 1000.000000000000000 ) ;
#18018 = CARTESIAN_POINT ( 'NONE',  ( 9.641350810849047548, 17.66889113945805789, -17.97192418671891190 ) ) ;
#18019 = DIRECTION ( 'NONE',  ( -1.000000000000000000, 0.000000000000000000, -0.000000000000000000 ) ) ;
#18020 = PRESENTATION_STYLE_ASSIGNMENT (( #20156 ) ) ;
#18021 = VECTOR ( 'NONE', #19690, 1000.000000000000000 ) ;
#18022 = ORIENTED_EDGE ( 'NONE', *, *, #11318, .T. ) ;
#18023 = PRESENTATION_LAYER_ASSIGNMENT (  '', '', ( #14118 ) ) ;
#18024 = CARTESIAN_POINT ( 'NONE',  ( 107.4261961205572931, -4.999999999999988454, -78.04970010342938735 ) ) ;
#18025 = ORIENTED_EDGE ( 'NONE', *, *, #27450, .F. ) ;
#18026 = CARTESIAN_POINT ( 'NONE',  ( 10.35864927600819740, 16.97212461358170188, -17.91506874352199574 ) ) ;
#18027 = CARTESIAN_POINT ( 'NONE',  ( 32.35289370704636980, -10.23129387835982129, -15.31177623828282108 ) ) ;
#18028 = CARTESIAN_POINT ( 'NONE',  ( 21.63873165585565417, 2.424707942738766331, -13.54651715722292060 ) ) ;
#18029 = ORIENTED_EDGE ( 'NONE', *, *, #20441, .T. ) ;
#18030 = CARTESIAN_POINT ( 'NONE',  ( 159.5152310637605240, -9.999999999999998224, -19.94844914048349693 ) ) ;
#18031 = CARTESIAN_POINT ( 'NONE',  ( 2.500000000000000444, 1.178949249685215417, -2.042000000000002036 ) ) ;
#18032 = CARTESIAN_POINT ( 'NONE',  ( 27.03959252790357581, -7.665547941290169476, -19.57376043866218041 ) ) ;
#18033 = VECTOR ( 'NONE', #14813, 1000.000000000000000 ) ;
#18034 = CARTESIAN_POINT ( 'NONE',  ( 24.43881766525553090, -7.056818123010307531, -19.17719463634885102 ) ) ;
#18035 = EDGE_CURVE ( 'NONE', #17865, #18212, #16997, .T. ) ;
#18037 = VERTEX_POINT ( 'NONE', #12406 ) ;
#18036 = EDGE_CURVE ( 'NONE', #7426, #2040, #9508, .T. ) ;
#18038 = CARTESIAN_POINT ( 'NONE',  ( 157.2287565553229740, -10.00000000000000000, -20.83012701892220520 ) ) ;
#18039 = VECTOR ( 'NONE', #7819, 1000.000000000000000 ) ;
#18040 = CARTESIAN_POINT ( 'NONE',  ( 152.0152310637605808, -1.999999999999974909, -24.27857615940569502 ) ) ;
#18041 = DIRECTION ( 'NONE',  ( 0.5877852522924731371, 1.586114251531760728E-16, 0.8090169943749474513 ) ) ;
#18042 = CARTESIAN_POINT ( 'NONE',  ( 141.1922820468854525, -1.999999999999978684, -10.74328820663507678 ) ) ;
#18043 = UNCERTAINTY_MEASURE_WITH_UNIT (LENGTH_MEASURE( 1.000000000000000082E-05 ), #29441, 'distance_accuracy_value', 'NONE');
#18044 = CARTESIAN_POINT ( 'NONE',  ( 11.22879857168519813, 9.069188343361037852, -17.23954317433854300 ) ) ;
#18045 = CARTESIAN_POINT ( 'NONE',  ( 12.77278825050581013, 8.691252192278360766, -14.91275796197543890 ) ) ;
#18047 = CONICAL_SURFACE ( 'NONE', #1024, 5.000000000000000888, 0.7853981633974456145 ) ;
#18046 = LINE ( 'NONE', #17742, #16012 ) ;
#18048 = VECTOR ( 'NONE', #12875, 1000.000000000000000 ) ;
#18049 = VERTEX_POINT ( 'NONE', #5407 ) ;
#18050 = DIRECTION ( 'NONE',  ( 0.000000000000000000, 0.000000000000000000, -1.000000000000000000 ) ) ;
#18051 = EDGE_LOOP ( 'NONE', ( #4563, #4671, #16719, #15070, #26620 ) ) ;
#18052 = VECTOR ( 'NONE', #20096, 1000.000000000000000 ) ;
#18053 = CARTESIAN_POINT ( 'NONE',  ( 9.641364314812712166, 17.66882920855936590, -17.90209449470656722 ) ) ;
#18054 = DIRECTION ( 'NONE',  ( 0.9510565162951536422, 2.566386769018988816E-16, 0.3090169943749472292 ) ) ;
#18055 = CARTESIAN_POINT ( 'NONE',  ( 17.06308625499319831, 6.674173717519480853, -15.25088821959635865 ) ) ;
#18056 = CARTESIAN_POINT ( 'NONE',  ( -4.000000000000004441, -0.3902508023145587202, -2.449999999999998401 ) ) ;
#18057 = CARTESIAN_POINT ( 'NONE',  ( 168.6922820468852819, -4.999999999999971578, -0.6060766987539614181 ) ) ;
#18059 = ORIENTED_EDGE ( 'NONE', *, *, #21683, .T. ) ;
#18058 = CARTESIAN_POINT ( 'NONE',  ( 24.14158683625483803, -3.940216521628096658, -13.50644477367014673 ) ) ;
#18060 = ORIENTED_EDGE ( 'NONE', *, *, #13563, .F. ) ;
#18061 = CARTESIAN_POINT ( 'NONE',  ( 130.7287565553229456, -9.999999999999982236, 3.500000000000003109 ) ) ;
#18062 = CARTESIAN_POINT ( 'NONE',  ( 12.25326555804286421, 9.517817489571868350, -15.32696995758615621 ) ) ;
#18063 = EDGE_CURVE ( 'NONE', #11008, #23288, #9966, .T. ) ;
#18064 = VECTOR ( 'NONE', #5173, 1000.000000000000000 ) ;
#18065 = CARTESIAN_POINT ( 'NONE',  ( 35.54502023521215648, -22.16846120802060938, -18.59538644662325524 ) ) ;
#18066 = DIRECTION ( 'NONE',  ( 1.000000000000000000, 0.000000000000000000, 0.000000000000000000 ) ) ;
#18067 = CARTESIAN_POINT ( 'NONE',  ( 21.69765170278760280, -5.035756590920279940, -14.89200278627170881 ) ) ;
#18068 = LINE ( 'NONE', #6333, #28185 ) ;
#18069 = CARTESIAN_POINT ( 'NONE',  ( 21.26848706961299129, -1.060808783303755387, -18.71231287479539063 ) ) ;
#18070 = ORIENTED_EDGE ( 'NONE', *, *, #6862, .T. ) ;
#18071 = CARTESIAN_POINT ( 'NONE',  ( 139.5152310637606092, -10.00000000000000533, -28.60870317832789311 ) ) ;
#18072 = SURFACE_STYLE_FILL_AREA ( #18222 ) ;
#18073 = CARTESIAN_POINT ( 'NONE',  ( 32.57950401048368150, -10.91418750421072659, -13.94906786461360504 ) ) ;
#18074 = CARTESIAN_POINT ( 'NONE',  ( 30.18376337559066158, -9.479172175342087669, -16.86143889264288021 ) ) ;
#18075 = EDGE_CURVE ( 'NONE', #12812, #26944, #26478, .T. ) ;
#18076 = VERTEX_POINT ( 'NONE', #4951 ) ;
#18077 = VECTOR ( 'NONE', #22841, 1000.000000000000000 ) ;
#18078 = PLANE ( 'NONE',  #2952 ) ;
#18079 = CONICAL_SURFACE ( 'NONE', #21987, 5.999999999999970690, 0.7853981633974530530 ) ;
#18080 = CARTESIAN_POINT ( 'NONE',  ( 147.0152310637606092, -10.00000000000000178, -32.93883019725009120 ) ) ;
#18081 =( GEOMETRIC_REPRESENTATION_CONTEXT ( 3 ) GLOBAL_UNCERTAINTY_ASSIGNED_CONTEXT ( ( #22336 ) ) GLOBAL_UNIT_ASSIGNED_CONTEXT ( ( #24465, #22167, #26469 ) ) REPRESENTATION_CONTEXT ( 'NONE', 'WORKASPACE' ) );
#18082 = FACE_OUTER_BOUND ( 'NONE', #8394, .T. ) ;
#18083 = DIRECTION ( 'NONE',  ( -1.110223024625156540E-16, 0.000000000000000000, -1.000000000000000000 ) ) ;
#18084 = LINE ( 'NONE', #10770, #18727 ) ;
#18085 = CARTESIAN_POINT ( 'NONE',  ( 4.000000000000008882, -6.928203230275510549, 0.000000000000000000 ) ) ;
#18086 = CARTESIAN_POINT ( 'NONE',  ( 24.46642504186807088, -8.279991823955473507, -18.31266784446766493 ) ) ;
#18087 = CARTESIAN_POINT ( 'NONE',  ( 19.92565466131104301, 6.686648131885553958, -19.16379146452587179 ) ) ;
#18088 = CARTESIAN_POINT ( 'NONE',  ( 36.06101586692013683, -20.99408596552883566, -21.31372499146719690 ) ) ;
#18089 = CARTESIAN_POINT ( 'NONE',  ( 0.3263565795980569728, -4.430380094434312355, -0.2484800633750388621 ) ) ;
#18090 = CARTESIAN_POINT ( 'NONE',  ( 12.49977518293622758, 8.570603418560722275, -15.13035415120363325 ) ) ;
#18091 = CARTESIAN_POINT ( 'NONE',  ( 0.000000000000000000, 0.000000000000000000, 2.549999999999998490 ) ) ;
#18092 = CARTESIAN_POINT ( 'NONE',  ( 174.5152310637604103, -9.999999999999994671, -2.627941064794695691 ) ) ;
#18093 = CARTESIAN_POINT ( 'NONE',  ( 9.700291501659986437, 16.07868063162199945, -17.87166786738998780 ) ) ;
#18094 = CARTESIAN_POINT ( 'NONE',  ( 2.309976723937609666, -7.903938623646900474, -4.869346954796172966 ) ) ;
#18095 = ORIENTED_EDGE ( 'NONE', *, *, #22760, .F. ) ;
#18096 = CARTESIAN_POINT ( 'NONE',  ( 0.000000000000000000, 55.00000000000000711, 23.00000000000000000 ) ) ;
#18097 = AXIS2_PLACEMENT_3D ( 'NONE', #19150, #16859, #26803 ) ;
#18098 = CARTESIAN_POINT ( 'NONE',  ( 12.53458732174692258, 8.585986940276173485, -15.10260830673100330 ) ) ;
#18099 = EDGE_CURVE ( 'NONE', #20136, #16501, #19133, .T. ) ;
#18100 = VERTEX_POINT ( 'NONE', #7402 ) ;
#18101 = LINE ( 'NONE', #2400, #27143 ) ;
#18102 = DIRECTION ( 'NONE',  ( -2.698458740408365879E-16, 1.000000000000000000, 0.000000000000000000 ) ) ;
#18103 = ADVANCED_FACE ( 'NONE', ( #5251 ), #5559, .T. ) ;
#18104 = DIRECTION ( 'NONE',  ( 0.5877852522924731371, 0.000000000000000000, 0.8090169943749474513 ) ) ;
#18105 = VERTEX_POINT ( 'NONE', #229 ) ;
#18106 = CARTESIAN_POINT ( 'NONE',  ( 13.48814714115247249, 7.673917307032582791, -15.62136820872497545 ) ) ;
#18107 = CARTESIAN_POINT ( 'NONE',  ( 35.94849409650817762, -20.48858525550898335, -21.40790205994406747 ) ) ;
#18108 = CARTESIAN_POINT ( 'NONE',  ( 18.99162967131814028, 0.6168208955672017657, -19.54819510397825510 ) ) ;
#18109 = CARTESIAN_POINT ( 'NONE',  ( 14.93998017692337221, 5.301442995092576105, -18.84457556472494488 ) ) ;
#18110 = PLANE ( 'NONE',  #26960 ) ;
#18111 = CARTESIAN_POINT ( 'NONE',  ( 24.97326132480219485, 0.3353791038140019887, -18.64228740943764961 ) ) ;
#18112 = VERTEX_POINT ( 'NONE', #14241 ) ;
#18113 = LINE ( 'NONE', #22713, #6008 ) ;
#18115 = ORIENTED_EDGE ( 'NONE', *, *, #28303, .F. ) ;
#18114 = DIRECTION ( 'NONE',  ( -0.9510565162951536422, -2.566386769018988816E-16, -0.3090169943749472292 ) ) ;
#18116 =( LENGTH_UNIT ( ) NAMED_UNIT ( * ) SI_UNIT ( .MILLI., .METRE. ) );
#18117 = CARTESIAN_POINT ( 'NONE',  ( 173.6922820468852535, -9.999999999999996447, -0.6060766987539614181 ) ) ;
#18118 = DIRECTION ( 'NONE',  ( -0.9510565162951536422, 0.000000000000000000, -0.3090169943749472292 ) ) ;
#18119 = CARTESIAN_POINT ( 'NONE',  ( 33.96051107771264554, -11.12695408846492739, -17.85276550113785277 ) ) ;
#18120 = ORIENTED_EDGE ( 'NONE', *, *, #439, .T. ) ;
#18121 = CARTESIAN_POINT ( 'NONE',  ( 10.66927416475804158, 9.041953549878499530, -16.41095583421565962 ) ) ;
#18122 = PRODUCT ( 'torque nut 08_iso_ISO 10511-M5-N', 'torque nut 08_iso_ISO 10511-M5-N', '', ( #13751 ) ) ;
#18123 = VERTEX_POINT ( 'NONE', #18832 ) ;
#18124 = CARTESIAN_POINT ( 'NONE',  ( 29.66490191837812773, -8.365349891895018430, -17.62461620872172574 ) ) ;
#18125 = LINE ( 'NONE', #6994, #8920 ) ;
#18126 = CARTESIAN_POINT ( 'NONE',  ( 12.87691298531170148, 9.519861518574414205, -16.10853261994384411 ) ) ;
#18127 = FACE_OUTER_BOUND ( 'NONE', #11152, .T. ) ;
#18128 = ORIENTED_EDGE ( 'NONE', *, *, #14907, .T. ) ;
#18129 = ORIENTED_EDGE ( 'NONE', *, *, #22074, .T. ) ;
#18130 = ADVANCED_FACE ( 'NONE', ( #11948 ), #12262, .T. ) ;
#18131 = VERTEX_POINT ( 'NONE', #16703 ) ;
#18132 = LINE ( 'NONE', #6548, #24656 ) ;
#18133 = EDGE_CURVE ( 'NONE', #8000, #5008, #16547, .T. ) ;
#18134 = CARTESIAN_POINT ( 'NONE',  ( 12.50906579366657390, 8.574708520419219937, -15.12294941509656354 ) ) ;
#18137 = ORIENTED_EDGE ( 'NONE', *, *, #8149, .F. ) ;
#18136 = PLANE ( 'NONE',  #5258 ) ;
#18135 = VECTOR ( 'NONE', #25780, 1000.000000000000000 ) ;
#18138 = EDGE_CURVE ( 'NONE', #4340, #27514, #2669, .T. ) ;
#18139 = ORIENTED_EDGE ( 'NONE', *, *, #11070, .T. ) ;
#18140 = DIRECTION ( 'NONE',  ( 0.9510565162951536422, 0.000000000000000000, -0.3090169943749475623 ) ) ;
#18141 = EDGE_LOOP ( 'NONE', ( #16325, #18639, #12582, #2181 ) ) ;
#18142 = CARTESIAN_POINT ( 'NONE',  ( 13.15105351193492744, 8.582979361647906202, -15.89003778131599098 ) ) ;
#18143 = CARTESIAN_POINT ( 'NONE',  ( 17.73099166324444553, -0.3602181158183791476, -14.74723639357852178 ) ) ;
#18144 = CARTESIAN_POINT ( 'NONE',  ( 22.18718699900398761, -4.329393945612883599, -17.49580572735151307 ) ) ;
#18145 = VERTEX_POINT ( 'NONE', #381 ) ;
#18146 = CARTESIAN_POINT ( 'NONE',  ( 19.36978511310259421, 2.022953856625822944, -19.43459320487130171 ) ) ;
#18147 = CARTESIAN_POINT ( 'NONE',  ( -11.85189716074913058, -5.341585316273319783, 4.999999999999998224 ) ) ;
#18148 = LINE ( 'NONE', #22898, #11316 ) ;
#18149 = CARTESIAN_POINT ( 'NONE',  ( 19.68115760211910725, 3.144890361740488860, -20.29587546762095940 ) ) ;
#18150 = VECTOR ( 'NONE', #4277, 1000.000000000000000 ) ;
#18151 = VERTEX_POINT ( 'NONE', #23728 ) ;
#18152 = DIRECTION ( 'NONE',  ( -0.7071067811865492381, -1.962615573354713720E-17, 0.7071067811865457964 ) ) ;
#18153 = CARTESIAN_POINT ( 'NONE',  ( 147.2287565553230309, -10.00000000000000178, -20.83012701892220520 ) ) ;
#18154 = VECTOR ( 'NONE', #10338, 1000.000000000000000 ) ;
#18155 = ORIENTED_EDGE ( 'NONE', *, *, #25376, .F. ) ;
#18156 = EDGE_CURVE ( 'NONE', #16318, #1647, #26025, .T. ) ;
#18157 = LINE ( 'NONE', #25190, #9229 ) ;
#18158 = CARTESIAN_POINT ( 'NONE',  ( 35.45944968151609800, -21.78403803824750185, -19.54251958818673174 ) ) ;
#18159 = DIRECTION ( 'NONE',  ( -0.9510565162951536422, 0.000000000000000000, -0.3090169943749472292 ) ) ;
#18160 = ORIENTED_EDGE ( 'NONE', *, *, #5897, .F. ) ;
#18161 = ORIENTED_EDGE ( 'NONE', *, *, #6372, .F. ) ;
#18162 = LINE ( 'NONE', #11432, #5133 ) ;
#18163 = CARTESIAN_POINT ( 'NONE',  ( 18.55171814111300321, 6.637122934506423988, -19.73184648383247364 ) ) ;
#18164 = CARTESIAN_POINT ( 'NONE',  ( 11.05541531668977662, 17.68942339022145305, -23.00000000000000711 ) ) ;
#18165 = CARTESIAN_POINT ( 'NONE',  ( 35.54787733059053778, -22.18129662410796854, -18.46719521006932396 ) ) ;
#18166 = ORIENTED_EDGE ( 'NONE', *, *, #14134, .T. ) ;
#18167 = DIRECTION ( 'NONE',  ( -0.9510565162951536422, 0.000000000000000000, -0.3090169943749472292 ) ) ;
#18168 = EDGE_CURVE ( 'NONE', #4109, #28929, #21429, .T. ) ;
#18169 = CARTESIAN_POINT ( 'NONE',  ( 9.641350810849047548, 17.66889113945805789, -23.00000000000000711 ) ) ;
#18170 = LINE ( 'NONE', #2324, #29836 ) ;
#18171 = CARTESIAN_POINT ( 'NONE',  ( 2.928571428571432378, 1.300546971703755312E-15, 9.480888224575629408 ) ) ;
#18172 = EDGE_CURVE ( 'NONE', #19263, #17861, #21874, .T. ) ;
#18173 = EDGE_CURVE ( 'NONE', #5025, #5499, #10869, .T. ) ;
#18174 = VERTEX_POINT ( 'NONE', #15452 ) ;
#18175 = CARTESIAN_POINT ( 'NONE',  ( 156.1922820468854241, -1.999999999999973577, -28.06379628232387802 ) ) ;
#18176 = EDGE_CURVE ( 'NONE', #17207, #29150, #17591, .T. ) ;
#18177 = VERTEX_POINT ( 'NONE', #24326 ) ;
#18178 = CARTESIAN_POINT ( 'NONE',  ( 12.86830129319110405, 9.516055860257337073, -16.11539629037995169 ) ) ;
#18179 = CARTESIAN_POINT ( 'NONE',  ( 36.54816482920796972, -21.18258820310476409, -18.41547799146826847 ) ) ;
#18180 = CARTESIAN_POINT ( 'NONE',  ( 17.36512755686010934, 0.5347363583120325892, -15.24149349723765390 ) ) ;
#18181 = DIRECTION ( 'NONE',  ( 2.908569913943825554E-16, -1.000000000000000000, 0.000000000000000000 ) ) ;
#18182 = ORIENTED_EDGE ( 'NONE', *, *, #9838, .T. ) ;
#18183 = VECTOR ( 'NONE', #9999, 1000.000000000000000 ) ;
#18184 = CARTESIAN_POINT ( 'NONE',  ( 141.1922820468854525, -10.00000000000000533, -19.40354224447947473 ) ) ;
#18185 = CARTESIAN_POINT ( 'NONE',  ( 0.000000000000000000, 0.000000000000000000, 0.000000000000000000 ) ) ;
#18186 = CARTESIAN_POINT ( 'NONE',  ( 28.96558774451377971, -5.053040458581501859, -15.93506438242870971 ) ) ;
#18187 = CARTESIAN_POINT ( 'NONE',  ( 27.68278592340041655, -3.068913841971319112, -15.41105173719521915 ) ) ;
#18188 = ORIENTED_EDGE ( 'NONE', *, *, #1806, .F. ) ;
#18189 = CIRCLE ( 'NONE', #669, 13.00000000000000178 ) ;
#18190 = LINE ( 'NONE', #6755, #3037 ) ;
#18191 = LINE ( 'NONE', #15292, #27187 ) ;
#18192 = DIRECTION ( 'NONE',  ( -0.5877852522924731371, -1.586114251531760235E-16, 0.8090169943749474513 ) ) ;
#18193 = DIRECTION ( 'NONE',  ( 1.000000000000000000, 2.891205793294675861E-16, 0.000000000000000000 ) ) ;
#18194 = VECTOR ( 'NONE', #29559, 1000.000000000000000 ) ;
#18195 = CARTESIAN_POINT ( 'NONE',  ( 12.29195110325218288, 8.516770644378290456, -15.29309475950548958 ) ) ;
#18196 = CARTESIAN_POINT ( 'NONE',  ( 6.938893903907228378E-15, 60.00000000000000711, -12.50000000000001066 ) ) ;
#18197 = ORIENTED_EDGE ( 'NONE', *, *, #21558, .F. ) ;
#18198 = CARTESIAN_POINT ( 'NONE',  ( 49.00000000000000000, 4.735455214955321593E-16, 5.000000000000000888 ) ) ;
#18199 = ORIENTED_EDGE ( 'NONE', *, *, #19437, .F. ) ;
#18200 = CARTESIAN_POINT ( 'NONE',  ( 9.642214727206800617, 17.66492910891761525, -17.80644250212319690 ) ) ;
#18201 = EDGE_CURVE ( 'NONE', #27047, #18859, #17437, .T. ) ;
#18202 = CARTESIAN_POINT ( 'NONE',  ( 14.32261721435726542, 8.042684561749755545, -14.95628083625202542 ) ) ;
#18203 = PLANE ( 'NONE',  #11216 ) ;
#18204 = DIRECTION ( 'NONE',  ( -0.9510565162951536422, 0.000000000000000000, -0.3090169943749472292 ) ) ;
#18205 = EDGE_CURVE ( 'NONE', #16252, #20351, #1591, .T. ) ;
#18207 = EDGE_LOOP ( 'NONE', ( #11797, #21108, #18892 ) ) ;
#18206 = CARTESIAN_POINT ( 'NONE',  ( 26.47492910780048447, -3.130564378024159211, -15.09640780237150892 ) ) ;
#18208 = ORIENTED_EDGE ( 'NONE', *, *, #25485, .T. ) ;
#18209 = DIRECTION ( 'NONE',  ( -2.698458740408365879E-16, 1.000000000000000000, 0.000000000000000000 ) ) ;
#18210 = EDGE_CURVE ( 'NONE', #9707, #22500, #22030, .T. ) ;
#18211 = CARTESIAN_POINT ( 'NONE',  ( 12.24503583471362234, 9.516058715885376884, -15.33338595299508889 ) ) ;
#18212 = VERTEX_POINT ( 'NONE', #22175 ) ;
#18213 = CARTESIAN_POINT ( 'NONE',  ( 35.45944968151609800, -21.78403803824750185, -19.54251958818673174 ) ) ;
#18214 = CARTESIAN_POINT ( 'NONE',  ( 162.2287565553229172, -4.999999999999973355, -20.83012701892220164 ) ) ;
#18215 = ORIENTED_EDGE ( 'NONE', *, *, #22873, .T. ) ;
#18216 = CARTESIAN_POINT ( 'NONE',  ( 23.77086030874127687, -7.150112426529108944, -14.59934731766091431 ) ) ;
#18217 = LINE ( 'NONE', #9043, #27699 ) ;
#18218 = CARTESIAN_POINT ( 'NONE',  ( 22.08459858401872467, -3.550466661657427636, -14.88928395763347723 ) ) ;
#18219 = ORIENTED_EDGE ( 'NONE', *, *, #20034, .T. ) ;
#18220 = FACE_OUTER_BOUND ( 'NONE', #27478, .T. ) ;
#18221 = VERTEX_POINT ( 'NONE', #1284 ) ;
#18222 = FILL_AREA_STYLE ('',( #29896 ) ) ;
#18223 = CARTESIAN_POINT ( 'NONE',  ( 13.98191416104776685, 5.331502061239655532, -16.22335970869868760 ) ) ;
#18224 = CARTESIAN_POINT ( 'NONE',  ( 28.93285792728966044, -11.80516759558957673, -13.86517224201260134 ) ) ;
#18225 = CIRCLE ( 'NONE', #18712, 4.000000000000000000 ) ;
#18226 = ORIENTED_EDGE ( 'NONE', *, *, #16659, .F. ) ;
#18227 = CYLINDRICAL_SURFACE ( 'NONE', #3445, 8.000000000000007105 ) ;
#18228 = FACE_OUTER_BOUND ( 'NONE', #19670, .T. ) ;
#18229 = DIRECTION ( 'NONE',  ( 0.9510565162951536422, 0.000000000000000000, -0.3090169943749475623 ) ) ;
#18230 = DIRECTION ( 'NONE',  ( 0.000000000000000000, 0.000000000000000000, -1.000000000000000000 ) ) ;
#18231 = CARTESIAN_POINT ( 'NONE',  ( 161.1922820468853104, -1.999999999999974021, -4.936203717676158398 ) ) ;
#18232 = DIRECTION ( 'NONE',  ( 0.3090169943749475623, 8.338696094058001131E-17, 0.9510565162951536422 ) ) ;
#18233 = CARTESIAN_POINT ( 'NONE',  ( 21.35588827150667512, -4.635113535248831518, -19.58358080364444476 ) ) ;
#18234 = CARTESIAN_POINT ( 'NONE',  ( 21.58357356133149807, 4.347441036859617469, -17.91576365920758107 ) ) ;
#18235 = CARTESIAN_POINT ( 'NONE',  ( 34.08234396701924851, -12.11069646272769162, -20.88346212624082909 ) ) ;
#18236 = CARTESIAN_POINT ( 'NONE',  ( -19.99999999999998934, 60.00000000000000711, 24.99999999999998934 ) ) ;
#18237 = CARTESIAN_POINT ( 'NONE',  ( 11.47310491742633687, 9.268236560789974376, -15.86081749295074594 ) ) ;
#18238 = AXIS2_PLACEMENT_3D ( 'NONE', #14877, #28680, #5596 ) ;
#18239 = DIRECTION ( 'NONE',  ( -0.5877852522924731371, -1.586114251531760235E-16, 0.8090169943749474513 ) ) ;
#18240 = DIRECTION ( 'NONE',  ( 0.9510565162951535312, 2.566386769018988816E-16, -0.3090169943749475623 ) ) ;
#18241 = CARTESIAN_POINT ( 'NONE',  ( 9.667859621686535121, 16.22741736728331929, -17.88507964468380251 ) ) ;
#18242 = ADVANCED_FACE ( 'NONE', ( #24933 ), #6307, .T. ) ;
#18243 = DIRECTION ( 'NONE',  ( 0.9510565162951536422, 0.000000000000000000, -0.3090169943749475623 ) ) ;
#18244 = ORIENTED_EDGE ( 'NONE', *, *, #28694, .T. ) ;
#18245 = DIRECTION ( 'NONE',  ( 0.3090169943749475623, 8.338696094058001131E-17, 0.9510565162951536422 ) ) ;
#18246 = EDGE_CURVE ( 'NONE', #3020, #25860, #24780, .T. ) ;
#18247 = CARTESIAN_POINT ( 'NONE',  ( 12.55500454421123457, 8.595009676161804890, -15.08633542003848049 ) ) ;
#18248 = ORIENTED_EDGE ( 'NONE', *, *, #26932, .T. ) ;
#18249 = CARTESIAN_POINT ( 'NONE',  ( 144.5152310637605524, -1.999999999999977573, -13.05155085951651195 ) ) ;
#18250 = CARTESIAN_POINT ( 'NONE',  ( -22.75000000000017053, 34.64101615137744972, -10.00000000000000000 ) ) ;
#18251 = APPLICATION_CONTEXT ( 'automotive_design' ) ;
#18252 = CARTESIAN_POINT ( 'NONE',  ( 161.1922820468853956, -9.999999999999998224, -28.06379628232387802 ) ) ;
#18253 = ORIENTED_EDGE ( 'NONE', *, *, #4401, .T. ) ;
#18254 = CARTESIAN_POINT ( 'NONE',  ( 9.090073284221231731, 16.28436349189565391, -17.07021669716791124 ) ) ;
#18255 = CARTESIAN_POINT ( 'NONE',  ( 33.19064478275001306, -12.59149944747283989, -20.68751865480438212 ) ) ;
#18256 = CARTESIAN_POINT ( 'NONE',  ( 19.50094987086785636, 1.087406662839465632, -19.92270839898774781 ) ) ;
#18257 = CARTESIAN_POINT ( 'NONE',  ( 19.14730738223925854, 6.711798791111892371, -15.43835307388804701 ) ) ;
#18258 = DIRECTION ( 'NONE',  ( 0.5877852522924731371, 1.586114251531760728E-16, 0.8090169943749474513 ) ) ;
#18259 = CARTESIAN_POINT ( 'NONE',  ( 21.36789492492977871, -4.378045371801569274, -13.15753336270543095 ) ) ;
#18260 = AXIS2_PLACEMENT_3D ( 'NONE', #4166, #2046, #16050 ) ;
#18261 = EDGE_LOOP ( 'NONE', ( #10044, #1300, #26964, #26575 ) ) ;
#18262 = FACE_BOUND ( 'NONE', #28079, .T. ) ;
#18263 = ORIENTED_EDGE ( 'NONE', *, *, #22536, .T. ) ;
#18264 = EDGE_CURVE ( 'NONE', #19635, #18890, #17734, .T. ) ;
#18265 = EDGE_CURVE ( 'NONE', #10473, #22161, #15290, .T. ) ;
#18267 = VERTEX_POINT ( 'NONE', #27255 ) ;
#18266 = CARTESIAN_POINT ( 'NONE',  ( 149.5152310637605524, -4.999999999999976907, -21.71180489736091346 ) ) ;
#18268 = CARTESIAN_POINT ( 'NONE',  ( 129.5152310637605808, -10.00000000000000888, -2.627941064794695691 ) ) ;
#18269 = FACE_OUTER_BOUND ( 'NONE', #4992, .T. ) ;
#18270 = CARTESIAN_POINT ( 'NONE',  ( 34.34130860390597206, -11.59244310827663149, -18.69197402374579653 ) ) ;
#18271 = CARTESIAN_POINT ( 'NONE',  ( 10.67817636951947868, 9.002809132723193386, -16.40714615800424880 ) ) ;
#18272 = ORIENTED_EDGE ( 'NONE', *, *, #12891, .T. ) ;
#18273 = CARTESIAN_POINT ( 'NONE',  ( 28.67486520862709654, -7.888541471525570614, -13.83454100519475105 ) ) ;
#18274 = DIRECTION ( 'NONE',  ( -2.698458740408365879E-16, 1.000000000000000000, 0.000000000000000000 ) ) ;
#18275 = CARTESIAN_POINT ( 'NONE',  ( 10.36219267574928260, 16.95587413069128857, -17.77286471925143019 ) ) ;
#18276 = DIRECTION ( 'NONE',  ( 0.3090169943749475623, 8.338696094058001131E-17, 0.9510565162951536422 ) ) ;
#18277 = PLANE ( 'NONE',  #5708 ) ;
#18278 = ORIENTED_EDGE ( 'NONE', *, *, #7871, .T. ) ;
#18279 = DIRECTION ( 'NONE',  ( -2.698458740408365879E-16, 1.000000000000000000, 0.000000000000000000 ) ) ;
#18280 = VECTOR ( 'NONE', #2464, 1000.000000000000000 ) ;
#18281 = CARTESIAN_POINT ( 'NONE',  ( 154.5152310637605240, -1.999999999999974909, -11.28819510263909542 ) ) ;
#18282 = ORIENTED_EDGE ( 'NONE', *, *, #13448, .T. ) ;
#18283 = ORIENTED_EDGE ( 'NONE', *, *, #17440, .T. ) ;
#18284 = PLANE ( 'NONE',  #11056 ) ;
#18285 = VERTEX_POINT ( 'NONE', #10575 ) ;
#18286 = CARTESIAN_POINT ( 'NONE',  ( 9.748920381043669536, 15.85566239202790406, -17.85155811514292878 ) ) ;
#18287 = CARTESIAN_POINT ( 'NONE',  ( 24.51656338950621361, -2.114370418465405521, -18.20187689272319176 ) ) ;
#18288 = CARTESIAN_POINT ( 'NONE',  ( 24.98402180921622673, -1.135180495641346266, -16.01319527449767932 ) ) ;
#18289 = CARTESIAN_POINT ( 'NONE',  ( 20.51209521231993094, 3.083376493849706801, -19.38174501956431683 ) ) ;
#18290 = DIRECTION ( 'NONE',  ( 0.000000000000000000, 0.000000000000000000, -1.000000000000000000 ) ) ;
#18291 = ORIENTED_EDGE ( 'NONE', *, *, #26932, .F. ) ;
#18292 = CARTESIAN_POINT ( 'NONE',  ( 20.00000000000017053, 43.64101615137744972, 12.00000000000000178 ) ) ;
#18293 = VECTOR ( 'NONE', #29916, 1000.000000000000000 ) ;
#18294 = CARTESIAN_POINT ( 'NONE',  ( 24.00918528248616468, -0.5066965781341161712, -13.81223085940890627 ) ) ;
#18295 = AXIS2_PLACEMENT_3D ( 'NONE', #7892, #21481, #28397 ) ;
#18296 = DIRECTION ( 'NONE',  ( -6.938893903907227392E-16, 0.000000000000000000, -1.000000000000000000 ) ) ;
#18297 = ADVANCED_FACE ( 'NONE', ( #22332 ), #3870, .T. ) ;
#18298 = LINE ( 'NONE', #29974, #26979 ) ;
#18299 = EDGE_CURVE ( 'NONE', #19125, #18552, #19879, .T. ) ;
#18300 = VECTOR ( 'NONE', #26757, 999.9999999999998863 ) ;
#18301 = ADVANCED_FACE ( 'NONE', ( #15142 ), #24623, .T. ) ;
#18302 = VECTOR ( 'NONE', #24676, 1000.000000000000000 ) ;
#18303 = EDGE_CURVE ( 'NONE', #3213, #5949, #5709, .T. ) ;
#18304 = CARTESIAN_POINT ( 'NONE',  ( 10.44197622278032611, 16.58997661396885803, -17.36392598754248695 ) ) ;
#18305 = CARTESIAN_POINT ( 'NONE',  ( 35.54859390953723874, -22.18451583373416014, -15.00000000000000000 ) ) ;
#18306 = CYLINDRICAL_SURFACE ( 'NONE', #4860, 3.000000000000002665 ) ;
#18307 = EDGE_LOOP ( 'NONE', ( #5591, #14451 ) ) ;
#18308 = VERTEX_POINT ( 'NONE', #12709 ) ;
#18309 = DIRECTION ( 'NONE',  ( 0.3090169943749472292, 8.338696094057992503E-17, -0.9510565162951536422 ) ) ;
#18310 = CARTESIAN_POINT ( 'NONE',  ( 14.17177033308128031, 6.273687421093853800, -17.36430109743762173 ) ) ;
#18311 = CARTESIAN_POINT ( 'NONE',  ( 11.24654891281740987, 16.81286035451327265, -16.80493547870787197 ) ) ;
#18312 = CARTESIAN_POINT ( 'NONE',  ( 163.6922820468853956, -9.999999999999998224, -35.24709285013155835 ) ) ;
#18313 = ORIENTED_EDGE ( 'NONE', *, *, #13820, .F. ) ;
#18314 = ORIENTED_EDGE ( 'NONE', *, *, #8280, .T. ) ;
#18315 = CARTESIAN_POINT ( 'NONE',  ( 9.915973561396301150, 16.40943619918981256, -16.50475030878699556 ) ) ;
#18316 = VECTOR ( 'NONE', #29813, 1000.000000000000000 ) ;
#18317 = CARTESIAN_POINT ( 'NONE',  ( 12.75938622741416140, 7.627299838292535661, -14.92343961094405103 ) ) ;
#18318 = DIRECTION ( 'NONE',  ( -1.000000000000000000, 0.000000000000000000, 0.000000000000000000 ) ) ;
#18319 = FILL_AREA_STYLE_COLOUR ( '', #4259 ) ;
#18320 = ORIENTED_EDGE ( 'NONE', *, *, #26567, .T. ) ;
#18321 = CARTESIAN_POINT ( 'NONE',  ( 101.6614607007391982, -4.999999999999989342, 73.86137465823269110 ) ) ;
#18322 = ORIENTED_EDGE ( 'NONE', *, *, #14691, .F. ) ;
#18323 = CARTESIAN_POINT ( 'NONE',  ( 12.97729766242475868, 9.564223303342972216, -16.02852426037668465 ) ) ;
#18325 = CARTESIAN_POINT ( 'NONE',  ( 33.40535544545146251, -10.40465400369240356, -18.27852168438239389 ) ) ;
#18324 = VECTOR ( 'NONE', #2243, 1000.000000000000000 ) ;
#18326 = CARTESIAN_POINT ( 'NONE',  ( 24.14158683625483803, -3.940216521628096658, -13.50644477367014673 ) ) ;
#18327 = ORIENTED_EDGE ( 'NONE', *, *, #5813, .F. ) ;
#18328 = COLOUR_RGB ( '', 0.31764706, 0.68627451, 0.89019608) ;
#18329 = LINE ( 'NONE', #13155, #14506 ) ;
#18330 = PLANE ( 'NONE',  #1584 ) ;
#18331 = SHAPE_REPRESENTATION_RELATIONSHIP ( 'NONE' , 'NONE' ,  #23798, #12376 ) ;
#18332 = CARTESIAN_POINT ( 'NONE',  ( 22.33774198005919587, -7.088069534354142220, -17.87445411435389886 ) ) ;
#18333 = CARTESIAN_POINT ( 'NONE',  ( 24.12676367385581244, 0.3224161365626431741, -13.25522683364457777 ) ) ;
#18334 = ORIENTED_EDGE ( 'NONE', *, *, #1936, .F. ) ;
#18335 = DIRECTION ( 'NONE',  ( 1.110223024625156540E-16, 2.995891024602366092E-32, 1.000000000000000000 ) ) ;
#18336 = ADVANCED_FACE ( 'NONE', ( #13017 ), #1651, .T. ) ;
#18337 = EDGE_CURVE ( 'NONE', #22465, #1603, #29095, .T. ) ;
#18338 = EDGE_CURVE ( 'NONE', #6921, #26865, #10943, .T. ) ;
#18339 = VECTOR ( 'NONE', #28661, 1000.000000000000000 ) ;
#18340 = EDGE_CURVE ( 'NONE', #26457, #1081, #3569, .T. ) ;
#18341 = ORIENTED_EDGE ( 'NONE', *, *, #5551, .T. ) ;
#18342 = DIRECTION ( 'NONE',  ( -0.5877852522924731371, -1.586114251531760728E-16, -0.8090169943749474513 ) ) ;
#18343 = CARTESIAN_POINT ( 'NONE',  ( 19.02732395299416623, -5.000000000000012434, -58.56008168663054647 ) ) ;
#18344 = AXIS2_PLACEMENT_3D ( 'NONE', #11339, #13187, #10887 ) ;
#18345 = CARTESIAN_POINT ( 'NONE',  ( 8.000000000000003553, 4.618802153517037823, -0.7145311798163362926 ) ) ;
#18346 = VECTOR ( 'NONE', #13466, 1000.000000000000000 ) ;
#18347 = UNCERTAINTY_MEASURE_WITH_UNIT (LENGTH_MEASURE( 1.000000000000000082E-05 ), #28940, 'distance_accuracy_value', 'NONE');
#18348 = CARTESIAN_POINT ( 'NONE',  ( 10.72183334705107960, 16.62641715516447150, -15.95376865854981929 ) ) ;
#18349 = CARTESIAN_POINT ( 'NONE',  ( 29.49448338005720416, -10.05855281841770221, -18.88094824714235642 ) ) ;
#18350 = ORIENTED_EDGE ( 'NONE', *, *, #28623, .F. ) ;
#18351 = FACE_BOUND ( 'NONE', #14074, .T. ) ;
#18352 = ORIENTED_EDGE ( 'NONE', *, *, #14608, .F. ) ;
#18353 = CARTESIAN_POINT ( 'NONE',  ( 9.655099948573186097, 17.60583584124798051, -17.48406748397995614 ) ) ;
#18354 = CARTESIAN_POINT ( 'NONE',  ( 18.71812633715165575, 6.658065805436550910, -18.41436643113302551 ) ) ;
#18355 = CARTESIAN_POINT ( 'NONE',  ( 72.52133520196026950, -4.999999999999997335, 52.68983421195638073 ) ) ;
#18356 = PLANE ( 'NONE',  #27866 ) ;
#18358 = ORIENTED_EDGE ( 'NONE', *, *, #21938, .T. ) ;
#18357 = CARTESIAN_POINT ( 'NONE',  ( 26.72610680620850232, -7.491537437428757329, -18.63066883040512067 ) ) ;
#18359 = EDGE_LOOP ( 'NONE', ( #18139, #15204, #24906, #27755 ) ) ;
#18360 = LINE ( 'NONE', #20346, #16361 ) ;
#18361 = CARTESIAN_POINT ( 'NONE',  ( 12.24557421509628519, 9.516296637964343219, -15.33295685416265286 ) ) ;
#18362 = CARTESIAN_POINT ( 'NONE',  ( 33.40713826534622655, -12.56408340279653757, -19.71064172033093698 ) ) ;
#18363 = LINE ( 'NONE', #2211, #8813 ) ;
#18364 = VECTOR ( 'NONE', #25703, 1000.000000000000000 ) ;
#18365 = CARTESIAN_POINT ( 'NONE',  ( 176.1922820468852535, -9.999999999999994671, -2.083034168790677043 ) ) ;
#18366 = EDGE_CURVE ( 'NONE', #25049, #22665, #23647, .T. ) ;
#18367 = CARTESIAN_POINT ( 'NONE',  ( 23.48045015178454165, 1.263488895044508897, -17.26779756161726098 ) ) ;
#18368 = EDGE_LOOP ( 'NONE', ( #274, #16294, #24848, #24470 ) ) ;
#18369 = LINE ( 'NONE', #18678, #2291 ) ;
#18370 = SURFACE_SIDE_STYLE ('',( #24968 ) ) ;
#18371 = CARTESIAN_POINT ( 'NONE',  ( 15.10175627602374249, 9.741420229655037843, -13.89989488922661742 ) ) ;
#18372 = AXIS2_PLACEMENT_3D ( 'NONE', #3219, #15081, #19373 ) ;
#18373 = CARTESIAN_POINT ( 'NONE',  ( 29.25075025305862653, -5.797754334661411768, -14.89650002867986878 ) ) ;
#18374 = AXIS2_PLACEMENT_3D ( 'NONE', #12986, #1406, #10700 ) ;
#18375 = VERTEX_POINT ( 'NONE', #9132 ) ;
#18376 = LINE ( 'NONE', #6793, #13164 ) ;
#18377 = EDGE_CURVE ( 'NONE', #19537, #9002, #2748, .T. ) ;
#18378 = ADVANCED_FACE ( 'NONE', ( #21349, #19059 ), #26096, .F. ) ;
#18379 = EDGE_CURVE ( 'NONE', #2523, #19537, #9433, .T. ) ;
#18380 = CARTESIAN_POINT ( 'NONE',  ( 156.1922820468853672, -10.00000000000000000, -10.74328820663507678 ) ) ;
#18381 = ORIENTED_EDGE ( 'NONE', *, *, #1450, .F. ) ;
#18382 = EDGE_CURVE ( 'NONE', #30249, #3306, #11731, .T. ) ;
#18383 = FACE_OUTER_BOUND ( 'NONE', #7992, .T. ) ;
#18384 = DIRECTION ( 'NONE',  ( -1.110223024625156540E-16, 0.000000000000000000, -1.000000000000000000 ) ) ;
#18385 = DIRECTION ( 'NONE',  ( 0.000000000000000000, 0.000000000000000000, -1.000000000000000000 ) ) ;
#18386 = VECTOR ( 'NONE', #24911, 1000.000000000000000 ) ;
#18387 = DIRECTION ( 'NONE',  ( 0.000000000000000000, -2.775557561562890735E-17, 1.000000000000000000 ) ) ;
#18388 = CARTESIAN_POINT ( 'NONE',  ( 19.07173961884560498, -1.856618079973750390, -13.92706601484911033 ) ) ;
#18389 = CARTESIAN_POINT ( 'NONE',  ( 20.38603433104324480, 7.363110203939331022, -17.91596102798271062 ) ) ;
#18391 = EDGE_LOOP ( 'NONE', ( #29694, #28085, #22182, #1175 ) ) ;
#18390 = CARTESIAN_POINT ( 'NONE',  ( 34.17142927738225922, -16.99764464586957402, -20.98398627866201238 ) ) ;
#18392 = FILL_AREA_STYLE ('',( #20823 ) ) ;
#18393 = VECTOR ( 'NONE', #14077, 1000.000000000000000 ) ;
#18394 = CARTESIAN_POINT ( 'NONE',  ( 11.47372892693763902, 9.265404009280679531, -15.86055721330185619 ) ) ;
#18395 = CARTESIAN_POINT ( 'NONE',  ( 16.00000000000017053, 34.64101615137744972, 10.00000000000000178 ) ) ;
#18396 = PLANE ( 'NONE',  #12447 ) ;
#18397 = CARTESIAN_POINT ( 'NONE',  ( 9.992064777962580635, 14.74057119405591543, -17.75100935390776158 ) ) ;
#18399 = ORIENTED_EDGE ( 'NONE', *, *, #26789, .F. ) ;
#18398 = DIRECTION ( 'NONE',  ( 1.110223024625156540E-16, 2.995891024602366092E-32, 1.000000000000000000 ) ) ;
#18400 = VERTEX_POINT ( 'NONE', #2602 ) ;
#18401 = LINE ( 'NONE', #27753, #2272 ) ;
#18402 = CARTESIAN_POINT ( 'NONE',  ( 12.07641845611955489, 8.540206757827041528, -15.45582622123028216 ) ) ;
#18403 = VECTOR ( 'NONE', #20771, 1000.000000000000000 ) ;
#18404 = ORIENTED_EDGE ( 'NONE', *, *, #24043, .T. ) ;
#18405 = LINE ( 'NONE', #16110, #7606 ) ;
#18406 = CARTESIAN_POINT ( 'NONE',  ( 0.000000000000000000, 2.357898499370430834, -3.469446951953614189E-15 ) ) ;
#18407 = DIRECTION ( 'NONE',  ( 0.000000000000000000, -2.775557561562890735E-17, 1.000000000000000000 ) ) ;
#18408 = ORIENTED_EDGE ( 'NONE', *, *, #12074, .F. ) ;
#18409 = ORIENTED_EDGE ( 'NONE', *, *, #17003, .F. ) ;
#18410 = CARTESIAN_POINT ( 'NONE',  ( 9.112894736278665420, 16.17970140370183785, -17.05457397994698709 ) ) ;
#18411 = CARTESIAN_POINT ( 'NONE',  ( 34.84906220094974572, -20.04189041930405324, -21.18881845514476581 ) ) ;
#18412 = CARTESIAN_POINT ( 'NONE',  ( 15.35879474092683594, 2.467707791974911302, -18.63256289774529151 ) ) ;
#18413 = CARTESIAN_POINT ( 'NONE',  ( 19.04375517570889187, 9.961537237715642590, -16.65452713690489617 ) ) ;
#18414 = VECTOR ( 'NONE', #24572, 1000.000000000000000 ) ;
#18415 = CARTESIAN_POINT ( 'NONE',  ( 154.7287565553230024, -1.999999999999974021, -25.16025403784440329 ) ) ;
#18416 = CARTESIAN_POINT ( 'NONE',  ( 23.96443177966278881, -0.8440764653970969089, -20.02211457469898548 ) ) ;
#18417 = VECTOR ( 'NONE', #12358, 1000.000000000000000 ) ;
#18418 = EDGE_CURVE ( 'NONE', #24045, #17748, #455, .T. ) ;
#18419 = ORIENTED_EDGE ( 'NONE', *, *, #1589, .F. ) ;
#18420 = EDGE_CURVE ( 'NONE', #6258, #19510, #18225, .T. ) ;
#18421 = CARTESIAN_POINT ( 'NONE',  ( 166.1922820468853672, -9.999999999999996447, -30.91696583120936026 ) ) ;
#18422 = EDGE_CURVE ( 'NONE', #319, #30249, #7317, .T. ) ;
#18424 = EDGE_LOOP ( 'NONE', ( #5048, #28668, #12810, #24213 ) ) ;
#18423 = DIRECTION ( 'NONE',  ( -2.698458740408365879E-16, 1.000000000000000000, 0.000000000000000000 ) ) ;
#18425 = ORIENTED_EDGE ( 'NONE', *, *, #23993, .F. ) ;
#18426 = FACE_OUTER_BOUND ( 'NONE', #1656, .T. ) ;
#18427 = FACE_OUTER_BOUND ( 'NONE', #29539, .T. ) ;
#18428 = ORIENTED_EDGE ( 'NONE', *, *, #15753, .F. ) ;
#18429 = CARTESIAN_POINT ( 'NONE',  ( 35.36378496564391583, -20.35426714484339783, -19.25178739305277631 ) ) ;
#18430 = CARTESIAN_POINT ( 'NONE',  ( 10.66893569228806271, 9.043500038842159583, -16.41109624600252559 ) ) ;
#18431 = ORIENTED_EDGE ( 'NONE', *, *, #18377, .F. ) ;
#18432 = VECTOR ( 'NONE', #24003, 1000.000000000000000 ) ;
#18433 = CARTESIAN_POINT ( 'NONE',  ( 34.54859390953723874, -22.18451583373416014, -15.00000000000000000 ) ) ;
#18434 = DIRECTION ( 'NONE',  ( 1.000000000000000000, 2.698458740408365879E-16, -1.110223024625156540E-16 ) ) ;
#18435 = CARTESIAN_POINT ( 'NONE',  ( 11.70392491148546732, 10.80251906652491556, -16.82536866641744311 ) ) ;
#18436 = DIRECTION ( 'NONE',  ( -2.698458740408365879E-16, 1.000000000000000000, 0.000000000000000000 ) ) ;
#18437 = CARTESIAN_POINT ( 'NONE',  ( 72.09850868606311280, -4.999999999999998224, 52.38263276618876318 ) ) ;
#18438 = ORIENTED_EDGE ( 'NONE', *, *, #24524, .F. ) ;
#18439 = CIRCLE ( 'NONE', #21353, 5.000000000000000888 ) ;
#18440 = FACE_OUTER_BOUND ( 'NONE', #1702, .T. ) ;
#18441 = CARTESIAN_POINT ( 'NONE',  ( 87.30281120929834060, -4.999999999999993783, 63.42920515797836600 ) ) ;
#18442 = ORIENTED_EDGE ( 'NONE', *, *, #15818, .T. ) ;
#18443 = ORIENTED_EDGE ( 'NONE', *, *, #2983, .T. ) ;
#18444 = DIRECTION ( 'NONE',  ( 1.000000000000000000, 0.000000000000000000, 0.000000000000000000 ) ) ;
#18445 = VECTOR ( 'NONE', #15440, 1000.000000000000000 ) ;
#18446 = ORIENTED_EDGE ( 'NONE', *, *, #14952, .F. ) ;
#18447 = CARTESIAN_POINT ( 'NONE',  ( 9.667875940510226584, 16.22734252707768832, -17.88507284477129033 ) ) ;
#18448 = EDGE_CURVE ( 'NONE', #6539, #3010, #28265, .T. ) ;
#18449 = CARTESIAN_POINT ( 'NONE',  ( 22.36047763332208405, -4.488847068091893711, -15.41575731358746104 ) ) ;
#18450 = CARTESIAN_POINT ( 'NONE',  ( 20.06573045921589227, -2.681363122285017386, -18.07621394912722934 ) ) ;
#18451 = CARTESIAN_POINT ( 'NONE',  ( 22.61876936045522513, 2.364863857962155258, -15.74433402521326819 ) ) ;
#18452 = LINE ( 'NONE', #5013, #16467 ) ;
#18453 = PLANE ( 'NONE',  #7724 ) ;
#18454 = CARTESIAN_POINT ( 'NONE',  ( 13.00000000000000178, 0.000000000000000000, 9.999999999999998224 ) ) ;
#18455 = CARTESIAN_POINT ( 'NONE',  ( 26.84970692451943819, -5.812874930055231815, -14.04107299160273037 ) ) ;
#18456 = CARTESIAN_POINT ( 'NONE',  ( -20.00000000000017053, 34.64101615137744972, -10.00000000000000000 ) ) ;
#18457 = AXIS2_PLACEMENT_3D ( 'NONE', #19589, #28958, #1447 ) ;
#18458 = CARTESIAN_POINT ( 'NONE',  ( 10.36273093427488590, -5.000000000000015099, 31.89320639659453605 ) ) ;
#18459 = DIRECTION ( 'NONE',  ( 0.000000000000000000, 0.000000000000000000, 1.000000000000000000 ) ) ;
#18460 = VECTOR ( 'NONE', #28263, 1000.000000000000000 ) ;
#18461 = CARTESIAN_POINT ( 'NONE',  ( 10.37265302513970688, 16.90790163500151166, -17.63730412279738147 ) ) ;
#18462 = DIRECTION ( 'NONE',  ( 0.000000000000000000, 0.000000000000000000, 1.000000000000000000 ) ) ;
#18463 = AXIS2_PLACEMENT_3D ( 'NONE', #4431, #20594, #23192 ) ;
#18464 = CARTESIAN_POINT ( 'NONE',  ( 131.1922820468854241, -1.999999999999982236, -13.59645775552055547 ) ) ;
#18465 = ORIENTED_EDGE ( 'NONE', *, *, #15235, .T. ) ;
#18466 = ORIENTED_EDGE ( 'NONE', *, *, #18593, .T. ) ;
#18467 = DIRECTION ( 'NONE',  ( 0.000000000000000000, -2.775557561562890735E-17, 1.000000000000000000 ) ) ;
#18468 = CARTESIAN_POINT ( 'NONE',  ( 15.94478687392618355, 4.193953704849600506, -19.05305658475056063 ) ) ;
#18469 = CARTESIAN_POINT ( 'NONE',  ( 11.27553273857261296, 16.67993683502164615, -16.78480078315762469 ) ) ;
#18470 = DIRECTION ( 'NONE',  ( -0.9116843969807022496, -0.4108911781748707526, 0.000000000000000000 ) ) ;
#18471 = EDGE_LOOP ( 'NONE', ( #24762, #26924 ) ) ;
#18472 = VERTEX_POINT ( 'NONE', #11020 ) ;
#18473 = CARTESIAN_POINT ( 'NONE',  ( 9.641350777746193756, 17.66889129127197577, -17.91630266473768884 ) ) ;
#18474 = CARTESIAN_POINT ( 'NONE',  ( 12.97376706329020557, 7.722038565090276308, -14.75257430067278719 ) ) ;
#18475 = LINE ( 'NONE', #18776, #28351 ) ;
#18476 = DIRECTION ( 'NONE',  ( 0.9510565162951536422, 2.566386769018988816E-16, 0.3090169943749472292 ) ) ;
#18477 = ORIENTED_EDGE ( 'NONE', *, *, #13444, .T. ) ;
#18478 = CARTESIAN_POINT ( 'NONE',  ( -3.673643420401923265, -2.497823135841289677, -0.2484800633750157139 ) ) ;
#18479 = ORIENTED_EDGE ( 'NONE', *, *, #25580, .T. ) ;
#18480 = CARTESIAN_POINT ( 'NONE',  ( 10.63408956504272140, 15.70892033759881734, -17.26778321585235787 ) ) ;
#18481 = EDGE_CURVE ( 'NONE', #27442, #966, #7172, .T. ) ;
#18482 = TOROIDAL_SURFACE ( 'NONE', #26293, 7.000000000000000888, 2.000000000000000000 ) ;
#18483 = CARTESIAN_POINT ( 'NONE',  ( 36.54859390953724585, -21.18451583373416014, -16.11276402859391510 ) ) ;
#18484 = CARTESIAN_POINT ( 'NONE',  ( 24.87127057246125972, -9.548149280147088191, -14.79180087847266556 ) ) ;
#18485 = EDGE_LOOP ( 'NONE', ( #12311, #16938, #11802, #4191 ) ) ;
#18486 = ADVANCED_FACE ( 'NONE', ( #23493 ), #11877, .T. ) ;
#18487 = DIRECTION ( 'NONE',  ( 1.110223024625156540E-16, 2.995891024602366092E-32, 1.000000000000000000 ) ) ;
#18488 = VECTOR ( 'NONE', #15062, 1000.000000000000000 ) ;
#18489 = CARTESIAN_POINT ( 'NONE',  ( 153.6922820468853388, -1.999999999999976241, -0.6060766987539614181 ) ) ;
#18490 = DIRECTION ( 'NONE',  ( 0.000000000000000000, 0.000000000000000000, -1.000000000000000000 ) ) ;
#18491 = CLOSED_SHELL ( 'NONE', ( #3448, #14777, #7502, #4574, #6823, #28735, #3986, #16173 ) ) ;
#18492 = CARTESIAN_POINT ( 'NONE',  ( 16.98323446405135329, 7.186294067752427850, -20.40390978395066313 ) ) ;
#18493 = CARTESIAN_POINT ( 'NONE',  ( 27.14379157474815685, -3.097389544916523185, -14.25532379610351263 ) ) ;
#18494 = ORIENTED_EDGE ( 'NONE', *, *, #20033, .T. ) ;
#18495 = LINE ( 'NONE', #27850, #11804 ) ;
#18496 = DIRECTION ( 'NONE',  ( 0.000000000000000000, -1.000000000000000000, 0.000000000000000000 ) ) ;
#18497 = VECTOR ( 'NONE', #21653, 1000.000000000000000 ) ;
#18498 = CARTESIAN_POINT ( 'NONE',  ( 176.1922820468852819, -1.999999999999969580, -10.74328820663507678 ) ) ;
#18499 = CARTESIAN_POINT ( 'NONE',  ( 6.862631103873988891, -5.000000000000015987, 21.12100677009980032 ) ) ;
#18500 = AXIS2_PLACEMENT_3D ( 'NONE', #9249, #30090, #9100 ) ;
#18501 = CARTESIAN_POINT ( 'NONE',  ( 10.33811696370167077, 18.38618940166710303, -17.91541423781815112 ) ) ;
#18502 = CONICAL_SURFACE ( 'NONE', #7794, 5.999999999999977796, 0.7853981633974509435 ) ;
#18503 = DIRECTION ( 'NONE',  ( -0.9510565162951536422, -2.566386769018988816E-16, -0.3090169943749472292 ) ) ;
#18504 = EDGE_LOOP ( 'NONE', ( #16879, #8944, #4742, #16605 ) ) ;
#18505 = DIRECTION ( 'NONE',  ( 1.000000000000000000, 2.698458740408365879E-16, -1.110223024625156540E-16 ) ) ;
#18506 = ORIENTED_EDGE ( 'NONE', *, *, #28034, .F. ) ;
#18507 = CARTESIAN_POINT ( 'NONE',  ( 11.47219014545126647, 9.272428573238919114, -15.86119603109536058 ) ) ;
#18508 = ORIENTED_EDGE ( 'NONE', *, *, #10653, .F. ) ;
#18509 = CARTESIAN_POINT ( 'NONE',  ( 18.42634509371275797, 7.189141296957872740, -15.94500943014882210 ) ) ;
#18510 = CARTESIAN_POINT ( 'NONE',  ( 4.952801047623463404, -5.000000000000015987, 15.24315424717507206 ) ) ;
#18511 = CARTESIAN_POINT ( 'NONE',  ( 98.27884857356201564, -4.999999999999990230, 71.40376309209180761 ) ) ;
#18513 = ORIENTED_EDGE ( 'NONE', *, *, #15689, .T. ) ;
#18512 = CARTESIAN_POINT ( 'NONE',  ( 27.21278356834291756, -7.014839303453253905, -18.45691071023835761 ) ) ;
#18514 = ORIENTED_EDGE ( 'NONE', *, *, #20669, .T. ) ;
#18515 = LINE ( 'NONE', #11191, #332 ) ;
#18516 = CARTESIAN_POINT ( 'NONE',  ( 11.13911793526871463, 17.30555251181618814, -17.04533519337964975 ) ) ;
#18517 = VERTEX_POINT ( 'NONE', #18912 ) ;
#18518 = EDGE_CURVE ( 'NONE', #25602, #8103, #23115, .T. ) ;
#18519 = CARTESIAN_POINT ( 'NONE',  ( 35.03938282813840743, -19.89690018161999419, -20.20402626681843117 ) ) ;
#18520 = CARTESIAN_POINT ( 'NONE',  ( 175.7287565553229456, -4.999999999999970690, 3.500000000000003109 ) ) ;
#18521 = ADVANCED_FACE ( 'NONE', ( #9740 ), #3617, .T. ) ;
#18522 = DIRECTION ( 'NONE',  ( 0.9510565162951535312, 2.566386769018988816E-16, -0.3090169943749475623 ) ) ;
#18523 = ADVANCED_FACE ( 'NONE', ( #25487 ), #26521, .T. ) ;
#18524 = CARTESIAN_POINT ( 'NONE',  ( 22.08234585817149664, -3.071498426668943793, -18.09723855971599704 ) ) ;
#18525 = ORIENTED_EDGE ( 'NONE', *, *, #19061, .T. ) ;
#18526 = MECHANICAL_DESIGN_GEOMETRIC_PRESENTATION_REPRESENTATION (  '', ( #13160 ), #29292 ) ;
#18527 = LINE ( 'NONE', #6631, #7159 ) ;
#18528 =( LENGTH_UNIT ( ) NAMED_UNIT ( * ) SI_UNIT ( .MILLI., .METRE. ) );
#18529 = VECTOR ( 'NONE', #4482, 1000.000000000000000 ) ;
#18530 = CARTESIAN_POINT ( 'NONE',  ( 22.83681518364245022, 2.349634567491368564, -16.30468554850739338 ) ) ;
#18531 = CARTESIAN_POINT ( 'NONE',  ( 29.08439603799166306, -5.802884797086306001, -14.52222230071497755 ) ) ;
#18532 = ORIENTED_EDGE ( 'NONE', *, *, #17070, .F. ) ;
#18533 = FACE_OUTER_BOUND ( 'NONE', #28421, .T. ) ;
#18534 = CARTESIAN_POINT ( 'NONE',  ( 11.50000000000008171, 17.32050807568872486, -30.00000000000000711 ) ) ;
#18535 = AXIS2_PLACEMENT_3D ( 'NONE', #23583, #2840, #18545 ) ;
#18536 = DIRECTION ( 'NONE',  ( 0.5877852522924731371, 0.000000000000000000, 0.8090169943749474513 ) ) ;
#18537 = AXIS2_PLACEMENT_3D ( 'NONE', #24300, #7960, #25998 ) ;
#18538 = CARTESIAN_POINT ( 'NONE',  ( 1.214306433183764966E-14, 4.618802153517016507, -2.450000000000000178 ) ) ;
#18539 = CARTESIAN_POINT ( 'NONE',  ( 9.641352920869014298, 17.66888146263751125, -17.91030124961049097 ) ) ;
#18540 = CARTESIAN_POINT ( 'NONE',  ( 27.14379157474815685, -3.097389544916523185, -14.25532379610351263 ) ) ;
#18541 = CARTESIAN_POINT ( 'NONE',  ( 19.54218497767158169, 4.227554098413554229, -14.22708607227295730 ) ) ;
#18542 = CARTESIAN_POINT ( 'NONE',  ( 36.54859390953724585, -23.18451583373416014, -17.78191007148576119 ) ) ;
#18544 =( LENGTH_UNIT ( ) NAMED_UNIT ( * ) SI_UNIT ( .MILLI., .METRE. ) );
#18543 = VECTOR ( 'NONE', #6533, 1000.000000000000000 ) ;
#18545 = DIRECTION ( 'NONE',  ( 0.9510565162951536422, 0.000000000000000000, -0.3090169943749475623 ) ) ;
#18546 = LINE ( 'NONE', #20982, #24934 ) ;
#18547 = CARTESIAN_POINT ( 'NONE',  ( 147.2287565553230024, -1.999999999999976685, -12.16987298107780369 ) ) ;
#18549 = ORIENTED_EDGE ( 'NONE', *, *, #19312, .T. ) ;
#18548 = CARTESIAN_POINT ( 'NONE',  ( 15.94478687392618355, 4.193953704849600506, -19.05305658475056063 ) ) ;
#18550 = PLANE ( 'NONE',  #22231 ) ;
#18551 = CARTESIAN_POINT ( 'NONE',  ( 12.60945047077962933, 8.619070305187777947, -15.04294105552940231 ) ) ;
#18552 = VERTEX_POINT ( 'NONE', #7020 ) ;
#18553 = DIRECTION ( 'NONE',  ( 1.000000000000000000, 0.000000000000000000, 0.000000000000000000 ) ) ;
#18554 = FACE_OUTER_BOUND ( 'NONE', #20359, .T. ) ;
#18555 = EDGE_CURVE ( 'NONE', #13963, #10847, #4578, .T. ) ;
#18556 = CARTESIAN_POINT ( 'NONE',  ( 14.79111372287554715, 6.954724682967856175, -19.27298399620107361 ) ) ;
#18557 = EDGE_CURVE ( 'NONE', #28590, #23545, #2, .T. ) ;
#18558 = EDGE_LOOP ( 'NONE', ( #24502, #25017, #3736, #30026 ) ) ;
#18559 = EDGE_CURVE ( 'NONE', #3628, #15830, #28559, .T. ) ;
#18560 = ORIENTED_EDGE ( 'NONE', *, *, #14021, .T. ) ;
#18561 = EDGE_CURVE ( 'NONE', #29468, #15766, #28714, .T. ) ;
#18563 = AXIS2_PLACEMENT_3D ( 'NONE', #18582, #25593, #7444 ) ;
#18562 = CARTESIAN_POINT ( 'NONE',  ( 35.54859390953724585, -23.18451583373416014, -18.06010107863414405 ) ) ;
#18564 = CARTESIAN_POINT ( 'NONE',  ( 23.81787570424677014, -0.6874775570582684070, -15.56398403670522157 ) ) ;
#18565 = VECTOR ( 'NONE', #10789, 1000.000000000000000 ) ;
#18566 = CARTESIAN_POINT ( 'NONE',  ( 18.51435942584036454, 8.743714487506315081, -19.56092670885941587 ) ) ;
#18567 = ORIENTED_EDGE ( 'NONE', *, *, #4401, .F. ) ;
#18568 = CARTESIAN_POINT ( 'NONE',  ( 8.851409776105752414, -5.000000000000015099, 27.24183814871275544 ) ) ;
#18569 = CARTESIAN_POINT ( 'NONE',  ( 25.07021298685211619, 1.093672866225363638, -16.25732641482299812 ) ) ;
#18570 = MECHANICAL_DESIGN_GEOMETRIC_PRESENTATION_REPRESENTATION (  '', ( #1531 ), #18081 ) ;
#18571 = ORIENTED_EDGE ( 'NONE', *, *, #5121, .T. ) ;
#18572 = PLANE ( 'NONE',  #10377 ) ;
#18574 = ORIENTED_EDGE ( 'NONE', *, *, #13349, .F. ) ;
#18573 = CARTESIAN_POINT ( 'NONE',  ( 144.7287565553229740, -10.00000000000000533, 0.8205080756887930260 ) ) ;
#18575 = ORIENTED_EDGE ( 'NONE', *, *, #22136, .F. ) ;
#18576 = CARTESIAN_POINT ( 'NONE',  ( 133.6922820468854241, -1.999999999999981348, -9.266330736598357376 ) ) ;
#18577 = CARTESIAN_POINT ( 'NONE',  ( 13.39606018151479461, 8.691252192278360766, -15.69476314099692971 ) ) ;
#18578 = EDGE_CURVE ( 'NONE', #22249, #20836, #25056, .T. ) ;
#18579 = CARTESIAN_POINT ( 'NONE',  ( 36.21506517127201619, -19.68614788779310132, -19.44682451121369482 ) ) ;
#18580 = AXIS2_PLACEMENT_3D ( 'NONE', #22851, #29474, #11379 ) ;
#18581 = CARTESIAN_POINT ( 'NONE',  ( 10.66768918063838179, 9.049215891674000645, -16.41161178408055932 ) ) ;
#18582 = CARTESIAN_POINT ( 'NONE',  ( 153.6922820468853388, -10.00000000000000178, -15.07341522555727309 ) ) ;
#18583 = DIRECTION ( 'NONE',  ( 1.000000000000000000, 2.698458740408365879E-16, -1.110223024625156540E-16 ) ) ;
#18584 = CARTESIAN_POINT ( 'NONE',  ( 10.47193650065820592, 16.45257496057443802, -17.33483926051624735 ) ) ;
#18585 = CARTESIAN_POINT ( 'NONE',  ( 147.2287565553229740, -1.999999999999977129, -3.509618943233403510 ) ) ;
#18586 = LINE ( 'NONE', #11266, #20732 ) ;
#18587 = VERTEX_POINT ( 'NONE', #3204 ) ;
#18588 = CARTESIAN_POINT ( 'NONE',  ( -4.000000000000003553, -6.938893903907228378E-15, -2.450000000000000178 ) ) ;
#18589 = EDGE_CURVE ( 'NONE', #4293, #12466, #3055, .T. ) ;
#18590 = LINE ( 'NONE', #17346, #2004 ) ;
#18591 = VERTEX_POINT ( 'NONE', #19353 ) ;
#18592 = VERTEX_POINT ( 'NONE', #7613 ) ;
#18593 = EDGE_CURVE ( 'NONE', #29723, #2898, #29165, .T. ) ;
#18594 = CARTESIAN_POINT ( 'NONE',  ( 0.000000000000000000, 0.000000000000000000, 9.480888224575629408 ) ) ;
#18595 = ORIENTED_EDGE ( 'NONE', *, *, #23169, .T. ) ;
#18596 = EDGE_CURVE ( 'NONE', #18615, #18805, #10493, .T. ) ;
#18597 = CARTESIAN_POINT ( 'NONE',  ( 9.661958148507006072, 16.25448227554711167, -17.91102859374088752 ) ) ;
#18598 = CARTESIAN_POINT ( 'NONE',  ( 24.16216977846044145, 1.369666316211566093, -18.31128106405367006 ) ) ;
#18599 = CARTESIAN_POINT ( 'NONE',  ( 20.53830075755067952, -2.223150928429542095, -18.95983797452030828 ) ) ;
#18600 = ORIENTED_EDGE ( 'NONE', *, *, #3571, .F. ) ;
#18601 = CARTESIAN_POINT ( 'NONE',  ( 22.28231863826031756, 1.183864898644814811, -18.90614694914491167 ) ) ;
#18602 = DIRECTION ( 'NONE',  ( -2.698458740408365879E-16, 1.000000000000000000, 0.000000000000000000 ) ) ;
#18603 = CARTESIAN_POINT ( 'NONE',  ( 163.6922820468852819, -9.999999999999998224, 2.247092850131519715 ) ) ;
#18604 = CARTESIAN_POINT ( 'NONE',  ( 10.00000000000007816, 17.32050807568872486, -23.00000000000000711 ) ) ;
#18605 = CARTESIAN_POINT ( 'NONE',  ( 22.34083945069921739, -4.755659482961629436, -14.12236044035638116 ) ) ;
#18606 = EDGE_LOOP ( 'NONE', ( #10004, #12621, #10363 ) ) ;
#18607 = DIRECTION ( 'NONE',  ( -2.698458740408365879E-16, 1.000000000000000000, 0.000000000000000000 ) ) ;
#18608 = LINE ( 'NONE', #26093, #15219 ) ;
#18609 = VECTOR ( 'NONE', #26628, 1000.000000000000000 ) ;
#18610 = DIRECTION ( 'NONE',  ( -0.9510565162951536422, -2.566386769018988323E-16, 0.3090169943749475623 ) ) ;
#18611 = DIRECTION ( 'NONE',  ( 1.110223024625156540E-16, 2.995891024602366092E-32, 1.000000000000000000 ) ) ;
#18612 = EDGE_CURVE ( 'NONE', #6718, #14621, #19677, .T. ) ;
#18613 = CARTESIAN_POINT ( 'NONE',  ( 0.000000000000000000, 0.000000000000000000, 0.000000000000000000 ) ) ;
#18615 = VERTEX_POINT ( 'NONE', #23966 ) ;
#18614 = DIRECTION ( 'NONE',  ( 1.000000000000000000, 0.000000000000000000, 0.000000000000000000 ) ) ;
#18616 = CARTESIAN_POINT ( 'NONE',  ( 33.43446274600908907, -12.68684440242773448, -19.71889742777951327 ) ) ;
#18617 = VERTEX_POINT ( 'NONE', #8054 ) ;
#18618 = CARTESIAN_POINT ( 'NONE',  ( 13.27290874800832121, 7.583804977141803683, -15.79253525446438999 ) ) ;
#18619 = VERTEX_POINT ( 'NONE', #7762 ) ;
#18620 = PLANE ( 'NONE',  #264 ) ;
#18621 = VECTOR ( 'NONE', #16197, 1000.000000000000000 ) ;
#18622 = CARTESIAN_POINT ( 'NONE',  ( 21.04385110482095200, 5.766204710259658306, -15.30406332615466347 ) ) ;
#18623 = CARTESIAN_POINT ( 'NONE',  ( 11.27582353004791216, 16.67860322824865449, -16.78467813988110890 ) ) ;
#18624 = CARTESIAN_POINT ( 'NONE',  ( 34.82539348385352440, -18.93555941106099993, -20.13934242161363741 ) ) ;
#18625 = EDGE_LOOP ( 'NONE', ( #26917, #20680, #8190, #29819 ) ) ;
#18626 = ORIENTED_EDGE ( 'NONE', *, *, #13891, .F. ) ;
#18627 = ORIENTED_EDGE ( 'NONE', *, *, #10098, .T. ) ;
#18628 = CARTESIAN_POINT ( 'NONE',  ( 9.898178882064430084, 16.49104486689975246, -16.51464960819000893 ) ) ;
#18629 = DIRECTION ( 'NONE',  ( -1.000000000000000000, 0.000000000000000000, 0.000000000000000000 ) ) ;
#18630 = CARTESIAN_POINT ( 'NONE',  ( 13.19155076956097083, 7.818281081198240834, -14.57899684263624351 ) ) ;
#18631 = PLANE ( 'NONE',  #28855 ) ;
#18632 = LINE ( 'NONE', #26114, #28675 ) ;
#18633 = VERTEX_POINT ( 'NONE', #604 ) ;
#18634 = ORIENTED_EDGE ( 'NONE', *, *, #14822, .F. ) ;
#18635 = DIRECTION ( 'NONE',  ( 1.000000000000000000, 4.440892098500622217E-16, 0.000000000000000000 ) ) ;
#18636 = ORIENTED_EDGE ( 'NONE', *, *, #8242, .F. ) ;
#18637 = EDGE_CURVE ( 'NONE', #24640, #28929, #12183, .T. ) ;
#18638 = CARTESIAN_POINT ( 'NONE',  ( 10.44197622278032611, 16.58997661396885803, -17.36392598754248695 ) ) ;
#18639 = ORIENTED_EDGE ( 'NONE', *, *, #27218, .T. ) ;
#18640 = CARTESIAN_POINT ( 'NONE',  ( 31.25429145842602452, -9.414624517878500853, -14.20845315089566441 ) ) ;
#18641 = CARTESIAN_POINT ( 'NONE',  ( 26.92971693216691165, -8.617903733377630715, -13.36642543767191427 ) ) ;
#18642 = AXIS2_PLACEMENT_3D ( 'NONE', #18038, #2041, #20628 ) ;
#18643 = PLANE ( 'NONE',  #24265 ) ;
#18644 = VERTEX_POINT ( 'NONE', #28878 ) ;
#18645 = CARTESIAN_POINT ( 'NONE',  ( 4.000000000000000000, 1.557668341133518819, -0.1596965656957546609 ) ) ;
#18646 = CARTESIAN_POINT ( 'NONE',  ( 0.000000000000000000, 0.000000000000000000, 9.999999999999998224 ) ) ;
#18647 = CARTESIAN_POINT ( 'NONE',  ( 18.93384218461971358, 6.651393094135895190, -15.21227712214292538 ) ) ;
#18648 = CARTESIAN_POINT ( 'NONE',  ( 28.13717792526295014, -10.23527491042630011, -17.83415580063453376 ) ) ;
#18649 = AXIS2_PLACEMENT_3D ( 'NONE', #27019, #5776, #29323 ) ;
#18650 = EDGE_LOOP ( 'NONE', ( #18789, #19410, #9378, #16316 ) ) ;
#18651 = CARTESIAN_POINT ( 'NONE',  ( 139.7287565553230024, -4.999999999999979572, 0.8205080756887861426 ) ) ;
#18652 = ORIENTED_EDGE ( 'NONE', *, *, #13817, .F. ) ;
#18653 = ADVANCED_FACE ( 'NONE', ( #26246 ), #742, .F. ) ;
#18654 = DIRECTION ( 'NONE',  ( 1.665334536937734318E-16, -2.498001805406601723E-16, -1.000000000000000000 ) ) ;
#18655 = LINE ( 'NONE', #28000, #28262 ) ;
#18656 = EDGE_CURVE ( 'NONE', #29392, #20051, #26401, .T. ) ;
#18657 = CARTESIAN_POINT ( 'NONE',  ( 146.1922820468854241, -1.999999999999977573, -13.59645775552055902 ) ) ;
#18658 = UNCERTAINTY_MEASURE_WITH_UNIT (LENGTH_MEASURE( 1.000000000000000082E-05 ), #15634, 'distance_accuracy_value', 'NONE');
#18659 = CARTESIAN_POINT ( 'NONE',  ( 10.33811987107833552, 18.38617606806709048, -17.90816805339326834 ) ) ;
#18660 = DIRECTION ( 'NONE',  ( 0.000000000000000000, 0.000000000000000000, 1.000000000000000000 ) ) ;
#18661 = DIRECTION ( 'NONE',  ( 1.000000000000000000, 0.000000000000000000, 0.000000000000000000 ) ) ;
#18662 = ORIENTED_EDGE ( 'NONE', *, *, #9684, .T. ) ;
#18663 = CARTESIAN_POINT ( 'NONE',  ( 10.24089172292967298, 14.91932009296530559, -16.37038124228770997 ) ) ;
#18664 = ORIENTED_EDGE ( 'NONE', *, *, #7535, .T. ) ;
#18665 = CIRCLE ( 'NONE', #21585, 2.928571428571432378 ) ;
#18666 = CARTESIAN_POINT ( 'NONE',  ( 18.17852402710872894, 9.427450501112501158, -16.79750701094832266 ) ) ;
#18667 = LINE ( 'NONE', #11781, #20972 ) ;
#18668 = CARTESIAN_POINT ( 'NONE',  ( 148.6922820468854525, -10.00000000000000178, -26.58683881228715862 ) ) ;
#18669 = CARTESIAN_POINT ( 'NONE',  ( 27.78884322698630882, -6.380937659459246625, -17.89340433249687834 ) ) ;
#18670 = EDGE_LOOP ( 'NONE', ( #7528, #27861, #29527, #3089, #19074 ) ) ;
#18671 = PLANE ( 'NONE',  #16886 ) ;
#18672 = CARTESIAN_POINT ( 'NONE',  ( 11.09873500484433606, 17.49075377836879497, -17.25232203421226274 ) ) ;
#18673 = CARTESIAN_POINT ( 'NONE',  ( 35.53758243340352863, -21.13504710440451007, -18.64505253599016044 ) ) ;
#18674 = CARTESIAN_POINT ( 'NONE',  ( 174.5152310637604671, -1.999999999999968914, -30.37205893520531319 ) ) ;
#18675 = DIRECTION ( 'NONE',  ( -0.000000000000000000, -0.000000000000000000, -1.000000000000000000 ) ) ;
#18676 = CARTESIAN_POINT ( 'NONE',  ( 28.44965076230254653, -4.228683950944192027, -16.16799691904953562 ) ) ;
#18677 = VERTEX_POINT ( 'NONE', #14467 ) ;
#18678 = CARTESIAN_POINT ( 'NONE',  ( 5.907716075748727036, -5.000000000000015987, 18.18208050863744063 ) ) ;
#18679 = FILL_AREA_STYLE_COLOUR ( '', #25904 ) ;
#18680 = CARTESIAN_POINT ( 'NONE',  ( 18.53947781130984751, 1.256531364521723537, -18.82393729036428098 ) ) ;
#18681 = CARTESIAN_POINT ( 'NONE',  ( 17.24934648279766947, 4.534969372434432877, -15.14864769235989073 ) ) ;
#18682 = ORIENTED_EDGE ( 'NONE', *, *, #25376, .T. ) ;
#18683 = CARTESIAN_POINT ( 'NONE',  ( -2.339468227445728132, -3.268109542640681209, -2.449999999999980194 ) ) ;
#18684 = B_SPLINE_CURVE_WITH_KNOTS ( 'NONE', 3,
 ( #25036, #25477, #13860, #10974, #23181, #4122, #16457, #2894 ),
 .UNSPECIFIED., .F., .F.,
 ( 4, 2, 2, 4 ),
 ( 0.004673709593152193878, 0.005837709341827673759, 0.007001709090503152773, 0.009329708587854109933 ),
 .UNSPECIFIED. ) ;
#18685 = VECTOR ( 'NONE', #28798, 1000.000000000000000 ) ;
#18686 = CARTESIAN_POINT ( 'NONE',  ( 75.79387768789761992, -4.999999999999996447, 55.06747550269425773 ) ) ;
#18687 = ORIENTED_EDGE ( 'NONE', *, *, #10697, .T. ) ;
#18688 = EDGE_CURVE ( 'NONE', #2298, #17680, #26550, .T. ) ;
#18689 = EDGE_CURVE ( 'NONE', #21176, #24060, #19805, .T. ) ;
#18690 = CYLINDRICAL_SURFACE ( 'NONE', #24669, 2.749999999999999112 ) ;
#18691 = CARTESIAN_POINT ( 'NONE',  ( -8.000000000000000000, 0.7809653281575998918, 1.234974037096769500E-15 ) ) ;
#18692 = EDGE_CURVE ( 'NONE', #28015, #15364, #3352, .T. ) ;
#18693 = CARTESIAN_POINT ( 'NONE',  ( 136.1922820468854241, -1.999999999999980460, -13.59645775552055547 ) ) ;
#18694 = EDGE_CURVE ( 'NONE', #11084, #8715, #23806, .T. ) ;
#18695 = CARTESIAN_POINT ( 'NONE',  ( 9.641350944112486943, 17.66889052829492002, -17.91441860517739215 ) ) ;
#18696 = CARTESIAN_POINT ( 'NONE',  ( 27.68339325353806046, -3.782361434017075474, -17.87574284786517964 ) ) ;
#18697 = CARTESIAN_POINT ( 'NONE',  ( 22.61876936045522513, 2.364863857962155258, -15.74433402521326819 ) ) ;
#18699 = ORIENTED_EDGE ( 'NONE', *, *, #2615, .F. ) ;
#18698 = CARTESIAN_POINT ( 'NONE',  ( 31.68531546575670532, -10.25520638109567173, -17.65856934995331784 ) ) ;
#18700 = CARTESIAN_POINT ( 'NONE',  ( 16.84948243412402036, 10.49281628697410262, -11.66356073909478575 ) ) ;
#18701 = LINE ( 'NONE', #25727, #10298 ) ;
#18702 = CARTESIAN_POINT ( 'NONE',  ( 151.1922820468853672, -1.999999999999976685, -4.936203717676158398 ) ) ;
#18703 = CARTESIAN_POINT ( 'NONE',  ( 15.73644607668725826, 9.740111719757674535, -14.94734896276200153 ) ) ;
#18704 = VERTEX_POINT ( 'NONE', #14616 ) ;
#18705 = CARTESIAN_POINT ( 'NONE',  ( 127.7287565553229740, -1.999999999999982681, 0.5000000000000115463 ) ) ;
#18706 = CARTESIAN_POINT ( 'NONE',  ( 10.72107673987424015, 16.62988705212242735, -15.95408154060974404 ) ) ;
#18707 = ORIENTED_EDGE ( 'NONE', *, *, #17279, .T. ) ;
#18708 = SHAPE_REPRESENTATION ( 'bushing', ( #13190 ), #6882 ) ;
#18709 = CARTESIAN_POINT ( 'NONE',  ( 130.7287565553229172, -4.999999999999983125, -33.50000000000000000 ) ) ;
#18710 = CARTESIAN_POINT ( 'NONE',  ( 147.0152310637606092, -10.00000000000000178, -32.93883019725009120 ) ) ;
#18711 = CARTESIAN_POINT ( 'NONE',  ( 15.78240017141095741, 4.038647184180326200, -18.77507866864583619 ) ) ;
#18712 = AXIS2_PLACEMENT_3D ( 'NONE', #16312, #18459, #18757 ) ;
#18713 = CARTESIAN_POINT ( 'NONE',  ( 12.89848499713582441, 9.804829593628518580, -14.81257543621576112 ) ) ;
#18714 = EDGE_LOOP ( 'NONE', ( #27782, #20321, #20288, #6303, #21972 ) ) ;
#18715 = CARTESIAN_POINT ( 'NONE',  ( 33.20847722810714231, -12.67161117835268058, -20.69290897523819694 ) ) ;
#18716 = CARTESIAN_POINT ( 'NONE',  ( 25.50636554463319072, -2.203555497659483553, -15.54816553724606187 ) ) ;
#18717 = CARTESIAN_POINT ( 'NONE',  ( 15.96850636225579656, 5.405031054132949819, -14.95518105802344344 ) ) ;
#18718 = CARTESIAN_POINT ( 'NONE',  ( 25.07031029108804887, -10.85539403410516535, -16.40584363908930499 ) ) ;
#18719 = ORIENTED_EDGE ( 'NONE', *, *, #4090, .F. ) ;
#18720 = DIRECTION ( 'NONE',  ( -1.000000000000000000, 0.000000000000000000, 0.000000000000000000 ) ) ;
#18721 = EDGE_CURVE ( 'NONE', #9848, #8637, #9892, .T. ) ;
#18723 = VERTEX_POINT ( 'NONE', #3501 ) ;
#18722 = CARTESIAN_POINT ( 'NONE',  ( 2.500000000000000444, 0.000000000000000000, 2.042000000000002036 ) ) ;
#18724 = VERTEX_POINT ( 'NONE', #10345 ) ;
#18725 = ADVANCED_FACE ( 'NONE', ( #12791 ), #22105, .T. ) ;
#18726 = PLANE ( 'NONE',  #7037 ) ;
#18727 = VECTOR ( 'NONE', #1178, 1000.000000000000000 ) ;
#18728 = EDGE_CURVE ( 'NONE', #17091, #29924, #28002, .T. ) ;
#18729 = CARTESIAN_POINT ( 'NONE',  ( 11.55449181034387962, -5.000000000000014211, 35.56106922512162782 ) ) ;
#18730 = CARTESIAN_POINT ( 'NONE',  ( 36.54859390953724585, -21.18451583373416014, -18.06010107863414405 ) ) ;
#18731 = CARTESIAN_POINT ( 'NONE',  ( 12.78320632028979809, 7.637826363492710158, -14.90445457646871574 ) ) ;
#18732 = ORIENTED_EDGE ( 'NONE', *, *, #21516, .T. ) ;
#18733 = DIRECTION ( 'NONE',  ( 0.9510565162951536422, 2.566386769018988816E-16, 0.3090169943749472292 ) ) ;
#18734 = CARTESIAN_POINT ( 'NONE',  ( 63.44486372867149981, -20.00000000000003197, -15.00000000000000000 ) ) ;
#18735 = AXIS2_PLACEMENT_3D ( 'NONE', #4917, #23390, #9787 ) ;
#18736 = CARTESIAN_POINT ( 'NONE',  ( 10.47195275365909595, 16.45250042224058618, -17.33483252618548676 ) ) ;
#18737 = DIRECTION ( 'NONE',  ( 1.000000000000000000, 0.000000000000000000, 0.000000000000000000 ) ) ;
#18738 = CARTESIAN_POINT ( 'NONE',  ( 20.53864511116330149, -5.000000000000012434, -63.21144993451233063 ) ) ;
#18739 = VERTEX_POINT ( 'NONE', #1669 ) ;
#18740 = DIRECTION ( 'NONE',  ( 1.000000000000000000, 0.000000000000000000, 0.000000000000000000 ) ) ;
#18741 = DIRECTION ( 'NONE',  ( -2.698458740408365879E-16, 1.000000000000000000, 0.000000000000000000 ) ) ;
#18742 = DIRECTION ( 'NONE',  ( -2.698458740408365879E-16, 1.000000000000000000, 0.000000000000000000 ) ) ;
#18743 = ORIENTED_EDGE ( 'NONE', *, *, #6986, .F. ) ;
#18744 = CARTESIAN_POINT ( 'NONE',  ( 9.661887760751893595, 16.25480508276471525, -17.91458275280492884 ) ) ;
#18745 = CARTESIAN_POINT ( 'NONE',  ( 26.88076058338416274, -6.009164776401831887, -18.61148891559023255 ) ) ;
#18746 = EDGE_LOOP ( 'NONE', ( #13988, #17467, #20214, #26715, #8212 ) ) ;
#18747 = CARTESIAN_POINT ( 'NONE',  ( 18.53947781130984751, 1.256531364521723537, -18.82393729036428098 ) ) ;
#18748 = CARTESIAN_POINT ( 'NONE',  ( 146.4575131106458912, -10.00000000000000178, -15.00000000000000000 ) ) ;
#18749 = DIRECTION ( 'NONE',  ( -0.9510565162951536422, -2.566386769018988323E-16, 0.3090169943749475623 ) ) ;
#18750 = AXIS2_PLACEMENT_3D ( 'NONE', #17881, #22639, #10872 ) ;
#18751 = DIRECTION ( 'NONE',  ( 0.9510565162951535312, 2.566386769018988816E-16, -0.3090169943749475623 ) ) ;
#18752 = CARTESIAN_POINT ( 'NONE',  ( 27.21278356834291756, -7.014839303453253905, -18.45691071023835761 ) ) ;
#18753 = LINE ( 'NONE', #23333, #27656 ) ;
#18754 = PLANE ( 'NONE',  #12789 ) ;
#18755 = EDGE_CURVE ( 'NONE', #16563, #19224, #20658, .T. ) ;
#18756 = DIRECTION ( 'NONE',  ( 1.000000000000000000, 4.440892098500622217E-16, 0.000000000000000000 ) ) ;
#18757 = DIRECTION ( 'NONE',  ( 1.000000000000000000, 0.000000000000000000, 0.000000000000000000 ) ) ;
#18758 = EDGE_CURVE ( 'NONE', #8805, #24538, #26045, .T. ) ;
#18759 = EDGE_CURVE ( 'NONE', #12786, #4780, #13832, .T. ) ;
#18760 = CARTESIAN_POINT ( 'NONE',  ( 10.46722255365007115, 16.47419372244215197, -17.33720764016775462 ) ) ;
#18761 = CARTESIAN_POINT ( 'NONE',  ( 35.37764311538968087, -21.41652447078215005, -19.89511094362359955 ) ) ;
#18762 = CARTESIAN_POINT ( 'NONE',  ( 31.15806985163746390, -10.82494328065958911, -14.16671120874331358 ) ) ;
#18763 = ORIENTED_EDGE ( 'NONE', *, *, #17248, .F. ) ;
#18764 = CARTESIAN_POINT ( 'NONE',  ( 8.944592922245861999, 16.95155497634765851, -17.90742740301624991 ) ) ;
#18765 = ORIENTED_EDGE ( 'NONE', *, *, #26020, .F. ) ;
#18766 = LINE ( 'NONE', #4878, #1244 ) ;
#18767 = VECTOR ( 'NONE', #8698, 1000.000000000000000 ) ;
#18768 = CARTESIAN_POINT ( 'NONE',  ( 19.07848178107829540, -2.338951347401693859, -17.85627120065723616 ) ) ;
#18769 = CARTESIAN_POINT ( 'NONE',  ( 11.27146506517978786, 16.69859170370891377, -16.78668372539920739 ) ) ;
#18770 = CARTESIAN_POINT ( 'NONE',  ( 143.6922820468854241, -1.999999999999978462, -15.07341522555727664 ) ) ;
#18771 = ORIENTED_EDGE ( 'NONE', *, *, #13655, .F. ) ;
#18772 = ORIENTED_EDGE ( 'NONE', *, *, #17587, .T. ) ;
#18773 = CARTESIAN_POINT ( 'NONE',  ( 9.641384570184822422, 17.66873631484086715, -17.89388817125738385 ) ) ;
#18774 = LINE ( 'NONE', #170, #28695 ) ;
#18775 = CARTESIAN_POINT ( 'NONE',  ( 10.82443827553465177, 12.24310121783546634, -16.12906421532448675 ) ) ;
#18776 = CARTESIAN_POINT ( 'NONE',  ( 134.5152310637605808, -1.999999999999980460, -19.94844914048349338 ) ) ;
#18777 = CARTESIAN_POINT ( 'NONE',  ( 5.000000000000006217, 2.832769448823991583E-15, -4.974599999999998801 ) ) ;
#18778 = ORIENTED_EDGE ( 'NONE', *, *, #26748, .T. ) ;
#18779 = ORIENTED_EDGE ( 'NONE', *, *, #20074, .T. ) ;
#18780 = LINE ( 'NONE', #14488, #20806 ) ;
#18781 = VERTEX_POINT ( 'NONE', #13542 ) ;
#18782 = CARTESIAN_POINT ( 'NONE',  ( 10.47184394332236224, 16.45299944031493311, -17.33487789703667303 ) ) ;
#18783 = EDGE_LOOP ( 'NONE', ( #25402, #29546, #7100, #18446 ) ) ;
#18784 = CARTESIAN_POINT ( 'NONE',  ( 36.54859390953724585, -22.18451583373416014, -17.22552805718784441 ) ) ;
#18785 = CARTESIAN_POINT ( 'NONE',  ( 26.07968421886551980, -9.001936657367064498, -13.61655714643126913 ) ) ;
#18786 = CARTESIAN_POINT ( 'NONE',  ( 26.47492910780048447, -3.130564378024159211, -15.09640780237150892 ) ) ;
#18787 = ORIENTED_EDGE ( 'NONE', *, *, #12594, .T. ) ;
#18788 = PLANE ( 'NONE',  #9136 ) ;
#18789 = ORIENTED_EDGE ( 'NONE', *, *, #12215, .T. ) ;
#18790 = CARTESIAN_POINT ( 'NONE',  ( 33.24108837279852224, -10.36619216719171632, -17.82210672427467912 ) ) ;
#18791 = CARTESIAN_POINT ( 'NONE',  ( 15.40919527484693319, 5.754234090002595003, -19.70842740302703078 ) ) ;
#18792 = CARTESIAN_POINT ( 'NONE',  ( 27.11308663627701776, -11.54974243744149653, -14.54931088138702933 ) ) ;
#18793 = CIRCLE ( 'NONE', #26635, 8.000000000000005329 ) ;
#18794 = VERTEX_POINT ( 'NONE', #1520 ) ;
#18795 = CARTESIAN_POINT ( 'NONE',  ( 420.0000000000002274, 41.64101615137744972, 10.00000000000000178 ) ) ;
#18796 = ADVANCED_FACE ( 'NONE', ( #24553 ), #13392, .T. ) ;
#18797 = ADVANCED_FACE ( 'NONE', ( #3643 ), #10651, .T. ) ;
#18798 = DIRECTION ( 'NONE',  ( -0.7172983783020616677, 0.6967661275386687336, 0.000000000000000000 ) ) ;
#18799 = LINE ( 'NONE', #11916, #21399 ) ;
#18800 = PLANE ( 'NONE',  #19264 ) ;
#18801 = CIRCLE ( 'NONE', #7111, 7.000000000000006217 ) ;
#18802 = CARTESIAN_POINT ( 'NONE',  ( 10.41323547201801958, 18.04168634714536168, -16.76531574090561350 ) ) ;
#18803 = LINE ( 'NONE', #19106, #20184 ) ;
#18804 = DIRECTION ( 'NONE',  ( 1.000000000000000000, 2.698458740408365879E-16, -1.110223024625156540E-16 ) ) ;
#18805 = VERTEX_POINT ( 'NONE', #27337 ) ;
#18806 = VECTOR ( 'NONE', #2552, 1000.000000000000000 ) ;
#18807 = CARTESIAN_POINT ( 'NONE',  ( 11.40798482813988635, 9.566882342703072695, -15.88774718835883348 ) ) ;
#18808 = VERTEX_POINT ( 'NONE', #17810 ) ;
#18809 = VECTOR ( 'NONE', #3978, 1000.000000000000000 ) ;
#18810 = CARTESIAN_POINT ( 'NONE',  ( 17.24934648279766947, 4.534969372434432877, -15.14864769235989073 ) ) ;
#18811 = CARTESIAN_POINT ( 'NONE',  ( -0.6543461111163901833, -4.241015250120830693, -2.310849780464841352 ) ) ;
#18812 = DIRECTION ( 'NONE',  ( -2.698458740408365879E-16, 1.000000000000000000, 0.000000000000000000 ) ) ;
#18813 = CARTESIAN_POINT ( 'NONE',  ( 25.26806593431409453, -8.821542497490490575, -18.05414547114721557 ) ) ;
#18814 = LINE ( 'NONE', #14523, #7635 ) ;
#18815 = CARTESIAN_POINT ( 'NONE',  ( 11.06231504941914423, 17.65778033641372957, -17.63750823492871334 ) ) ;
#18816 = ORIENTED_EDGE ( 'NONE', *, *, #18561, .T. ) ;
#18817 = CARTESIAN_POINT ( 'NONE',  ( 35.30103323675335503, -20.07235686745416103, -19.24079536022738068 ) ) ;
#18818 = DIRECTION ( 'NONE',  ( 2.908569913943825554E-16, -1.000000000000000000, 0.000000000000000000 ) ) ;
#18819 = CARTESIAN_POINT ( 'NONE',  ( 138.6922820468854525, -10.00000000000000533, -23.73366926340167282 ) ) ;
#18820 = CARTESIAN_POINT ( 'NONE',  ( 24.09482019364002880, -4.431952660107454811, -19.05667854325333721 ) ) ;
#18821 = ORIENTED_EDGE ( 'NONE', *, *, #18201, .F. ) ;
#18822 = CARTESIAN_POINT ( 'NONE',  ( 9.884967449281287344, -8.443187699361503817, -16.50000000000001421 ) ) ;
#18823 = EDGE_CURVE ( 'NONE', #25891, #17512, #4246, .T. ) ;
#18824 =( NAMED_UNIT ( * ) SI_UNIT ( $, .STERADIAN. ) SOLID_ANGLE_UNIT ( ) );
#18825 = CARTESIAN_POINT ( 'NONE',  ( 17.20140313730510684, 4.016069822000726042, -19.84498366692964666 ) ) ;
#18826 = CARTESIAN_POINT ( 'NONE',  ( 17.26923406770577074, 6.766716122889627094, -15.27140832040383422 ) ) ;
#18827 = CIRCLE ( 'NONE', #26139, 4.000000000000000000 ) ;
#18828 = EDGE_LOOP ( 'NONE', ( #21847, #2139, #22647, #12898, #12739 ) ) ;
#18829 = CARTESIAN_POINT ( 'NONE',  ( 159.7287565553229456, -1.999999999999973133, -16.50000000000000355 ) ) ;
#18830 = AXIS2_PLACEMENT_3D ( 'NONE', #13598, #27235, #15431 ) ;
#18831 = AXIS2_PLACEMENT_3D ( 'NONE', #16009, #11424, #14308 ) ;
#18832 = CARTESIAN_POINT ( 'NONE',  ( 163.6922820468852819, -1.999999999999973577, -0.6060766987539614181 ) ) ;
#18833 = CARTESIAN_POINT ( 'NONE',  ( 87.79094120493316211, -4.999999999999993783, -63.78385235900214667 ) ) ;
#18834 = CARTESIAN_POINT ( 'NONE',  ( 133.7287565553229172, -9.999999999999980460, -33.50000000000000000 ) ) ;
#18835 = CARTESIAN_POINT ( 'NONE',  ( 24.00000000000017053, 34.64101615137744972, 14.00000000000000178 ) ) ;
#18836 = ORIENTED_EDGE ( 'NONE', *, *, #24527, .F. ) ;
#18837 = CARTESIAN_POINT ( 'NONE',  ( 9.893572868141015775, 16.51216863388285461, -16.51808063826580408 ) ) ;
#18838 = CARTESIAN_POINT ( 'NONE',  ( 21.64995824428719828, -4.359751022247916552, -19.89060884261010287 ) ) ;
#18839 = CARTESIAN_POINT ( 'NONE',  ( 20.53420570626898822, -0.4664991210283321310, -19.04361528682417415 ) ) ;
#18841 = ORIENTED_EDGE ( 'NONE', *, *, #15130, .F. ) ;
#18840 = CARTESIAN_POINT ( 'NONE',  ( 33.19064478275001306, -12.59149944747283989, -20.68751865480438212 ) ) ;
#18842 = DIRECTION ( 'NONE',  ( -2.698458740408365879E-16, 1.000000000000000000, 0.000000000000000000 ) ) ;
#18843 = DIRECTION ( 'NONE',  ( 0.9773680663943725699, 2.003532158470061275E-17, 0.2115458881484706954 ) ) ;
#18844 = VECTOR ( 'NONE', #10110, 1000.000000000000000 ) ;
#18845 = DIRECTION ( 'NONE',  ( 1.000000000000000000, 0.000000000000000000, 0.000000000000000000 ) ) ;
#18846 = CARTESIAN_POINT ( 'NONE',  ( 2.678494666091048693, 3.072372537026350159, -2.415789719053474283 ) ) ;
#18847 = CARTESIAN_POINT ( 'NONE',  ( 14.29829396236512729, 6.476847147513518088, -18.28004444394726491 ) ) ;
#18848 = ORIENTED_EDGE ( 'NONE', *, *, #9021, .F. ) ;
#18849 = CARTESIAN_POINT ( 'NONE',  ( 132.0152310637605524, -1.999999999999981348, -17.38167787843870826 ) ) ;
#18850 = CARTESIAN_POINT ( 'NONE',  ( 10.72132679622416696, 16.62874026182691267, -15.95397813513572061 ) ) ;
#18851 = EDGE_LOOP ( 'NONE', ( #17983, #10169, #25695, #9992, #265 ) ) ;
#18852 = AXIS2_PLACEMENT_3D ( 'NONE', #25960, #9612, #14186 ) ;
#18853 = LINE ( 'NONE', #2847, #15399 ) ;
#18854 = DIRECTION ( 'NONE',  ( -0.5877852522924731371, -1.586114251531760728E-16, -0.8090169943749474513 ) ) ;
#18855 = VECTOR ( 'NONE', #8402, 1000.000000000000000 ) ;
#18856 = CARTESIAN_POINT ( 'NONE',  ( 19.51440197245297270, 8.071880087464508691, -17.28625796899888201 ) ) ;
#18857 = EDGE_LOOP ( 'NONE', ( #20273, #5550, #30242, #15864 ) ) ;
#18858 = CARTESIAN_POINT ( 'NONE',  ( 27.55585723563325473, -10.26521964199731407, -19.78748283923107820 ) ) ;
#18859 = VERTEX_POINT ( 'NONE', #29333 ) ;
#18860 = CARTESIAN_POINT ( 'NONE',  ( 35.09535884372434111, -21.14837076832613860, -21.10414782775458420 ) ) ;
#18861 = ADVANCED_FACE ( 'NONE', ( #13250 ), #22866, .T. ) ;
#18862 = EDGE_CURVE ( 'NONE', #28921, #11253, #17669, .T. ) ;
#18863 = VECTOR ( 'NONE', #3719, 1000.000000000000000 ) ;
#18864 = CARTESIAN_POINT ( 'NONE',  ( 20.68883037063079300, -1.960602941680898548, -15.52464631352181001 ) ) ;
#18865 = ADVANCED_FACE ( 'NONE', ( #15532 ), #8948, .T. ) ;
#18866 = CARTESIAN_POINT ( 'NONE',  ( 17.00902653454025071, 3.367308883600929281, -16.20218648120260951 ) ) ;
#18867 = CARTESIAN_POINT ( 'NONE',  ( 30.22932097093386261, -9.048247045011217793, -15.48080783641366942 ) ) ;
#18868 = VECTOR ( 'NONE', #12995, 1000.000000000000000 ) ;
#18869 = VERTEX_POINT ( 'NONE', #11254 ) ;
#18870 = DIRECTION ( 'NONE',  ( -2.698458740408365879E-16, 1.000000000000000000, 0.000000000000000000 ) ) ;
#18871 = CARTESIAN_POINT ( 'NONE',  ( 20.00000000000017053, 34.64101615137744972, 12.00000000000000178 ) ) ;
#18872 = AXIS2_PLACEMENT_3D ( 'NONE', #21258, #2524, #24023 ) ;
#18873 = DIRECTION ( 'NONE',  ( -2.698458740408365879E-16, 1.000000000000000000, 0.000000000000000000 ) ) ;
#18874 = FACE_OUTER_BOUND ( 'NONE', #11373, .T. ) ;
#18875 = CARTESIAN_POINT ( 'NONE',  ( 36.31991209326969283, -20.15716956937155047, -19.46864736847591359 ) ) ;
#18876 =( BOUNDED_SURFACE ( )  B_SPLINE_SURFACE ( 3, 3, ( 
 ( #20058, #24344, #29114, #1306, #17312, #3442, #29432, #22513, #10595, #12733, #14862, #1157, #26968, #6028, #24644, #3739, #10751, #1613, #8453, #5579, #24201, #3304, #10291, #28969, #21898, #9194, #13779, #4633, #1758, #18362, #6330, #8746, #27720, #6481, #13479, #22961, #11343, #11484, #27426, #13334, #15918, #22657, #30032, #20798, #15770, #30184, #27569, #4488, #18519, #25540, #11047, #20349, #6625, #4335, #25095, #25248, #27877, #6932, #6780, #18213, #11640, #16226, #13631, #29740, #18065, #16070, #2062, #20645, #4185, #9040, #22811, #1915, #9347, #25398, #13923, #11193, #23107, #23255 ),
 ( #20503, #29889, #2210, #2368, #20951, #8897, #63, #27280, #15625, #24959, #4039, #7233, #21564, #18973, #26159, #9948, #16982, #4785, #11790, #28332, #26005, #16532, #16682, #12246, #663, #28475, #9654, #3120, #19261, #7387, #21109, #2521, #19119, #5084, #2812, #215, #14372, #14075, #23404, #809, #23710, #26308, #25855, #12096, #7674, #24020, #21412, #517, #25693, #18817, #5390, #4934, #5233, #9807, #9493, #14225, #12392, #28175, #21704, #7523, #14677, #18673, #28018, #16827, #28619, #14527, #23557, #7077, #16374, #2658, #23869, #11934, #2969, #21256, #367, #5987, #10251, #15127 ),
 ( #19564, #10101, #17720, #969, #10554, #24457, #1124, #19863, #26771, #5693, #24764, #8263, #3853, #3553, #24607, #28932, #14972, #24308, #12540, #21859, #3699, #27079, #3404, #7968, #19414, #26612, #12695, #12845, #17276, #22157, #1267, #29389, #29227, #17573, #22016, #10402, #5540, #14825, #19709, #22312, #26928, #6138, #24160, #15275, #29075, #17422, #8117, #5841, #13000, #1421, #10710, #20020, #13150, #8415, #15434, #22474, #3265, #28783, #7826, #17133, #26460, #8861, #27239, #6289, #13889, #18179, #9154, #29698, #1880, #20759, #6902, #29855, #6591, #8563, #1720, #18483, #8712, #9005 ),
 ( #16192, #11005, #18027, #13446, #2030, #22929, #15735, #15881, #15585, #27839, #17863, #6743, #20309, #27393, #27537, #18325, #1572, #4455, #6446, #25062, #23075, #2174, #11450, #10851, #4149, #30147, #25360, #25214, #13601, #13747, #22774, #25510, #4601, #24920, #20162, #11161, #29544, #22619, #20466, #4302, #11309, #16035, #4001, #27683, #20612, #30000, #13300, #23367, #27986, #5199, #181, #25815, #28292, #19085, #23518, #23672, #20914, #2627, #9768, #12208, #25655, #7346, #4747, #14493, #7046, #21527, #9315, #16337, #18936, #23830, #9460, #28437, #28, #18784, #2776, #16646, #629, #14038 ),
 ( #18640, #25964, #7489, #11757, #26121, #11902, #479, #2928, #9914, #2483, #21074, #28138, #21218, #333, #7195, #9618, #16794, #19225, #12058, #14191, #7636, #28582, #5045, #16489, #4896, #21371, #14336, #16943, #26272, #5354, #23216, #2331, #11600, #22401, #22701, #12502, #15355, #4084, #20391, #13078, #20101, #21666, #14786, #1808, #21825, #22557, #6220, #17096, #10217, #29782, #10065, #8790, #17798, #11090, #18107, #27469, #15513, #25001, #24694, #5501, #23987, #3084, #12353, #20244, #14640, #29631, #24847, #768, #10933, #24126, #29479, #3781, #19377, #6069, #3224, #28741, #7787, #925 ),
 ( #13377, #26421, #19948, #17651, #29315, #8349, #1504, #10794, #27013, #8643, #15668, #17946, #3933, #8499, #6377, #27160, #13236, #27321, #1655, #9086, #11527, #2406, #6828, #6974, #4229, #16116, #23294, #25740, #8939, #20839, #18255, #18715, #11239, #4822, #22855, #20543, #2254, #28063, #13679, #11682, #13530, #23005, #16261, #30220, #14120, #29932, #23449, #1957, #6523, #18411, #25437, #107, #27610, #9389, #20996, #7116, #18860, #16420, #25573, #15813, #2561, #4672, #6673, #11835, #27761, #15962, #25292, #21147, #9232, #18562, #4528, #25138, #27915, #13964, #13816, #258, #9536, #4381 ),
 ( #2107, #11384, #23144, #20688, #30074, #407, #12288, #564, #19458, #5280, #2853, #21300, #14567, #25898, #9692, #17027, #16575, #12139, #3310, #7427, #14416, #9849, #28669, #19307, #21456, #21608, #11980, #5586, #4975, #3162, #16727, #26048, #23917, #5432, #10297, #856, #5126, #19162, #28828, #7865, #17175, #7272, #23756, #26504, #21753, #3011, #9991, #10146, #28519, #12586, #14867, #14266, #21905, #7567, #24207, #19018, #16873, #706, #26202, #12434, #1020, #24062, #7718, #26353, #28222, #28372, #2697, #23601, #14719, #22201, #24651, #15478, #19912, #20064, #17319, #29276, #6183, #8607 ) ),
 .UNSPECIFIED., .T., .F., .F. ) 
 B_SPLINE_SURFACE_WITH_KNOTS ( ( 4, 3, 4 ),
 ( 4, 2, 2, 2, 2, 2, 2, 2, 2, 2, 2, 2, 2, 2, 2, 2, 2, 2, 2, 2, 2, 2, 2, 2, 2, 2, 2, 2, 2, 2, 2, 2, 2, 2, 2, 2, 2, 2, 4 ),
 ( 0.000000000000000000, 0.5000000000000000000, 1.000000000000000000 ),
 ( 0.000000000000000000, 0.1003381136405422785, 0.1505071704608134109, 0.1755916988709489979, 0.1881339630760167636, 0.1944050951785506465, 0.2006762272810845571, 0.2086934065084689038, 0.2167105857358532783, 0.2327449441906219718, 0.2648136611001593588, 0.2968823780096967457, 0.3129167364644654947, 0.3209339156918498137, 0.3289510949192341882, 0.3346579968240730452, 0.3403648987289118466, 0.3517787025385894495, 0.3746063101579446553, 0.4202615253966550668, 0.5115719558740758899, 0.6028823863514967130, 0.6485376015902071245, 0.6713652092095623303, 0.6827790130192399332, 0.6941928168289175360, 0.7036545619149295883, 0.7131163070009416405, 0.7320397971729657449, 0.7698867775170139538, 0.8077337578610621627, 0.8266572480330862671, 0.8361189931190984304, 0.8455807382051104826, 0.8552319420672911399, 0.8648831459294716861, 0.8841855536538327787, 0.9227903691025551858, 1.000000000000000000 ),
 .UNSPECIFIED. ) 
 GEOMETRIC_REPRESENTATION_ITEM ( )  RATIONAL_B_SPLINE_SURFACE ( (
 ( 1.000000000000000000, 1.000000000000000000, 1.000000000000000000, 1.000000000000000000, 1.000000000000000000, 1.000000000000000000, 1.000000000000000000, 1.000000000000000000, 1.000000000000000000, 1.000000000000000000, 1.000000000000000000, 1.000000000000000000, 1.000000000000000000, 1.000000000000000000, 1.000000000000000000, 1.000000000000000000, 1.000000000000000000, 1.000000000000000000, 1.000000000000000000, 1.000000000000000000, 1.000000000000000000, 1.000000000000000000, 1.000000000000000000, 1.000000000000000000, 1.000000000000000000, 1.000000000000000000, 1.000000000000000000, 1.000000000000000000, 1.000000000000000000, 1.000000000000000000, 1.000000000000000000, 1.000000000000000000, 1.000000000000000000, 1.000000000000000000, 1.000000000000000000, 1.000000000000000000, 1.000000000000000000, 1.000000000000000000, 1.000000000000000000, 1.000000000000000000, 1.000000000000000000, 1.000000000000000000, 1.000000000000000000, 1.000000000000000000, 1.000000000000000000, 1.000000000000000000, 1.000000000000000000, 1.000000000000000000, 1.000000000000000000, 1.000000000000000000, 1.000000000000000000, 1.000000000000000000, 1.000000000000000000, 1.000000000000000000, 1.000000000000000000, 1.000000000000000000, 1.000000000000000000, 1.000000000000000000, 1.000000000000000000, 1.000000000000000000, 1.000000000000000000, 1.000000000000000000, 1.000000000000000000, 1.000000000000000000, 1.000000000000000000, 1.000000000000000000, 1.000000000000000000, 1.000000000000000000, 1.000000000000000000, 1.000000000000000000, 1.000000000000000000, 1.000000000000000000, 1.000000000000000000, 1.000000000000000000, 1.000000000000000000, 1.000000000000000000, 1.000000000000000000, 1.000000000000000000),
 ( 0.3333333333333333703, 0.3333333333333333703, 0.3333333333333333703, 0.3333333333333333703, 0.3333333333333333703, 0.3333333333333333703, 0.3333333333333333703, 0.3333333333333333703, 0.3333333333333333703, 0.3333333333333333703, 0.3333333333333333703, 0.3333333333333333703, 0.3333333333333333703, 0.3333333333333333703, 0.3333333333333333703, 0.3333333333333333703, 0.3333333333333333703, 0.3333333333333333703, 0.3333333333333333703, 0.3333333333333333703, 0.3333333333333333703, 0.3333333333333333703, 0.3333333333333333703, 0.3333333333333333703, 0.3333333333333333703, 0.3333333333333333703, 0.3333333333333333703, 0.3333333333333333703, 0.3333333333333333703, 0.3333333333333333703, 0.3333333333333333703, 0.3333333333333333703, 0.3333333333333333703, 0.3333333333333333703, 0.3333333333333333703, 0.3333333333333333703, 0.3333333333333333703, 0.3333333333333333703, 0.3333333333333333703, 0.3333333333333333703, 0.3333333333333333703, 0.3333333333333333703, 0.3333333333333333703, 0.3333333333333333703, 0.3333333333333333703, 0.3333333333333333703, 0.3333333333333333703, 0.3333333333333333703, 0.3333333333333333703, 0.3333333333333333703, 0.3333333333333333703, 0.3333333333333333703, 0.3333333333333333703, 0.3333333333333333703, 0.3333333333333333703, 0.3333333333333333703, 0.3333333333333333703, 0.3333333333333333703, 0.3333333333333333703, 0.3333333333333333703, 0.3333333333333333703, 0.3333333333333333703, 0.3333333333333333703, 0.3333333333333333703, 0.3333333333333333703, 0.3333333333333333703, 0.3333333333333333703, 0.3333333333333333703, 0.3333333333333333703, 0.3333333333333333703, 0.3333333333333333703, 0.3333333333333333703, 0.3333333333333333703, 0.3333333333333333703, 0.3333333333333333703, 0.3333333333333333703, 0.3333333333333333703, 0.3333333333333333703),
 ( 0.3333333333333333703, 0.3333333333333333703, 0.3333333333333333703, 0.3333333333333333703, 0.3333333333333333703, 0.3333333333333333703, 0.3333333333333333703, 0.3333333333333333703, 0.3333333333333333703, 0.3333333333333333703, 0.3333333333333333703, 0.3333333333333333703, 0.3333333333333333703, 0.3333333333333333703, 0.3333333333333333703, 0.3333333333333333703, 0.3333333333333333703, 0.3333333333333333703, 0.3333333333333333703, 0.3333333333333333703, 0.3333333333333333703, 0.3333333333333333703, 0.3333333333333333703, 0.3333333333333333703, 0.3333333333333333703, 0.3333333333333333703, 0.3333333333333333703, 0.3333333333333333703, 0.3333333333333333703, 0.3333333333333333703, 0.3333333333333333703, 0.3333333333333333703, 0.3333333333333333703, 0.3333333333333333703, 0.3333333333333333703, 0.3333333333333333703, 0.3333333333333333703, 0.3333333333333333703, 0.3333333333333333703, 0.3333333333333333703, 0.3333333333333333703, 0.3333333333333333703, 0.3333333333333333703, 0.3333333333333333703, 0.3333333333333333703, 0.3333333333333333703, 0.3333333333333333703, 0.3333333333333333703, 0.3333333333333333703, 0.3333333333333333703, 0.3333333333333333703, 0.3333333333333333703, 0.3333333333333333703, 0.3333333333333333703, 0.3333333333333333703, 0.3333333333333333703, 0.3333333333333333703, 0.3333333333333333703, 0.3333333333333333703, 0.3333333333333333703, 0.3333333333333333703, 0.3333333333333333703, 0.3333333333333333703, 0.3333333333333333703, 0.3333333333333333703, 0.3333333333333333703, 0.3333333333333333703, 0.3333333333333333703, 0.3333333333333333703, 0.3333333333333333703, 0.3333333333333333703, 0.3333333333333333703, 0.3333333333333333703, 0.3333333333333333703, 0.3333333333333333703, 0.3333333333333333703, 0.3333333333333333703, 0.3333333333333333703),
 ( 1.000000000000000000, 1.000000000000000000, 1.000000000000000000, 1.000000000000000000, 1.000000000000000000, 1.000000000000000000, 1.000000000000000000, 1.000000000000000000, 1.000000000000000000, 1.000000000000000000, 1.000000000000000000, 1.000000000000000000, 1.000000000000000000, 1.000000000000000000, 1.000000000000000000, 1.000000000000000000, 1.000000000000000000, 1.000000000000000000, 1.000000000000000000, 1.000000000000000000, 1.000000000000000000, 1.000000000000000000, 1.000000000000000000, 1.000000000000000000, 1.000000000000000000, 1.000000000000000000, 1.000000000000000000, 1.000000000000000000, 1.000000000000000000, 1.000000000000000000, 1.000000000000000000, 1.000000000000000000, 1.000000000000000000, 1.000000000000000000, 1.000000000000000000, 1.000000000000000000, 1.000000000000000000, 1.000000000000000000, 1.000000000000000000, 1.000000000000000000, 1.000000000000000000, 1.000000000000000000, 1.000000000000000000, 1.000000000000000000, 1.000000000000000000, 1.000000000000000000, 1.000000000000000000, 1.000000000000000000, 1.000000000000000000, 1.000000000000000000, 1.000000000000000000, 1.000000000000000000, 1.000000000000000000, 1.000000000000000000, 1.000000000000000000, 1.000000000000000000, 1.000000000000000000, 1.000000000000000000, 1.000000000000000000, 1.000000000000000000, 1.000000000000000000, 1.000000000000000000, 1.000000000000000000, 1.000000000000000000, 1.000000000000000000, 1.000000000000000000, 1.000000000000000000, 1.000000000000000000, 1.000000000000000000, 1.000000000000000000, 1.000000000000000000, 1.000000000000000000, 1.000000000000000000, 1.000000000000000000, 1.000000000000000000, 1.000000000000000000, 1.000000000000000000, 1.000000000000000000),
 ( 0.3333333333333333703, 0.3333333333333333703, 0.3333333333333333703, 0.3333333333333333703, 0.3333333333333333703, 0.3333333333333333703, 0.3333333333333333703, 0.3333333333333333703, 0.3333333333333333703, 0.3333333333333333703, 0.3333333333333333703, 0.3333333333333333703, 0.3333333333333333703, 0.3333333333333333703, 0.3333333333333333703, 0.3333333333333333703, 0.3333333333333333703, 0.3333333333333333703, 0.3333333333333333703, 0.3333333333333333703, 0.3333333333333333703, 0.3333333333333333703, 0.3333333333333333703, 0.3333333333333333703, 0.3333333333333333703, 0.3333333333333333703, 0.3333333333333333703, 0.3333333333333333703, 0.3333333333333333703, 0.3333333333333333703, 0.3333333333333333703, 0.3333333333333333703, 0.3333333333333333703, 0.3333333333333333703, 0.3333333333333333703, 0.3333333333333333703, 0.3333333333333333703, 0.3333333333333333703, 0.3333333333333333703, 0.3333333333333333703, 0.3333333333333333703, 0.3333333333333333703, 0.3333333333333333703, 0.3333333333333333703, 0.3333333333333333703, 0.3333333333333333703, 0.3333333333333333703, 0.3333333333333333703, 0.3333333333333333703, 0.3333333333333333703, 0.3333333333333333703, 0.3333333333333333703, 0.3333333333333333703, 0.3333333333333333703, 0.3333333333333333703, 0.3333333333333333703, 0.3333333333333333703, 0.3333333333333333703, 0.3333333333333333703, 0.3333333333333333703, 0.3333333333333333703, 0.3333333333333333703, 0.3333333333333333703, 0.3333333333333333703, 0.3333333333333333703, 0.3333333333333333703, 0.3333333333333333703, 0.3333333333333333703, 0.3333333333333333703, 0.3333333333333333703, 0.3333333333333333703, 0.3333333333333333703, 0.3333333333333333703, 0.3333333333333333703, 0.3333333333333333703, 0.3333333333333333703, 0.3333333333333333703, 0.3333333333333333703),
 ( 0.3333333333333333703, 0.3333333333333333703, 0.3333333333333333703, 0.3333333333333333703, 0.3333333333333333703, 0.3333333333333333703, 0.3333333333333333703, 0.3333333333333333703, 0.3333333333333333703, 0.3333333333333333703, 0.3333333333333333703, 0.3333333333333333703, 0.3333333333333333703, 0.3333333333333333703, 0.3333333333333333703, 0.3333333333333333703, 0.3333333333333333703, 0.3333333333333333703, 0.3333333333333333703, 0.3333333333333333703, 0.3333333333333333703, 0.3333333333333333703, 0.3333333333333333703, 0.3333333333333333703, 0.3333333333333333703, 0.3333333333333333703, 0.3333333333333333703, 0.3333333333333333703, 0.3333333333333333703, 0.3333333333333333703, 0.3333333333333333703, 0.3333333333333333703, 0.3333333333333333703, 0.3333333333333333703, 0.3333333333333333703, 0.3333333333333333703, 0.3333333333333333703, 0.3333333333333333703, 0.3333333333333333703, 0.3333333333333333703, 0.3333333333333333703, 0.3333333333333333703, 0.3333333333333333703, 0.3333333333333333703, 0.3333333333333333703, 0.3333333333333333703, 0.3333333333333333703, 0.3333333333333333703, 0.3333333333333333703, 0.3333333333333333703, 0.3333333333333333703, 0.3333333333333333703, 0.3333333333333333703, 0.3333333333333333703, 0.3333333333333333703, 0.3333333333333333703, 0.3333333333333333703, 0.3333333333333333703, 0.3333333333333333703, 0.3333333333333333703, 0.3333333333333333703, 0.3333333333333333703, 0.3333333333333333703, 0.3333333333333333703, 0.3333333333333333703, 0.3333333333333333703, 0.3333333333333333703, 0.3333333333333333703, 0.3333333333333333703, 0.3333333333333333703, 0.3333333333333333703, 0.3333333333333333703, 0.3333333333333333703, 0.3333333333333333703, 0.3333333333333333703, 0.3333333333333333703, 0.3333333333333333703, 0.3333333333333333703),
 ( 1.000000000000000000, 1.000000000000000000, 1.000000000000000000, 1.000000000000000000, 1.000000000000000000, 1.000000000000000000, 1.000000000000000000, 1.000000000000000000, 1.000000000000000000, 1.000000000000000000, 1.000000000000000000, 1.000000000000000000, 1.000000000000000000, 1.000000000000000000, 1.000000000000000000, 1.000000000000000000, 1.000000000000000000, 1.000000000000000000, 1.000000000000000000, 1.000000000000000000, 1.000000000000000000, 1.000000000000000000, 1.000000000000000000, 1.000000000000000000, 1.000000000000000000, 1.000000000000000000, 1.000000000000000000, 1.000000000000000000, 1.000000000000000000, 1.000000000000000000, 1.000000000000000000, 1.000000000000000000, 1.000000000000000000, 1.000000000000000000, 1.000000000000000000, 1.000000000000000000, 1.000000000000000000, 1.000000000000000000, 1.000000000000000000, 1.000000000000000000, 1.000000000000000000, 1.000000000000000000, 1.000000000000000000, 1.000000000000000000, 1.000000000000000000, 1.000000000000000000, 1.000000000000000000, 1.000000000000000000, 1.000000000000000000, 1.000000000000000000, 1.000000000000000000, 1.000000000000000000, 1.000000000000000000, 1.000000000000000000, 1.000000000000000000, 1.000000000000000000, 1.000000000000000000, 1.000000000000000000, 1.000000000000000000, 1.000000000000000000, 1.000000000000000000, 1.000000000000000000, 1.000000000000000000, 1.000000000000000000, 1.000000000000000000, 1.000000000000000000, 1.000000000000000000, 1.000000000000000000, 1.000000000000000000, 1.000000000000000000, 1.000000000000000000, 1.000000000000000000, 1.000000000000000000, 1.000000000000000000, 1.000000000000000000, 1.000000000000000000, 1.000000000000000000, 1.000000000000000000) ) ) 
 REPRESENTATION_ITEM ( '' )  SURFACE ( )  );
#18877 = CARTESIAN_POINT ( 'NONE',  ( 9.641350810849047548, 17.66889113945805789, -17.91796598306941135 ) ) ;
#18878 = ORIENTED_EDGE ( 'NONE', *, *, #26856, .T. ) ;
#18879 = DIRECTION ( 'NONE',  ( 0.000000000000000000, 1.471414886128461471E-15, 1.000000000000000000 ) ) ;
#18880 = DIRECTION ( 'NONE',  ( -2.698458740408365879E-16, 1.000000000000000000, 0.000000000000000000 ) ) ;
#18881 = CARTESIAN_POINT ( 'NONE',  ( 12.56022695423237145, 8.580358410770909217, -16.34122335808152826 ) ) ;
#18882 = CARTESIAN_POINT ( 'NONE',  ( -1.310841663519413114, 7.511012776518212944E-16, -5.000000000000000888 ) ) ;
#18883 = LINE ( 'NONE', #585, #12945 ) ;
#18884 = EDGE_CURVE ( 'NONE', #17616, #600, #3799, .T. ) ;
#18885 = VERTEX_POINT ( 'NONE', #5937 ) ;
#18886 = ORIENTED_EDGE ( 'NONE', *, *, #29573, .F. ) ;
#18887 = DIRECTION ( 'NONE',  ( 0.9510565162951536422, 2.566386769018988816E-16, 0.3090169943749472292 ) ) ;
#18888 = VECTOR ( 'NONE', #7629, 1000.000000000000000 ) ;
#18889 = CYLINDRICAL_SURFACE ( 'NONE', #23423, 1.499999999999996225 ) ;
#18890 = VERTEX_POINT ( 'NONE', #1823 ) ;
#18891 = DIRECTION ( 'NONE',  ( 6.938893903907227392E-16, -0.000000000000000000, 1.000000000000000000 ) ) ;
#18892 = ORIENTED_EDGE ( 'NONE', *, *, #2645, .F. ) ;
#18893 = CARTESIAN_POINT ( 'NONE',  ( 9.669138625804738041, 16.22155169136211583, -17.88455067742322413 ) ) ;
#18894 = EDGE_CURVE ( 'NONE', #30251, #10208, #1363, .T. ) ;
#18895 = VECTOR ( 'NONE', #337, 1000.000000000000000 ) ;
#18896 = CARTESIAN_POINT ( 'NONE',  ( 23.13192804015912785, -6.366449129859712563, -15.65771855518050870 ) ) ;
#18897 = EDGE_CURVE ( 'NONE', #3561, #17674, #20406, .T. ) ;
#18898 = ADVANCED_FACE ( 'NONE', ( #27180 ), #15680, .T. ) ;
#18899 = CARTESIAN_POINT ( 'NONE',  ( 26.68443370873975340, -2.140902173977853540, -15.79004130932784555 ) ) ;
#18900 = DIRECTION ( 'NONE',  ( -1.000000000000000000, -1.280948979423041851E-16, -0.000000000000000000 ) ) ;
#18901 = DIRECTION ( 'NONE',  ( -2.698458740408365879E-16, 1.000000000000000000, 0.000000000000000000 ) ) ;
#18902 = EDGE_CURVE ( 'NONE', #11106, #6687, #8808, .T. ) ;
#18903 = CARTESIAN_POINT ( 'NONE',  ( 174.5152310637604387, -4.999999999999970690, -11.28819510263909542 ) ) ;
#18904 = CONICAL_SURFACE ( 'NONE', #14026, 8.000000000000007105, 1.047197551196596077 ) ;
#18905 = CARTESIAN_POINT ( 'NONE',  ( 28.12266609392075267, -5.599633216697744942, -16.00068813756295327 ) ) ;
#18906 = ORIENTED_EDGE ( 'NONE', *, *, #11426, .T. ) ;
#18907 = CARTESIAN_POINT ( 'NONE',  ( 157.0152310637605808, -9.999999999999998224, -32.93883019725009120 ) ) ;
#18908 = LINE ( 'NONE', #23644, #4993 ) ;
#18909 = CARTESIAN_POINT ( 'NONE',  ( 101.3039376645797347, -4.999999999999989342, -73.60161896772125090 ) ) ;
#18910 = CONICAL_SURFACE ( 'NONE', #7223, 5.000000000000000888, 0.7853981633974456145 ) ;
#18911 = DIRECTION ( 'NONE',  ( -0.9510565162951536422, 0.000000000000000000, -0.3090169943749472292 ) ) ;
#18912 = CARTESIAN_POINT ( 'NONE',  ( 132.0152310637605808, -4.999999999999982236, -15.61832212156129351 ) ) ;
#18913 = CARTESIAN_POINT ( 'NONE',  ( 10.47204342302745417, 16.45208460095963687, -17.33479495221483901 ) ) ;
#18914 = DIRECTION ( 'NONE',  ( 0.000000000000000000, 0.000000000000000000, 1.000000000000000000 ) ) ;
#18915 = CARTESIAN_POINT ( 'NONE',  ( 130.7287565553229172, -4.999999999999982236, -2.233642730705378998 ) ) ;
#18916 = VECTOR ( 'NONE', #8534, 1000.000000000000000 ) ;
#18917 = ORIENTED_EDGE ( 'NONE', *, *, #26706, .F. ) ;
#18918 = CARTESIAN_POINT ( 'NONE',  ( 13.38350887602579142, 7.627675785621035764, -15.70476675302002612 ) ) ;
#18919 = ORIENTED_EDGE ( 'NONE', *, *, #13945, .F. ) ;
#18920 = FACE_OUTER_BOUND ( 'NONE', #10630, .T. ) ;
#18921 = CARTESIAN_POINT ( 'NONE',  ( 22.89472691350227507, 1.279074496056108901, -19.72372301458170796 ) ) ;
#18922 = CARTESIAN_POINT ( 'NONE',  ( 11.27712745377669101, 16.67262326781682802, -16.78413812462462573 ) ) ;
#18923 = CARTESIAN_POINT ( 'NONE',  ( 10.99808568030000444, -5.000000000000015099, 33.84862723870220691 ) ) ;
#18924 = ORIENTED_EDGE ( 'NONE', *, *, #5370, .T. ) ;
#18925 = ORIENTED_EDGE ( 'NONE', *, *, #28285, .T. ) ;
#18926 = CARTESIAN_POINT ( 'NONE',  ( 9.641350810849047548, 17.66889113945805789, -17.92981046679734547 ) ) ;
#18927 = CARTESIAN_POINT ( 'NONE',  ( 153.6922820468853388, -10.00000000000000178, -17.92658477444275533 ) ) ;
#18928 = CARTESIAN_POINT ( 'NONE',  ( 9.917015787971365626, 16.40465641526357743, -16.50431533440121257 ) ) ;
#18929 = DIRECTION ( 'NONE',  ( 1.000000000000000000, 2.698458740408365879E-16, -1.110223024625156540E-16 ) ) ;
#18930 = ADVANCED_BREP_SHAPE_REPRESENTATION ( '', ( #21737, #13190 ), #6882 ) ;
#18931 = ORIENTED_EDGE ( 'NONE', *, *, #19310, .F. ) ;
#18932 = DIRECTION ( 'NONE',  ( 2.698458740408365879E-16, -1.000000000000000000, 0.000000000000000000 ) ) ;
#18933 = ORIENTED_EDGE ( 'NONE', *, *, #11317, .F. ) ;
#18934 = CARTESIAN_POINT ( 'NONE',  ( 10.45306510330410177, 16.53912159438435125, -17.34933906371858114 ) ) ;
#18935 = ORIENTED_EDGE ( 'NONE', *, *, #8623, .F. ) ;
#18936 = CARTESIAN_POINT ( 'NONE',  ( 36.54859390953724585, -22.18451583373416014, -18.19919658220850778 ) ) ;
#18937 = CARTESIAN_POINT ( 'NONE',  ( 24.68825858685077179, -9.385095155728059524, -16.92495907518576104 ) ) ;
#18938 = CARTESIAN_POINT ( 'NONE',  ( 23.21730923944814506, -4.364887171357101359, -13.63095412955673247 ) ) ;
#18939 = EDGE_CURVE ( 'NONE', #23167, #26513, #2707, .T. ) ;
#18940 = PLANE ( 'NONE',  #2839 ) ;
#18941 = EDGE_CURVE ( 'NONE', #10103, #16958, #4988, .T. ) ;
#18942 = EDGE_CURVE ( 'NONE', #4384, #20699, #28075, .T. ) ;
#18943 = EDGE_CURVE ( 'NONE', #4151, #22156, #2572, .T. ) ;
#18944 = CARTESIAN_POINT ( 'NONE',  ( 34.63381380623899020, -13.58242311684542081, -20.01117170570581649 ) ) ;
#18945 = APPLICATION_PROTOCOL_DEFINITION ( 'draft international standard', 'automotive_design', 1998, #12991 ) ;
#18946 = CARTESIAN_POINT ( 'NONE',  ( 26.35635630057183576, -13.06715036242849948, -16.03892985609963873 ) ) ;
#18947 = AXIS2_PLACEMENT_3D ( 'NONE', #26641, #5722, #7994 ) ;
#18948 = CARTESIAN_POINT ( 'NONE',  ( 29.29807706749550889, -8.594015191909356588, -15.50881839395299444 ) ) ;
#18949 = ORIENTED_EDGE ( 'NONE', *, *, #20270, .T. ) ;
#18950 = FACE_BOUND ( 'NONE', #26264, .T. ) ;
#18951 = VECTOR ( 'NONE', #23968, 1000.000000000000000 ) ;
#18952 = CARTESIAN_POINT ( 'NONE',  ( 151.1922820468853956, -1.999999999999976241, -13.59645775552055902 ) ) ;
#18953 = CARTESIAN_POINT ( 'NONE',  ( 133.7287565553229172, -4.000000000000003553, -33.50000000000000000 ) ) ;
#18954 = CARTESIAN_POINT ( 'NONE',  ( 174.5152310637604671, -4.999999999999970690, -1.937508276747662207E-14 ) ) ;
#18955 = DIRECTION ( 'NONE',  ( -0.000000000000000000, -0.000000000000000000, -1.000000000000000000 ) ) ;
#18956 = CARTESIAN_POINT ( 'NONE',  ( 10.71920666609040573, 16.63846344887410922, -15.95486870256106648 ) ) ;
#18957 = CARTESIAN_POINT ( 'NONE',  ( 162.2287565553228887, -1.999999999999973133, -3.509618943233403510 ) ) ;
#18958 = VECTOR ( 'NONE', #3100, 1000.000000000000000 ) ;
#18959 = CARTESIAN_POINT ( 'NONE',  ( 161.1922820468853956, -4.999999999999973355, -28.06379628232387802 ) ) ;
#18960 = EDGE_LOOP ( 'NONE', ( #25568, #9189, #13352, #18771 ) ) ;
#18961 = CARTESIAN_POINT ( 'NONE',  ( 9.916953853453376766, 16.40494045485788632, -16.50434094533541085 ) ) ;
#18962 = ORIENTED_EDGE ( 'NONE', *, *, #29324, .F. ) ;
#18963 = CARTESIAN_POINT ( 'NONE',  ( 9.667670487869566287, 16.22828475907693146, -17.88517164372263579 ) ) ;
#18964 = CARTESIAN_POINT ( 'NONE',  ( 20.76503381105741397, 0.5146303624313508518, -20.54264311693622602 ) ) ;
#18965 = DIRECTION ( 'NONE',  ( -2.698458740408365879E-16, 1.000000000000000000, 0.000000000000000000 ) ) ;
#18966 = CARTESIAN_POINT ( 'NONE',  ( 133.7287565553229740, -84.33034373659253902, 8.500000000000003553 ) ) ;
#18967 = CARTESIAN_POINT ( 'NONE',  ( 26.32595758385100382, -12.12905223104374386, -14.21117607008287642 ) ) ;
#18968 = AXIS2_PLACEMENT_3D ( 'NONE', #24852, #22405, #10798 ) ;
#18969 = ORIENTED_EDGE ( 'NONE', *, *, #374, .T. ) ;
#18970 = DIRECTION ( 'NONE',  ( -0.5877852522924731371, -1.586114251531760728E-16, -0.8090169943749474513 ) ) ;
#18971 = CARTESIAN_POINT ( 'NONE',  ( 11.05541802266494855, 17.68941098027438841, -17.91029082024824959 ) ) ;
#18972 = ORIENTED_EDGE ( 'NONE', *, *, #18420, .T. ) ;
#18973 = CARTESIAN_POINT ( 'NONE',  ( 33.23402178976249388, -11.79005478413273522, -18.03234444571244666 ) ) ;
#18974 = CARTESIAN_POINT ( 'NONE',  ( 133.6922820468854241, -4.999999999999982236, -35.24709285013155835 ) ) ;
#18975 = ORIENTED_EDGE ( 'NONE', *, *, #5508, .T. ) ;
#18976 = EDGE_CURVE ( 'NONE', #14016, #20426, #2419, .T. ) ;
#18977 = LINE ( 'NONE', #521, #20824 ) ;
#18978 = CARTESIAN_POINT ( 'NONE',  ( 9.144997394934375023, 16.03247451896970688, -17.04129840131518492 ) ) ;
#18979 = CARTESIAN_POINT ( 'NONE',  ( 28.04121823296437199, -4.154284946049297211, -14.96295611916008994 ) ) ;
#18980 = EDGE_CURVE ( 'NONE', #15766, #3931, #21311, .T. ) ;
#18981 = ORIENTED_EDGE ( 'NONE', *, *, #28189, .F. ) ;
#18982 = ADVANCED_FACE ( 'NONE', ( #15978, #16129 ), #18726, .T. ) ;
#18983 = CARTESIAN_POINT ( 'NONE',  ( 142.0152310637606092, -4.999999999999979572, -32.93883019725009120 ) ) ;
#18984 = PRESENTATION_STYLE_ASSIGNMENT (( #9814 ) ) ;
#18985 = CARTESIAN_POINT ( 'NONE',  ( 20.37871551743239351, 7.600776799596193456, -17.08157252577618479 ) ) ;
#18986 = CARTESIAN_POINT ( 'NONE',  ( 17.68287507214707688, 6.939063861736925354, -15.39301800483504934 ) ) ;
#18987 = ORIENTED_EDGE ( 'NONE', *, *, #19402, .T. ) ;
#18988 = CARTESIAN_POINT ( 'NONE',  ( 20.00000000000000711, 60.00000000000000711, 29.99999999999998579 ) ) ;
#18989 = VECTOR ( 'NONE', #278, 1000.000000000000000 ) ;
#18990 = DIRECTION ( 'NONE',  ( 0.5877852522924731371, 1.586114251531760728E-16, -0.8090169943749474513 ) ) ;
#18991 = PRESENTATION_LAYER_ASSIGNMENT (  '', '', ( #19945 ) ) ;
#18992 = DIRECTION ( 'NONE',  ( 1.110223024625156540E-16, 2.995891024602366092E-32, 1.000000000000000000 ) ) ;
#18993 = CARTESIAN_POINT ( 'NONE',  ( 157.0152310637605808, -1.999999999999973133, -32.93883019725009120 ) ) ;
#18994 = DIRECTION ( 'NONE',  ( 1.110223024625156540E-16, 2.995891024602366092E-32, 1.000000000000000000 ) ) ;
#18995 = CARTESIAN_POINT ( 'NONE',  ( 9.641364314812712166, 17.66882920855936590, -17.90209449470656722 ) ) ;
#18996 = CARTESIAN_POINT ( 'NONE',  ( 28.63694740700460173, -9.765300015774602826, -17.75617681614052046 ) ) ;
#18997 = CARTESIAN_POINT ( 'NONE',  ( 24.38930386813997586, -0.5518329404549096040, -18.38842912410832753 ) ) ;
#18998 = ADVANCED_FACE ( 'NONE', ( #11993 ), #25450, .T. ) ;
#19000 = EDGE_LOOP ( 'NONE', ( #24586, #13434, #9659, #10022 ) ) ;
#18999 = CARTESIAN_POINT ( 'NONE',  ( 36.54859105337858693, -23.18450300252589003, -18.42496455282032386 ) ) ;
#19001 = LINE ( 'NONE', #11817, #30078 ) ;
#19002 = CARTESIAN_POINT ( 'NONE',  ( 18.62881505491278489, -5.000000000000012434, -57.33359741158763256 ) ) ;
#19003 = CARTESIAN_POINT ( 'NONE',  ( 148.6922820468853672, -10.00000000000000355, 2.247092850131519715 ) ) ;
#19004 = LINE ( 'NONE', #19151, #7581 ) ;
#19005 = CARTESIAN_POINT ( 'NONE',  ( 17.54642605795894994, 9.676486402519270058, -18.74681543856335608 ) ) ;
#19006 = ORIENTED_EDGE ( 'NONE', *, *, #24360, .F. ) ;
#19007 = LINE ( 'NONE', #16564, #28109 ) ;
#19008 = CARTESIAN_POINT ( 'NONE',  ( 10.33811696370167077, 18.38618940166710303, -17.91541423781815112 ) ) ;
#19009 = VECTOR ( 'NONE', #21048, 1000.000000000000000 ) ;
#19010 = FACE_OUTER_BOUND ( 'NONE', #1120, .T. ) ;
#19011 = DIRECTION ( 'NONE',  ( 0.3090169943749475623, 8.338696094058001131E-17, 0.9510565162951536422 ) ) ;
#19012 = CARTESIAN_POINT ( 'NONE',  ( 17.78594395145776019, 10.14170102421038422, -17.68001733040774681 ) ) ;
#19013 = ORIENTED_EDGE ( 'NONE', *, *, #11814, .T. ) ;
#19014 = VECTOR ( 'NONE', #17555, 1000.000000000000000 ) ;
#19015 = CARTESIAN_POINT ( 'NONE',  ( 13.46306793452363770, 5.846312397186087750, -15.11995136480861746 ) ) ;
#19016 = VECTOR ( 'NONE', #22530, 1000.000000000000000 ) ;
#19017 = ORIENTED_EDGE ( 'NONE', *, *, #4534, .F. ) ;
#19018 = CARTESIAN_POINT ( 'NONE',  ( 35.22227017426903473, -20.71851614966110233, -20.19360243392694088 ) ) ;
#19019 = CARTESIAN_POINT ( 'NONE',  ( 24.12901349891383163, -0.6887463444711696692, -16.28517635256633156 ) ) ;
#19020 = CARTESIAN_POINT ( 'NONE',  ( 18.67986154365276619, -0.9315889389632653339, -17.94220784458306994 ) ) ;
#19021 = CARTESIAN_POINT ( 'NONE',  ( 30.18376337559066158, -9.479172175342087669, -16.86143889264288021 ) ) ;
#19022 = VECTOR ( 'NONE', #1750, 1000.000000000000000 ) ;
#19023 = VERTEX_POINT ( 'NONE', #11539 ) ;
#19024 = EDGE_LOOP ( 'NONE', ( #24573, #29145, #27519, #15369 ) ) ;
#19025 = CARTESIAN_POINT ( 'NONE',  ( 154.5152310637605524, -1.999999999999974465, -19.94844914048349693 ) ) ;
#19026 = FACE_OUTER_BOUND ( 'NONE', #27367, .T. ) ;
#19027 = CARTESIAN_POINT ( 'NONE',  ( 154.5152310637604955, -10.00000000000000178, -2.627941064794695691 ) ) ;
#19028 = DIRECTION ( 'NONE',  ( 0.5877852522924731371, 0.000000000000000000, 0.8090169943749474513 ) ) ;
#19029 = EDGE_CURVE ( 'NONE', #23789, #17928, #4542, .T. ) ;
#19030 = CARTESIAN_POINT ( 'NONE',  ( 34.85979932414094407, -13.59765634092047470, -19.03716015824713281 ) ) ;
#19031 = CARTESIAN_POINT ( 'NONE',  ( 9.642214727206800617, 17.66492910891761525, -17.80644250212319690 ) ) ;
#19032 = EDGE_LOOP ( 'NONE', ( #18560, #18425, #17729, #16195 ) ) ;
#19033 = LINE ( 'NONE', #6847, #12710 ) ;
#19034 = CARTESIAN_POINT ( 'NONE',  ( 148.6922820468854525, -1.999999999999976241, -35.24709285013155835 ) ) ;
#19035 = CARTESIAN_POINT ( 'NONE',  ( 12.03055882466574289, 9.304755949677762317, -16.69027714870545864 ) ) ;
#19036 = CARTESIAN_POINT ( 'NONE',  ( 137.0152310637605808, -4.999999999999980460, 1.702185954127501066 ) ) ;
#19037 = CARTESIAN_POINT ( 'NONE',  ( 132.0152310637605524, -1.999999999999981348, -17.38167787843870826 ) ) ;
#19038 = VECTOR ( 'NONE', #23786, 1000.000000000000000 ) ;
#19039 = EDGE_LOOP ( 'NONE', ( #24324, #30255, #22041, #13731 ) ) ;
#19040 = VECTOR ( 'NONE', #172, 999.9999999999998863 ) ;
#19041 = DIRECTION ( 'NONE',  ( 0.5877852522924731371, 0.000000000000000000, 0.8090169943749474513 ) ) ;
#19042 = ORIENTED_EDGE ( 'NONE', *, *, #7571, .T. ) ;
#19043 = CARTESIAN_POINT ( 'NONE',  ( 167.2287565553228887, -1.999999999999971800, -3.509618943233403510 ) ) ;
#19044 = VERTEX_POINT ( 'NONE', #18576 ) ;
#19045 = CARTESIAN_POINT ( 'NONE',  ( 130.7287565553229172, -9.999999999999982236, -33.50000000000000000 ) ) ;
#19046 = ORIENTED_EDGE ( 'NONE', *, *, #6194, .T. ) ;
#19047 = CARTESIAN_POINT ( 'NONE',  ( 11.24427277393626134, 9.004760228429224966, -17.23264536074314179 ) ) ;
#19048 = CARTESIAN_POINT ( 'NONE',  ( 24.00126410897001605, -3.753019607378720757, -14.48453144943877113 ) ) ;
#19049 = CARTESIAN_POINT ( 'NONE',  ( 24.70156281743647142, 0.04986695427254615731, -17.03102378627558977 ) ) ;
#19050 = LINE ( 'NONE', #12174, #5286 ) ;
#19051 = LINE ( 'NONE', #25779, #15523 ) ;
#19052 = CARTESIAN_POINT ( 'NONE',  ( 152.0152310637604955, -1.999999999999975797, -8.721423840594312082 ) ) ;
#19053 = CARTESIAN_POINT ( 'NONE',  ( 173.6922820468852819, -4.999999999999971578, -9.266330736598359152 ) ) ;
#19054 = AXIS2_PLACEMENT_3D ( 'NONE', #8336, #3921, #4069 ) ;
#19055 = DIRECTION ( 'NONE',  ( 0.3090169943749472292, 8.338696094057992503E-17, -0.9510565162951536422 ) ) ;
#19056 = DIRECTION ( 'NONE',  ( -2.698458740408365879E-16, 1.000000000000000000, -0.000000000000000000 ) ) ;
#19057 = VECTOR ( 'NONE', #11675, 1000.000000000000000 ) ;
#19058 = CARTESIAN_POINT ( 'NONE',  ( 25.00000000000000000, 60.00000000000000711, -24.99999999999999289 ) ) ;
#19059 = FACE_OUTER_BOUND ( 'NONE', #14644, .T. ) ;
#19060 = CARTESIAN_POINT ( 'NONE',  ( 12.02406503409520333, 9.334315655862766903, -16.69297946412503819 ) ) ;
#19061 = EDGE_CURVE ( 'NONE', #28345, #14964, #27925, .T. ) ;
#19062 = ADVANCED_FACE ( 'NONE', ( #25305 ), #6985, .T. ) ;
#19063 = DIRECTION ( 'NONE',  ( -2.698458740408365879E-16, 1.000000000000000000, 0.000000000000000000 ) ) ;
#19064 = CARTESIAN_POINT ( 'NONE',  ( 34.93238815599637803, -19.41622979634004764, -20.17168434421570922 ) ) ;
#19065 = ORIENTED_EDGE ( 'NONE', *, *, #19310, .T. ) ;
#19066 = CARTESIAN_POINT ( 'NONE',  ( 13.92371455371928590, 7.866402339252101861, -15.27421329262669936 ) ) ;
#19067 = EDGE_CURVE ( 'NONE', #8041, #14150, #27623, .T. ) ;
#19068 = VERTEX_POINT ( 'NONE', #20853 ) ;
#19069 = DIRECTION ( 'NONE',  ( 0.9510565162951535312, 2.566386769018988816E-16, -0.3090169943749475623 ) ) ;
#19070 = EDGE_CURVE ( 'NONE', #19198, #12834, #9248, .T. ) ;
#19071 = CARTESIAN_POINT ( 'NONE',  ( 17.88091890332929523, 4.544920326333207861, -13.91018511019278669 ) ) ;
#19072 = CARTESIAN_POINT ( 'NONE',  ( 12.70256148071318414, 10.13540111970991653, -16.19467101188346092 ) ) ;
#19073 = DIRECTION ( 'NONE',  ( -0.9510565162951536422, -2.566386769018988323E-16, 0.3090169943749475623 ) ) ;
#19074 = ORIENTED_EDGE ( 'NONE', *, *, #28317, .T. ) ;
#19075 = ORIENTED_EDGE ( 'NONE', *, *, #12409, .T. ) ;
#19076 = CARTESIAN_POINT ( 'NONE',  ( 11.44040408106239326, 9.418203516307107392, -15.87434068686103394 ) ) ;
#19077 = CARTESIAN_POINT ( 'NONE',  ( 148.6922820468854241, -10.00000000000000178, -15.07341522555727664 ) ) ;
#19078 = CARTESIAN_POINT ( 'NONE',  ( 9.914377700407460026, 16.41675502110963336, -16.50544604630902867 ) ) ;
#19079 = CARTESIAN_POINT ( 'NONE',  ( 1.321505333908960633, -3.855830693249187480, -2.415789719053445417 ) ) ;
#19080 = ORIENTED_EDGE ( 'NONE', *, *, #23918, .T. ) ;
#19081 = FACE_OUTER_BOUND ( 'NONE', #2576, .T. ) ;
#19082 = ORIENTED_EDGE ( 'NONE', *, *, #2755, .T. ) ;
#19083 = CARTESIAN_POINT ( 'NONE',  ( 10.35865266338826984, 16.97210907862488938, -17.91126819201198472 ) ) ;
#19084 = VERTEX_POINT ( 'NONE', #16275 ) ;
#19086 = AXIS2_PLACEMENT_3D ( 'NONE', #26338, #15760, #3883 ) ;
#19085 = CARTESIAN_POINT ( 'NONE',  ( 36.12281451779777797, -20.27171456826661355, -20.44288436412734100 ) ) ;
#19087 = CARTESIAN_POINT ( 'NONE',  ( 28.75197783424699693, -9.407057218516385433, -18.70835418409691542 ) ) ;
#19088 = CARTESIAN_POINT ( 'NONE',  ( 26.08768104250457753, -11.87935956797728210, -17.28510650846989805 ) ) ;
#19089 = CARTESIAN_POINT ( 'NONE',  ( 148.6922820468854241, -4.999999999999976907, -15.07341522555727664 ) ) ;
#19090 = CARTESIAN_POINT ( 'NONE',  ( 33.19592593216645326, -10.35933293216661610, -17.69446280125821147 ) ) ;
#19091 = DIRECTION ( 'NONE',  ( 0.000000000000000000, 0.000000000000000000, -1.000000000000000000 ) ) ;
#19092 = CARTESIAN_POINT ( 'NONE',  ( 19.55510877418759819, -0.09764134006120470111, -19.21341144728512518 ) ) ;
#19093 = CARTESIAN_POINT ( 'NONE',  ( 29.00298259868716499, -8.617193473538632631, -14.90553363820342092 ) ) ;
#19094 = VERTEX_POINT ( 'NONE', #21012 ) ;
#19095 = FACE_BOUND ( 'NONE', #24946, .T. ) ;
#19096 = VECTOR ( 'NONE', #21040, 1000.000000000000000 ) ;
#19097 = CARTESIAN_POINT ( 'NONE',  ( 0.000000000000000000, 0.000000000000000000, 9.480888224575629408 ) ) ;
#19098 = FACE_OUTER_BOUND ( 'NONE', #8846, .T. ) ;
#19099 = DIRECTION ( 'NONE',  ( -0.8090169943749474513, -2.183098979609982436E-16, -0.5877852522924731371 ) ) ;
#19100 = ADVANCED_FACE ( 'NONE', ( #11697 ), #25588, .T. ) ;
#19101 = DIRECTION ( 'NONE',  ( -0.5877852522924731371, -1.586114251531760235E-16, 0.8090169943749474513 ) ) ;
#19102 = ADVANCED_FACE ( 'NONE', ( #18426 ), #23019, .T. ) ;
#19103 = ADVANCED_FACE ( 'NONE', ( #21155 ), #269, .T. ) ;
#19104 = CARTESIAN_POINT ( 'NONE',  ( 12.27593128402378753, 9.499125914797495795, -15.31109449298900671 ) ) ;
#19105 = ADVANCED_FACE ( 'NONE', ( #8022 ), #21658, .F. ) ;
#19106 = CARTESIAN_POINT ( 'NONE',  ( -3.469446951953614189E-15, -4.618802153517058251, -2.450000000000000178 ) ) ;
#19107 = EDGE_LOOP ( 'NONE', ( #26847, #2762, #2984, #4095 ) ) ;
#19108 = CARTESIAN_POINT ( 'NONE',  ( 156.1922820468854241, -10.00000000000000000, -30.91696583120936026 ) ) ;
#19109 = VERTEX_POINT ( 'NONE', #14581 ) ;
#19110 = CARTESIAN_POINT ( 'NONE',  ( 11.39177520167864266, 9.641221755901229429, -15.89445043910815336 ) ) ;
#19111 = EDGE_LOOP ( 'NONE', ( #18060, #12655, #12272, #13268 ) ) ;
#19112 = CARTESIAN_POINT ( 'NONE',  ( 20.46796597391333350, 5.758383238370681667, -16.38968713894368534 ) ) ;
#19113 = CARTESIAN_POINT ( 'NONE',  ( 31.84774147790582433, -10.54213090804960018, -15.00000000011102763 ) ) ;
#19114 = CARTESIAN_POINT ( 'NONE',  ( 142.0152310637605808, -4.999999999999979572, -34.70218595412750773 ) ) ;
#19115 = CARTESIAN_POINT ( 'NONE',  ( 164.5152310637604671, -4.999999999999973355, -2.627941064794695691 ) ) ;
#19116 = DIRECTION ( 'NONE',  ( 1.000000000000000000, 0.000000000000000000, 0.000000000000000000 ) ) ;
#19117 = CARTESIAN_POINT ( 'NONE',  ( 11.28117986039200815, 16.65403841451731637, -16.78246231193739035 ) ) ;
#19118 = VERTEX_POINT ( 'NONE', #26062 ) ;
#19119 = CARTESIAN_POINT ( 'NONE',  ( 33.66936448658974257, -12.74213349194280553, -18.74758104053764995 ) ) ;
#19120 = CARTESIAN_POINT ( 'NONE',  ( 19.91209246711783010, 5.411768277715644615, -14.29674560697521457 ) ) ;
#19121 = CARTESIAN_POINT ( 'NONE',  ( 167.2287565553229172, -1.999999999999971356, -12.16987298107780369 ) ) ;
#19122 = VECTOR ( 'NONE', #10030, 1000.000000000000000 ) ;
#19123 = CARTESIAN_POINT ( 'NONE',  ( 9.098468484354940600, 16.24586203394349582, -17.06302340752861824 ) ) ;
#19124 = CARTESIAN_POINT ( 'NONE',  ( 30.28780241637438664, -8.987295266975118935, -19.34112676082218840 ) ) ;
#19125 = VERTEX_POINT ( 'NONE', #19471 ) ;
#19126 = PLANE ( 'NONE',  #25196 ) ;
#19127 = CARTESIAN_POINT ( 'NONE',  ( 21.10828700581006601, 3.717818950362942854, -18.90958453460783417 ) ) ;
#19128 = CARTESIAN_POINT ( 'NONE',  ( 18.48188012193690710, 6.385789046977964567, -18.71539758422269628 ) ) ;
#19129 = DIRECTION ( 'NONE',  ( -1.000000000000000000, 0.000000000000000000, 0.000000000000000000 ) ) ;
#19130 = ORIENTED_EDGE ( 'NONE', *, *, #29961, .T. ) ;
#19131 = DIRECTION ( 'NONE',  ( 0.5877852522924731371, 1.586114251531760728E-16, 0.8090169943749474513 ) ) ;
#19132 = AXIS2_PLACEMENT_3D ( 'NONE', #9430, #19055, #28107 ) ;
#19133 = LINE ( 'NONE', #7840, #6520 ) ;
#19134 = DIRECTION ( 'NONE',  ( 2.207829878515935943E-16, 1.000000000000000000, 0.000000000000000000 ) ) ;
#19135 = CARTESIAN_POINT ( 'NONE',  ( 133.7287565553229740, -84.33034373659253902, 0.5000000000000029976 ) ) ;
#19136 = EDGE_CURVE ( 'NONE', #2732, #18869, #30008, .T. ) ;
#19137 = ADVANCED_FACE ( 'NONE', ( #28530 ), #872, .T. ) ;
#19138 = CARTESIAN_POINT ( 'NONE',  ( 159.7287565553229740, -9.999999999999998224, -25.16025403784440329 ) ) ;
#19139 = ORIENTED_EDGE ( 'NONE', *, *, #11899, .F. ) ;
#19140 = VECTOR ( 'NONE', #3634, 1000.000000000000114 ) ;
#19141 = EDGE_CURVE ( 'NONE', #12198, #4291, #5296, .T. ) ;
#19142 = CARTESIAN_POINT ( 'NONE',  ( 9.910898653440767703, 16.43271037397421708, -16.50709950392603531 ) ) ;
#19143 = ADVANCED_FACE ( 'NONE', ( #24221 ), #9861, .T. ) ;
#19144 = CARTESIAN_POINT ( 'NONE',  ( 27.63516133065608926, -10.68623331565014034, -17.71408682504818088 ) ) ;
#19145 = CARTESIAN_POINT ( 'NONE',  ( 19.75232399841803854, 1.290101960903724754, -14.36573431580270999 ) ) ;
#19147 = ORIENTED_EDGE ( 'NONE', *, *, #19616, .F. ) ;
#19146 = CARTESIAN_POINT ( 'NONE',  ( 34.84906220094974572, -20.04189041930405324, -21.18881845514476581 ) ) ;
#19148 = PLANE ( 'NONE',  #12973 ) ;
#19149 = FACE_OUTER_BOUND ( 'NONE', #10825, .T. ) ;
#19150 = CARTESIAN_POINT ( 'NONE',  ( 172.7287565553229456, -9.999999999999980460, 0.5000000000000029976 ) ) ;
#19151 = CARTESIAN_POINT ( 'NONE',  ( 152.2287565553229456, -1.999999999999975797, -3.509618943233403510 ) ) ;
#19152 = CARTESIAN_POINT ( 'NONE',  ( 18.55171814111300321, 6.637122934506423988, -19.73184648383247364 ) ) ;
#19153 = ORIENTED_EDGE ( 'NONE', *, *, #2235, .F. ) ;
#19154 = LINE ( 'NONE', #16408, #27627 ) ;
#19155 = CARTESIAN_POINT ( 'NONE',  ( 10.33830461362823883, 18.38532881518400686, -17.85494544563047370 ) ) ;
#19156 = LINE ( 'NONE', #9530, #3717 ) ;
#19157 = DIRECTION ( 'NONE',  ( 0.5877852522924731371, 1.586114251531760728E-16, -0.8090169943749474513 ) ) ;
#19158 = VECTOR ( 'NONE', #17219, 1000.000000000000000 ) ;
#19159 = CARTESIAN_POINT ( 'NONE',  ( 19.05868480923028940, 8.129737193291200370, -16.02886444249750042 ) ) ;
#19160 = CARTESIAN_POINT ( 'NONE',  ( 15.74206018803408469, 8.560804325426111916, -21.16119476544194100 ) ) ;
#19161 = ORIENTED_EDGE ( 'NONE', *, *, #27287, .F. ) ;
#19162 = CARTESIAN_POINT ( 'NONE',  ( 33.68411698100747032, -13.80840863474736935, -19.79436191385186916 ) ) ;
#19163 = CARTESIAN_POINT ( 'NONE',  ( 21.44242187996815119, -3.785596145164559445, -16.19382493935754397 ) ) ;
#19164 = CARTESIAN_POINT ( 'NONE',  ( 21.26848695057635297, 1.468789200266592099, -19.53654423682621299 ) ) ;
#19165 = VECTOR ( 'NONE', #11099, 1000.000000000000000 ) ;
#19166 = ORIENTED_EDGE ( 'NONE', *, *, #9869, .T. ) ;
#19167 = CARTESIAN_POINT ( 'NONE',  ( 26.63012090756776828, -10.30360588212082007, -13.56444477573641905 ) ) ;
#19168 = VERTEX_POINT ( 'NONE', #12752 ) ;
#19169 = ORIENTED_EDGE ( 'NONE', *, *, #29830, .F. ) ;
#19170 = DIRECTION ( 'NONE',  ( 0.000000000000000000, 0.000000000000000000, 1.000000000000000000 ) ) ;
#19171 = CARTESIAN_POINT ( 'NONE',  ( 120.0000000000000000, 20.00000000000000355, -17.99999999999998934 ) ) ;
#19172 = DIRECTION ( 'NONE',  ( -1.000000000000000000, -4.440892098500622217E-16, 0.000000000000000000 ) ) ;
#19173 = EDGE_CURVE ( 'NONE', #13402, #26227, #7729, .T. ) ;
#19174 = CARTESIAN_POINT ( 'NONE',  ( 116.5082401878149909, -4.999999999999985789, -84.64819135951087503 ) ) ;
#19175 = B_SPLINE_CURVE_WITH_KNOTS ( 'NONE', 3,
 ( #25059, #11157, #328, #27982, #9310, #5193, #16189, #12054 ),
 .UNSPECIFIED., .F., .F.,
 ( 4, 2, 2, 4 ),
 ( 0.004673709593152178265, 0.005837709341827659881, 0.007001709090503141497, 0.009329708587854104729 ),
 .UNSPECIFIED. ) ;
#19176 = CARTESIAN_POINT ( 'NONE',  ( 31.87116100697361887, -10.15812870475309815, -13.95024105943860171 ) ) ;
#19177 = CARTESIAN_POINT ( 'NONE',  ( 9.641350810849047548, 17.66889113945805789, -23.00000000000000711 ) ) ;
#19178 = AXIS2_PLACEMENT_3D ( 'NONE', #26947, #8577, #14991 ) ;
#19179 = DIRECTION ( 'NONE',  ( 0.000000000000000000, 0.000000000000000000, 1.000000000000000000 ) ) ;
#19180 = CARTESIAN_POINT ( 'NONE',  ( 99.12450160535630062, -4.999999999999990230, 72.01816598362702848 ) ) ;
#19181 = CARTESIAN_POINT ( 'NONE',  ( 12.01798642417223739, 9.362192935812041483, -16.69549318315592856 ) ) ;
#19182 = CARTESIAN_POINT ( 'NONE',  ( 133.7287565553229456, -4.999999999999982236, 3.500000000000003109 ) ) ;
#19183 = FACE_OUTER_BOUND ( 'NONE', #16578, .T. ) ;
#19184 = ORIENTED_EDGE ( 'NONE', *, *, #18063, .T. ) ;
#19185 = LINE ( 'NONE', #3185, #27126 ) ;
#19186 = DIRECTION ( 'NONE',  ( -0.9510565162951536422, -2.566386769018988323E-16, 0.3090169943749475623 ) ) ;
#19187 = EDGE_LOOP ( 'NONE', ( #7386, #17533, #1991, #5610 ) ) ;
#19188 = VERTEX_POINT ( 'NONE', #24071 ) ;
#19189 = ORIENTED_EDGE ( 'NONE', *, *, #7876, .F. ) ;
#19190 = CARTESIAN_POINT ( 'NONE',  ( 11.21994398240249957, 9.109360644301018439, -17.24323810967081982 ) ) ;
#19191 = CARTESIAN_POINT ( 'NONE',  ( 22.62754675296084983, -4.373583220233932423, -15.05708262856468060 ) ) ;
#19192 = CARTESIAN_POINT ( 'NONE',  ( 24.47846259200217034, 0.2319951948203725633, -15.89054235832688278 ) ) ;
#19193 = FACE_OUTER_BOUND ( 'NONE', #7002, .T. ) ;
#19194 = FACE_OUTER_BOUND ( 'NONE', #27225, .T. ) ;
#19195 = CARTESIAN_POINT ( 'NONE',  ( 2.500000000000000444, 2.357898499370430834, -3.469446951953614189E-15 ) ) ;
#19196 = EDGE_CURVE ( 'NONE', #15051, #8663, #2868, .T. ) ;
#19197 = AXIS2_PLACEMENT_3D ( 'NONE', #22570, #10950, #15825 ) ;
#19198 = VERTEX_POINT ( 'NONE', #7579 ) ;
#19199 = CARTESIAN_POINT ( 'NONE',  ( 142.0152310637605808, -10.00000000000000355, -6.958068083716895558 ) ) ;
#19200 = CARTESIAN_POINT ( 'NONE',  ( 134.5152310637605808, -10.00000000000000533, -11.28819510263909187 ) ) ;
#19201 = LINE ( 'NONE', #7315, #10178 ) ;
#19202 = LINE ( 'NONE', #21643, #16096 ) ;
#19203 = DIRECTION ( 'NONE',  ( -0.8090169943749474513, -2.183098979609982436E-16, -0.5877852522924731371 ) ) ;
#19204 = CARTESIAN_POINT ( 'NONE',  ( 11.12037835888041393, 13.47873794165536410, -17.06668569338069830 ) ) ;
#19205 = CARTESIAN_POINT ( 'NONE',  ( -16.00000000000017053, 34.64101615137744972, -10.00000000000000000 ) ) ;
#19206 = CARTESIAN_POINT ( 'NONE',  ( 173.6922820468853672, -4.999999999999970690, -35.24709285013155835 ) ) ;
#19207 = ORIENTED_EDGE ( 'NONE', *, *, #18759, .F. ) ;
#19208 = CARTESIAN_POINT ( 'NONE',  ( 13.44731269622883296, 7.655871835264917102, -15.65391398210326201 ) ) ;
#19209 = CARTESIAN_POINT ( 'NONE',  ( 141.1922820468854241, -1.999999999999979128, -4.936203717676158398 ) ) ;
#19210 = CARTESIAN_POINT ( 'NONE',  ( 19.18841159021359033, -2.222386543571284179, -18.22349448661670834 ) ) ;
#19211 = CARTESIAN_POINT ( 'NONE',  ( 12.83225835781710344, 9.540595166069421040, -16.14103675596956933 ) ) ;
#19212 = DIRECTION ( 'NONE',  ( 0.000000000000000000, 0.000000000000000000, 1.000000000000000000 ) ) ;
#19213 = VERTEX_POINT ( 'NONE', #16882 ) ;
#19214 = CARTESIAN_POINT ( 'NONE',  ( 11.47269659055779378, 9.270105954394804115, -15.86098659800193644 ) ) ;
#19215 = CARTESIAN_POINT ( 'NONE',  ( 0.000000000000000000, 0.000000000000000000, 1.700000000000000178 ) ) ;
#19216 = VECTOR ( 'NONE', #5448, 1000.000000000000000 ) ;
#19217 = CARTESIAN_POINT ( 'NONE',  ( 9.920751600319857033, 16.38752350362809551, -16.50277044458016107 ) ) ;
#19218 = LINE ( 'NONE', #16934, #5744 ) ;
#19219 = ORIENTED_EDGE ( 'NONE', *, *, #12074, .T. ) ;
#19220 = ORIENTED_EDGE ( 'NONE', *, *, #21520, .F. ) ;
#19221 = CARTESIAN_POINT ( 'NONE',  ( -13.00000000000000178, 0.000000000000000000, -18.00000000000000000 ) ) ;
#19222 = EDGE_LOOP ( 'NONE', ( #27956, #10854, #18532, #9300 ) ) ;
#19223 = CARTESIAN_POINT ( 'NONE',  ( 13.09695832212169364, 8.559710067821024282, -15.93310406974445392 ) ) ;
#19224 = VERTEX_POINT ( 'NONE', #14729 ) ;
#19225 = CARTESIAN_POINT ( 'NONE',  ( 32.94969931363368687, -9.746457777152386370, -18.95700739231402920 ) ) ;
#19226 = CARTESIAN_POINT ( 'NONE',  ( 17.06037746458228810, 10.50611453990982191, -19.02300506704843741 ) ) ;
#19227 = CARTESIAN_POINT ( 'NONE',  ( 28.01381056668970260, -10.10121741814351459, -18.82353034625045041 ) ) ;
#19228 = ORIENTED_EDGE ( 'NONE', *, *, #10828, .F. ) ;
#19229 =( REPRESENTATION_RELATIONSHIP ('NONE','NONE', #5250, #17708 ) REPRESENTATION_RELATIONSHIP_WITH_TRANSFORMATION ( #21673 )SHAPE_REPRESENTATION_RELATIONSHIP( ) );
#19230 = CARTESIAN_POINT ( 'NONE',  ( -13.00000000000000178, -2.870178842070716726E-15, -23.00000000000000000 ) ) ;
#19231 = CARTESIAN_POINT ( 'NONE',  ( 33.25614251967556356, -10.36847857886694868, -17.86465469861353483 ) ) ;
#19232 = CONTEXT_DEPENDENT_SHAPE_REPRESENTATION ( #29217, #13255 ) ;
#19233 = EDGE_CURVE ( 'NONE', #10558, #29062, #23931, .T. ) ;
#19234 = ADVANCED_FACE ( 'NONE', ( #16740 ), #19620, .T. ) ;
#19235 = CARTESIAN_POINT ( 'NONE',  ( 16.89975486243277913, 3.514059009776604015, -17.86885937027150817 ) ) ;
#19236 = ADVANCED_FACE ( 'NONE', ( #3174 ), #3323, .T. ) ;
#19237 = CARTESIAN_POINT ( 'NONE',  ( 27.38292679376507266, -11.43094998702963849, -14.23096243513112036 ) ) ;
#19238 = EDGE_CURVE ( 'NONE', #11857, #17842, #711, .T. ) ;
#19239 =( LENGTH_UNIT ( ) NAMED_UNIT ( * ) SI_UNIT ( .MILLI., .METRE. ) );
#19240 = FACE_BOUND ( 'NONE', #12944, .T. ) ;
#19241 = VECTOR ( 'NONE', #2991, 1000.000000000000000 ) ;
#19242 = DIRECTION ( 'NONE',  ( -0.5877852522924731371, -1.586114251531760235E-16, 0.8090169943749474513 ) ) ;
#19243 = CARTESIAN_POINT ( 'NONE',  ( 136.1922820468854241, -4.999999999999981348, -22.25671179336495697 ) ) ;
#19244 = CARTESIAN_POINT ( 'NONE',  ( 144.5152310637605524, -4.999999999999978684, -13.05155085951651195 ) ) ;
#19245 = DIRECTION ( 'NONE',  ( -0.9510565162951536422, -2.566386769018988816E-16, -0.3090169943749472292 ) ) ;
#19246 = CARTESIAN_POINT ( 'NONE',  ( 12.27694278248960558, 9.494486990809335225, -15.31067620760345527 ) ) ;
#19247 = CARTESIAN_POINT ( 'NONE',  ( -5.354491962338132183, 6.146186931204415949, -0.06809871960543412150 ) ) ;
#19248 = EDGE_LOOP ( 'NONE', ( #14109, #28277 ) ) ;
#19249 = DIRECTION ( 'NONE',  ( 0.9510565162951536422, 0.000000000000000000, -0.3090169943749475623 ) ) ;
#19250 = ORIENTED_EDGE ( 'NONE', *, *, #14573, .T. ) ;
#19251 = CARTESIAN_POINT ( 'NONE',  ( 12.39803340617553928, 8.535179507765855433, -15.21071672276548625 ) ) ;
#19252 = CARTESIAN_POINT ( 'NONE',  ( 18.66675855576620791, -1.414919486740021881, -19.12600662388792117 ) ) ;
#19253 = DIRECTION ( 'NONE',  ( -2.698458740408365879E-16, 1.000000000000000000, 0.000000000000000000 ) ) ;
#19254 = LINE ( 'NONE', #16975, #22782 ) ;
#19255 = ORIENTED_EDGE ( 'NONE', *, *, #8578, .T. ) ;
#19256 = CARTESIAN_POINT ( 'NONE',  ( 19.10627256897540605, -5.000000000000012434, -58.80306054231878221 ) ) ;
#19257 = ORIENTED_EDGE ( 'NONE', *, *, #950, .F. ) ;
#19258 = CARTESIAN_POINT ( 'NONE',  ( 167.0152310637605524, -9.999999999999996447, -32.93883019725009120 ) ) ;
#19259 = CARTESIAN_POINT ( 'NONE',  ( 12.84300253770136990, 9.521034635873322216, -16.13432743836305505 ) ) ;
#19260 = EDGE_LOOP ( 'NONE', ( #10287, #22014, #3361, #3372 ) ) ;
#19261 = CARTESIAN_POINT ( 'NONE',  ( 33.61574637963836665, -12.50126044309498496, -18.73137083807847958 ) ) ;
#19262 = CARTESIAN_POINT ( 'NONE',  ( 16.57956996521092918, 4.788269978297743812, -19.71382457362092566 ) ) ;
#19263 = VERTEX_POINT ( 'NONE', #3462 ) ;
#19264 = AXIS2_PLACEMENT_3D ( 'NONE', #16964, #7215, #5822 ) ;
#19265 = FACE_OUTER_BOUND ( 'NONE', #15767, .T. ) ;
#19266 = CARTESIAN_POINT ( 'NONE',  ( 25.84292692831908766, -2.469955994367391661, -17.24682881138801704 ) ) ;
#19267 = ORIENTED_EDGE ( 'NONE', *, *, #30047, .F. ) ;
#19268 = DIRECTION ( 'NONE',  ( 0.000000000000000000, 0.000000000000000000, -1.000000000000000000 ) ) ;
#19269 = PRESENTATION_STYLE_ASSIGNMENT (( #24317 ) ) ;
#19270 = EDGE_CURVE ( 'NONE', #21626, #6687, #5138, .T. ) ;
#19271 = CARTESIAN_POINT ( 'NONE',  ( 24.59961324288297391, 0.2024632608770970121, -16.27125138369466484 ) ) ;
#19272 = EDGE_CURVE ( 'NONE', #23960, #16007, #3023, .T. ) ;
#19273 = CARTESIAN_POINT ( 'NONE',  ( 15.83821057800014920, 6.120979864746498578, -15.70533851924537672 ) ) ;
#19274 = EDGE_CURVE ( 'NONE', #756, #26426, #15035, .T. ) ;
#19275 = CARTESIAN_POINT ( 'NONE',  ( 173.6922820468853672, -9.999999999999994671, -35.24709285013155835 ) ) ;
#19276 = EDGE_CURVE ( 'NONE', #9240, #30179, #12298, .T. ) ;
#19277 = ORIENTED_EDGE ( 'NONE', *, *, #20034, .F. ) ;
#19278 = ORIENTED_EDGE ( 'NONE', *, *, #23377, .F. ) ;
#19279 = LINE ( 'NONE', #18829, #10723 ) ;
#19280 = VECTOR ( 'NONE', #5002, 1000.000000000000000 ) ;
#19281 = FACE_OUTER_BOUND ( 'NONE', #16688, .T. ) ;
#19282 = DIRECTION ( 'NONE',  ( -2.698458740408365879E-16, 1.000000000000000000, 0.000000000000000000 ) ) ;
#19283 = FACE_OUTER_BOUND ( 'NONE', #12862, .T. ) ;
#19284 = AXIS2_PLACEMENT_3D ( 'NONE', #25130, #11515, #4074 ) ;
#19285 = CARTESIAN_POINT ( 'NONE',  ( 143.6922820468853956, -1.999999999999978462, 2.247092850131521491 ) ) ;
#19286 = AXIS2_PLACEMENT_3D ( 'NONE', #9598, #5339, #2756 ) ;
#19287 = CARTESIAN_POINT ( 'NONE',  ( 11.46775782571576130, 9.292755756535285627, -15.86302895122203616 ) ) ;
#19288 = CARTESIAN_POINT ( 'NONE',  ( 27.54771222089439320, -11.35863810494041459, -14.08592588049474692 ) ) ;
#19289 = CARTESIAN_POINT ( 'NONE',  ( 22.16683763302808430, -0.5050174593055701822, -13.96310542101677044 ) ) ;
#19291 = EDGE_LOOP ( 'NONE', ( #9414, #20129, #6240, #13102 ) ) ;
#19290 = CARTESIAN_POINT ( 'NONE',  ( 35.54859390953724585, -23.18451583373416014, -17.78191007148576119 ) ) ;
#19292 = CARTESIAN_POINT ( 'NONE',  ( 133.6922820468853956, -1.999999999999980904, -6.413161187712875133 ) ) ;
#19293 = DIRECTION ( 'NONE',  ( -2.698458740408365879E-16, 1.000000000000000000, 0.000000000000000000 ) ) ;
#19294 = CARTESIAN_POINT ( 'NONE',  ( -0.3263565795980836182, 4.430380094434250182, -2.201519936624996010 ) ) ;
#19295 = CARTESIAN_POINT ( 'NONE',  ( 125.7287565553229456, -84.33034373659255323, -33.50000000000000000 ) ) ;
#19296 = CYLINDRICAL_SURFACE ( 'NONE', #27371, 12.50000000000000000 ) ;
#19297 = FACE_BOUND ( 'NONE', #7392, .T. ) ;
#19298 = CARTESIAN_POINT ( 'NONE',  ( 23.36212950203212557, 2.915605996956767587, -15.34809340432955693 ) ) ;
#19299 = CARTESIAN_POINT ( 'NONE',  ( 151.1922820468854241, -1.999999999999976241, -28.06379628232387446 ) ) ;
#19300 = CARTESIAN_POINT ( 'NONE',  ( 10.33886748782435561, 18.38274740237080351, -17.79416814676874381 ) ) ;
#19301 = CARTESIAN_POINT ( 'NONE',  ( 130.7287565553229456, -4.999999999999983125, 3.500000000000003109 ) ) ;
#19302 = DIRECTION ( 'NONE',  ( -0.9510565162951536422, 0.000000000000000000, -0.3090169943749472292 ) ) ;
#19303 = AXIS2_PLACEMENT_3D ( 'NONE', #27464, #25569, #18553 ) ;
#19304 = CARTESIAN_POINT ( 'NONE',  ( 19.71807001554888217, -1.708786246101231532, -19.21472004699903380 ) ) ;
#19305 = CARTESIAN_POINT ( 'NONE',  ( 13.78422571733443647, 6.778978001458615843, -20.29761332830707232 ) ) ;
#19306 = EDGE_LOOP ( 'NONE', ( #15995, #5067, #3470, #18404, #25307 ) ) ;
#19307 = CARTESIAN_POINT ( 'NONE',  ( 33.27037009343090546, -12.05169513820189309, -19.60996450177851713 ) ) ;
#19308 = CARTESIAN_POINT ( 'NONE',  ( 27.22116495027615812, -8.412805768781604243, -11.93592671293571605 ) ) ;
#19309 = VECTOR ( 'NONE', #8449, 1000.000000000000000 ) ;
#19310 = EDGE_CURVE ( 'NONE', #3398, #18151, #13211, .T. ) ;
#19311 = CARTESIAN_POINT ( 'NONE',  ( 18.22321846687148650, 1.664438589611230812, -15.57940112478783945 ) ) ;
#19312 = EDGE_CURVE ( 'NONE', #13296, #19419, #11420, .T. ) ;
#19313 = PRESENTATION_LAYER_ASSIGNMENT (  '', '', ( #5174 ) ) ;
#19314 = EDGE_CURVE ( 'NONE', #25811, #28921, #8329, .T. ) ;
#19315 = EDGE_CURVE ( 'NONE', #10352, #28379, #12901, .T. ) ;
#19316 = CARTESIAN_POINT ( 'NONE',  ( 131.1922820468854241, -4.999999999999982236, -13.59645775552055547 ) ) ;
#19317 = CARTESIAN_POINT ( 'NONE',  ( 158.6922820468853956, -9.999999999999998224, -26.58683881228715862 ) ) ;
#19318 = LINE ( 'NONE', #26674, #10610 ) ;
#19319 = CARTESIAN_POINT ( 'NONE',  ( 0.000000000000000000, 0.000000000000000000, 0.000000000000000000 ) ) ;
#19320 = VECTOR ( 'NONE', #7084, 1000.000000000000000 ) ;
#19321 = CARTESIAN_POINT ( 'NONE',  ( 144.7287565553230309, -4.999999999999978684, -25.16025403784439973 ) ) ;
#19322 = CARTESIAN_POINT ( 'NONE',  ( 36.54859590101256828, -22.18452478037840336, -18.26685560724362034 ) ) ;
#19323 = VECTOR ( 'NONE', #9803, 1000.000000000000000 ) ;
#19324 = CARTESIAN_POINT ( 'NONE',  ( 9.641350810849047548, 17.66889113945805789, -17.91752729848689185 ) ) ;
#19325 = VECTOR ( 'NONE', #28164, 1000.000000000000000 ) ;
#19326 = DIRECTION ( 'NONE',  ( 0.9510565162951536422, 2.566386769018988816E-16, 0.3090169943749472292 ) ) ;
#19327 = DIRECTION ( 'NONE',  ( -2.698458740408365879E-16, 1.000000000000000000, 0.000000000000000000 ) ) ;
#19328 = CARTESIAN_POINT ( 'NONE',  ( 12.02932678857878734, 9.310239991255825132, -16.69079931733866218 ) ) ;
#19329 = DIRECTION ( 'NONE',  ( 0.3090169943749475623, 8.338696094058001131E-17, 0.9510565162951536422 ) ) ;
#19330 = CARTESIAN_POINT ( 'NONE',  ( 14.49336047848676223, -5.000000000000013323, -44.60597694298518689 ) ) ;
#19331 = ORIENTED_EDGE ( 'NONE', *, *, #11949, .T. ) ;
#19332 = DIRECTION ( 'NONE',  ( 1.110223024625156540E-16, 2.995891024602366092E-32, 1.000000000000000000 ) ) ;
#19333 = LINE ( 'NONE', #28857, #15640 ) ;
#19334 = CARTESIAN_POINT ( 'NONE',  ( 20.61759372714454841, -5.000000000000012434, -63.45442879020060900 ) ) ;
#19335 = ORIENTED_EDGE ( 'NONE', *, *, #5753, .T. ) ;
#19336 = VERTEX_POINT ( 'NONE', #19926 ) ;
#19337 = EDGE_LOOP ( 'NONE', ( #23970, #4906, #16681, #27062 ) ) ;
#19338 = CARTESIAN_POINT ( 'NONE',  ( 11.21386537247953363, 9.137237924250291243, -17.24575182870169598 ) ) ;
#19339 = CARTESIAN_POINT ( 'NONE',  ( 25.04368804655567970, -3.332730676350641463, -14.85212872609148427 ) ) ;
#19340 = EDGE_CURVE ( 'NONE', #3218, #288, #18084, .T. ) ;
#19341 = CARTESIAN_POINT ( 'NONE',  ( 22.96196402503608169, -2.069733343145511828, -19.51364111617685992 ) ) ;
#19342 = VECTOR ( 'NONE', #25849, 1000.000000000000000 ) ;
#19343 = FACE_OUTER_BOUND ( 'NONE', #29423, .T. ) ;
#19344 = DIRECTION ( 'NONE',  ( -0.9510565162951536422, -2.566386769018988323E-16, 0.3090169943749475623 ) ) ;
#19345 = EDGE_CURVE ( 'NONE', #1366, #2635, #13355, .T. ) ;
#19346 = LINE ( 'NONE', #3492, #4506 ) ;
#19347 = ADVANCED_FACE ( 'NONE', ( #6198 ), #15788, .T. ) ;
#19348 = CARTESIAN_POINT ( 'NONE',  ( 142.2287565553230309, -1.999999999999978018, -12.16987298107780369 ) ) ;
#19349 = ORIENTED_EDGE ( 'NONE', *, *, #22109, .F. ) ;
#19350 = DIRECTION ( 'NONE',  ( -0.9510565162951536422, -2.566386769018988816E-16, -0.3090169943749472292 ) ) ;
#19351 = DIRECTION ( 'NONE',  ( 1.000000000000000000, 2.698458740408365879E-16, -1.110223024625156540E-16 ) ) ;
#19352 = FACE_OUTER_BOUND ( 'NONE', #16056, .T. ) ;
#19353 = CARTESIAN_POINT ( 'NONE',  ( 142.0152310637605524, -4.999999999999978684, 1.702185954127501066 ) ) ;
#19354 = CARTESIAN_POINT ( 'NONE',  ( 12.01798642417223739, 9.362192935812041483, -16.69549318315592856 ) ) ;
#19355 = LINE ( 'NONE', #19205, #10667 ) ;
#19356 = CARTESIAN_POINT ( 'NONE',  ( 32.73840480032550460, -11.71477781474665925, -16.63156947497440541 ) ) ;
#19357 = ORIENTED_EDGE ( 'NONE', *, *, #18264, .T. ) ;
#19358 = CARTESIAN_POINT ( 'NONE',  ( 13.51537010444165254, 7.685947621549766851, -15.59967102646339043 ) ) ;
#19359 = CARTESIAN_POINT ( 'NONE',  ( 169.5152310637604955, -9.999999999999996447, -19.94844914048349693 ) ) ;
#19360 = VECTOR ( 'NONE', #8328, 1000.000000000000000 ) ;
#19361 = CARTESIAN_POINT ( 'NONE',  ( 21.57856661146780652, -4.666631351218505586, -18.28211233923166645 ) ) ;
#19362 = CARTESIAN_POINT ( 'NONE',  ( 12.83173194157631514, 9.543008920787411142, -16.14125448247791184 ) ) ;
#19363 = DIRECTION ( 'NONE',  ( -2.698458740408365879E-16, 1.000000000000000000, 0.000000000000000000 ) ) ;
#19364 = ORIENTED_EDGE ( 'NONE', *, *, #5212, .F. ) ;
#19365 = EDGE_CURVE ( 'NONE', #461, #4135, #25116, .T. ) ;
#19366 = EDGE_LOOP ( 'NONE', ( #25289, #22310, #27622, #2616 ) ) ;
#19367 = VECTOR ( 'NONE', #13926, 1000.000000000000000 ) ;
#19368 = CARTESIAN_POINT ( 'NONE',  ( 11.48043977940431226, 9.236673419044803879, -15.85762597608872326 ) ) ;
#19369 = DIRECTION ( 'NONE',  ( 0.000000000000000000, 0.000000000000000000, 1.000000000000000000 ) ) ;
#19370 = CARTESIAN_POINT ( 'NONE',  ( 9.936961226781097167, 16.31318409042999917, -16.49606719383117337 ) ) ;
#19371 = DIRECTION ( 'NONE',  ( -0.5877852522924731371, -1.586114251531760728E-16, -0.8090169943749474513 ) ) ;
#19372 = ORIENTED_EDGE ( 'NONE', *, *, #10935, .T. ) ;
#19373 = DIRECTION ( 'NONE',  ( -1.000000000000000000, -2.891205793294689173E-16, 0.000000000000000000 ) ) ;
#19374 = EDGE_LOOP ( 'NONE', ( #14690, #9116, #14084, #7590 ) ) ;
#19375 = CARTESIAN_POINT ( 'NONE',  ( 12.05017172662707381, 9.228765020691243492, -16.68110209197688221 ) ) ;
#19376 = ORIENTED_EDGE ( 'NONE', *, *, #17853, .F. ) ;
#19377 = CARTESIAN_POINT ( 'NONE',  ( 36.54859390953724585, -23.18451583373416014, -17.64281456791166391 ) ) ;
#19378 = CARTESIAN_POINT ( 'NONE',  ( 25.24878800877705487, -9.370948223588685622, -14.18615728435988288 ) ) ;
#19379 = CARTESIAN_POINT ( 'NONE',  ( 29.76939623719675510, -8.219725197086590995, -17.35520659559267287 ) ) ;
#19380 = ORIENTED_EDGE ( 'NONE', *, *, #230, .F. ) ;
#19381 = CARTESIAN_POINT ( 'NONE',  ( 7.261140001955372014, -5.000000000000015987, 22.34749104514272844 ) ) ;
#19382 = VERTEX_POINT ( 'NONE', #3609 ) ;
#19383 = EDGE_CURVE ( 'NONE', #7231, #21422, #10912, .T. ) ;
#19384 = CARTESIAN_POINT ( 'NONE',  ( 34.38415957124060895, -12.46085888452578594, -19.93570721963346060 ) ) ;
#19385 = CARTESIAN_POINT ( 'NONE',  ( 21.44849557978440657, 3.047722651366359781, -15.04725200041975341 ) ) ;
#19386 = CARTESIAN_POINT ( 'NONE',  ( 15.22033579473957410, 7.355362781181614018, -19.64495939069069763 ) ) ;
#19387 = CIRCLE ( 'NONE', #10123, 8.000000000000000000 ) ;
#19388 = CARTESIAN_POINT ( 'NONE',  ( 136.1922820468854241, -10.00000000000000533, -19.40354224447947473 ) ) ;
#19389 = DIRECTION ( 'NONE',  ( -1.000000000000000000, 0.000000000000000000, 0.000000000000000000 ) ) ;
#19390 = VECTOR ( 'NONE', #18487, 1000.000000000000000 ) ;
#19391 = DIRECTION ( 'NONE',  ( -0.7071067811865492381, 1.062217613570962316E-16, -0.7071067811865457964 ) ) ;
#19392 = CARTESIAN_POINT ( 'NONE',  ( 139.5152310637605524, -1.999999999999979128, -4.391296821672111328 ) ) ;
#19393 = DIRECTION ( 'NONE',  ( -1.110223024625156540E-16, 0.000000000000000000, -1.000000000000000000 ) ) ;
#19394 = DIRECTION ( 'NONE',  ( 1.000000000000000000, 0.000000000000000000, 0.000000000000000000 ) ) ;
#19395 = CARTESIAN_POINT ( 'NONE',  ( 12.27693042220145969, 9.494543488390625896, -15.31068133337694803 ) ) ;
#19396 = CARTESIAN_POINT ( 'NONE',  ( 105.4221331823114127, -4.999999999999988454, -76.59366314999438430 ) ) ;
#19397 = EDGE_CURVE ( 'NONE', #19635, #20619, #22377, .T. ) ;
#19398 = ORIENTED_EDGE ( 'NONE', *, *, #16238, .F. ) ;
#19399 = LINE ( 'NONE', #17264, #5218 ) ;
#19400 = ORIENTED_EDGE ( 'NONE', *, *, #18688, .F. ) ;
#19401 = CARTESIAN_POINT ( 'NONE',  ( 12.50268541164654756, 8.571888915454989544, -15.12803469218787811 ) ) ;
#19402 = EDGE_CURVE ( 'NONE', #12094, #20051, #29132, .T. ) ;
#19403 = ORIENTED_EDGE ( 'NONE', *, *, #9301, .F. ) ;
#19404 = CARTESIAN_POINT ( 'NONE',  ( 16.22630451241072436, 4.170241327582352220, -17.06284370071109535 ) ) ;
#19405 = LINE ( 'NONE', #12087, #6380 ) ;
#19406 = CARTESIAN_POINT ( 'NONE',  ( 148.6922820468853672, -1.999999999999977129, 2.247092850131519715 ) ) ;
#19407 = DIRECTION ( 'NONE',  ( 0.5877852522924731371, 0.000000000000000000, 0.8090169943749474513 ) ) ;
#19408 = ORIENTED_EDGE ( 'NONE', *, *, #12759, .F. ) ;
#19409 = LINE ( 'NONE', #26766, #27152 ) ;
#19410 = ORIENTED_EDGE ( 'NONE', *, *, #10485, .F. ) ;
#19411 = CARTESIAN_POINT ( 'NONE',  ( 12.79981923948071554, 9.689364640521217709, -16.15445150739013158 ) ) ;
#19412 = VERTEX_POINT ( 'NONE', #26987 ) ;
#19413 = AXIS2_PLACEMENT_3D ( 'NONE', #15400, #24733, #20135 ) ;
#19414 = CARTESIAN_POINT ( 'NONE',  ( 34.49426285277334614, -12.00696374527110066, -18.89673795385250799 ) ) ;
#19415 = CARTESIAN_POINT ( 'NONE',  ( 21.41025690189560748, 5.821651141963339882, -16.00656683556521998 ) ) ;
#19416 = VERTEX_POINT ( 'NONE', #6352 ) ;
#19417 = DIRECTION ( 'NONE',  ( 0.5877852522924731371, 1.586114251531760728E-16, 0.8090169943749474513 ) ) ;
#19418 = CARTESIAN_POINT ( 'NONE',  ( 28.90796184913828171, -12.27476343136570414, -11.88515153054143347 ) ) ;
#19419 = VERTEX_POINT ( 'NONE', #29760 ) ;
#19420 = CIRCLE ( 'NONE', #29202, 9.000000000000001776 ) ;
#19421 = LINE ( 'NONE', #5397, #27169 ) ;
#19422 =( NAMED_UNIT ( * ) PLANE_ANGLE_UNIT ( ) SI_UNIT ( $, .RADIAN. ) );
#19423 = CARTESIAN_POINT ( 'NONE',  ( 19.47299019774181161, -1.479546722229555744, -17.51644493673600067 ) ) ;
#19424 = CARTESIAN_POINT ( 'NONE',  ( 19.07048665705943336, 2.338351316274200453, -13.70053041002553407 ) ) ;
#19425 = DIRECTION ( 'NONE',  ( -2.698458740408365879E-16, 1.000000000000000000, 0.000000000000000000 ) ) ;
#19426 = ORIENTED_EDGE ( 'NONE', *, *, #26828, .F. ) ;
#19427 = CARTESIAN_POINT ( 'NONE',  ( 63.44486372867152824, 109.8897274573438096, -15.00000000000000000 ) ) ;
#19428 = CARTESIAN_POINT ( 'NONE',  ( 94.75885269270503386, -4.999999999999992006, -68.84633638624551111 ) ) ;
#19429 = CARTESIAN_POINT ( 'NONE',  ( 147.0152310637606092, -1.999999999999976241, -32.93883019725009120 ) ) ;
#19430 = AXIS2_PLACEMENT_3D ( 'NONE', #22560, #11094, #3938 ) ;
#19431 = DIRECTION ( 'NONE',  ( -2.698458740408365879E-16, 1.000000000000000000, 0.000000000000000000 ) ) ;
#19432 = DIRECTION ( 'NONE',  ( -1.000000000000000000, -4.440892098500622217E-16, -0.000000000000000000 ) ) ;
#19433 = CARTESIAN_POINT ( 'NONE',  ( 11.45256130090833935, 9.362448956408465861, -15.86931324879919991 ) ) ;
#19434 = AXIS2_PLACEMENT_3D ( 'NONE', #4717, #14006, #3052 ) ;
#19435 = CARTESIAN_POINT ( 'NONE',  ( 29.40876261992080032, -8.787110225502646088, -16.42709622331022956 ) ) ;
#19436 = CARTESIAN_POINT ( 'NONE',  ( 26.00956027078203192, -8.595392566010074731, -19.46287731774799212 ) ) ;
#19437 = EDGE_CURVE ( 'NONE', #8011, #4895, #4207, .T. ) ;
#19439 = ORIENTED_EDGE ( 'NONE', *, *, #6301, .F. ) ;
#19438 = CARTESIAN_POINT ( 'NONE',  ( 35.51409509342218485, -23.02953092745895347, -19.29936871477319826 ) ) ;
#19440 = VECTOR ( 'NONE', #26937, 1000.000000000000000 ) ;
#19441 = DIRECTION ( 'NONE',  ( 1.000000000000000000, 0.000000000000000000, 0.000000000000000000 ) ) ;
#19442 = CARTESIAN_POINT ( 'NONE',  ( 164.5152310637605240, -1.999999999999971356, -28.60870317832789667 ) ) ;
#19443 = CARTESIAN_POINT ( 'NONE',  ( -2.000000000000008882, 3.464101615137750390, 0.000000000000000000 ) ) ;
#19444 = CARTESIAN_POINT ( 'NONE',  ( 148.6922820468854241, -1.999999999999976685, -17.92658477444275889 ) ) ;
#19445 = ADVANCED_FACE ( 'NONE', ( #13503 ), #10459, .T. ) ;
#19446 = CARTESIAN_POINT ( 'NONE',  ( 148.6922820468854525, -1.999999999999976241, -26.58683881228715862 ) ) ;
#19447 = CARTESIAN_POINT ( 'NONE',  ( 143.6922820468854525, -1.999999999999977573, -23.73366926340167282 ) ) ;
#19448 = EDGE_CURVE ( 'NONE', #30101, #2137, #17631, .T. ) ;
#19449 = CARTESIAN_POINT ( 'NONE',  ( 16.06572049258021195, 3.735912457719189117, -15.00855390560170477 ) ) ;
#19450 = ORIENTED_EDGE ( 'NONE', *, *, #16372, .F. ) ;
#19451 = DIRECTION ( 'NONE',  ( -0.8090169943749474513, -2.183098979609982436E-16, -0.5877852522924731371 ) ) ;
#19452 = CARTESIAN_POINT ( 'NONE',  ( 12.25826188308600351, 9.517053581970603915, -15.32321445922237224 ) ) ;
#19453 = DIRECTION ( 'NONE',  ( -0.8090169943749474513, -2.183098979609982436E-16, 0.5877852522924731371 ) ) ;
#19454 = CARTESIAN_POINT ( 'NONE',  ( 2.500000000000000444, 1.768423874527823347, 1.020999999999997687 ) ) ;
#19455 = CARTESIAN_POINT ( 'NONE',  ( 18.98200677837107264, -2.562081333921657933, -16.63161468174866187 ) ) ;
#19456 = CARTESIAN_POINT ( 'NONE',  ( 18.53087132295907935, 5.398958961476600038, -21.24745519132487459 ) ) ;
#19457 = EDGE_LOOP ( 'NONE', ( #2801, #25927, #5627, #9504 ) ) ;
#19458 = CARTESIAN_POINT ( 'NONE',  ( 32.48283477683061449, -11.02614750807341260, -17.91093295056291979 ) ) ;
#19459 = ORIENTED_EDGE ( 'NONE', *, *, #6300, .F. ) ;
#19460 = VECTOR ( 'NONE', #12521, 1000.000000000000000 ) ;
#19461 = CARTESIAN_POINT ( 'NONE',  ( 26.37963984661160310, -4.639223599391875119, -13.30093322687953616 ) ) ;
#19462 = CARTESIAN_POINT ( 'NONE',  ( 22.33718609693395862, 3.185771058179875492, -16.53122240148476152 ) ) ;
#19463 = TOROIDAL_SURFACE ( 'NONE', #11179, 7.000000000000000888, 2.000000000000000000 ) ;
#19464 = ORIENTED_EDGE ( 'NONE', *, *, #18000, .T. ) ;
#19465 = CARTESIAN_POINT ( 'NONE',  ( 22.16846437878366061, -4.107540447007581363, -19.06500358040360865 ) ) ;
#19466 = DIRECTION ( 'NONE',  ( 1.000000000000000000, 0.000000000000000000, 0.000000000000000000 ) ) ;
#19467 = ORIENTED_EDGE ( 'NONE', *, *, #27731, .F. ) ;
#19469 = EDGE_LOOP ( 'NONE', ( #15733, #10516, #10668 ) ) ;
#19468 = DIRECTION ( 'NONE',  ( 0.9510565162951536422, 0.000000000000000000, -0.3090169943749475623 ) ) ;
#19470 = DIRECTION ( 'NONE',  ( -0.8660254037844348218, 0.5000000000000065503, -0.000000000000000000 ) ) ;
#19471 = CARTESIAN_POINT ( 'NONE',  ( 131.1922820468854241, -1.999999999999982236, -4.936203717676158398 ) ) ;
#19472 = CARTESIAN_POINT ( 'NONE',  ( 14.73435313093308174, 9.569269045654692718, -13.91804818168885305 ) ) ;
#19473 = CARTESIAN_POINT ( 'NONE',  ( 35.06179249480944549, -15.50510465796065596, -20.14053939611612520 ) ) ;
#19474 = VECTOR ( 'NONE', #25315, 1000.000000000000000 ) ;
#19475 = CARTESIAN_POINT ( 'NONE',  ( 9.893572868141015775, 16.51216863388285461, -16.51808063826580408 ) ) ;
#19476 = EDGE_CURVE ( 'NONE', #13972, #21176, #17482, .T. ) ;
#19477 = LINE ( 'NONE', #717, #14662 ) ;
#19478 = CARTESIAN_POINT ( 'NONE',  ( 139.5152310637606092, -10.00000000000000533, -28.60870317832789311 ) ) ;
#19479 = EDGE_CURVE ( 'NONE', #18472, #12418, #8475, .T. ) ;
#19480 = EDGE_CURVE ( 'NONE', #14, #25907, #10616, .T. ) ;
#19482 = CARTESIAN_POINT ( 'NONE',  ( 12.02761088988360783, 9.318053909225662679, -16.69151312802368636 ) ) ;
#19481 = VECTOR ( 'NONE', #17779, 1000.000000000000000 ) ;
#19483 = CARTESIAN_POINT ( 'NONE',  ( 163.6922820468852819, -9.999999999999998224, -0.6060766987539614181 ) ) ;
#19484 = EDGE_CURVE ( 'NONE', #28345, #22694, #15184, .T. ) ;
#19485 = DIRECTION ( 'NONE',  ( 0.000000000000000000, 0.000000000000000000, -1.000000000000000000 ) ) ;
#19486 = ORIENTED_EDGE ( 'NONE', *, *, #27860, .T. ) ;
#19487 = DIRECTION ( 'NONE',  ( 0.000000000000000000, 0.000000000000000000, 1.000000000000000000 ) ) ;
#19488 = CARTESIAN_POINT ( 'NONE',  ( 137.0152310637605808, -1.999999999999979572, -8.721423840594312082 ) ) ;
#19489 = DIRECTION ( 'NONE',  ( -0.9510565162951536422, -2.566386769018988323E-16, 0.3090169943749475623 ) ) ;
#19490 = VERTEX_POINT ( 'NONE', #2383 ) ;
#19491 = VERTEX_POINT ( 'NONE', #25874 ) ;
#19492 = VERTEX_POINT ( 'NONE', #20664 ) ;
#19493 = CARTESIAN_POINT ( 'NONE',  ( 11.15915788317279578, 9.388133443793682531, -17.26837529997955301 ) ) ;
#19494 = CARTESIAN_POINT ( 'NONE',  ( 15.74206018803408469, 8.560804325426111916, -21.16119476544194100 ) ) ;
#19495 = CARTESIAN_POINT ( 'NONE',  ( 24.59961324288297391, 0.2024632608770970121, -16.27125138369466484 ) ) ;
#19496 = CARTESIAN_POINT ( 'NONE',  ( 100.3929811530477423, -4.999999999999990230, 72.93977032092985269 ) ) ;
#19497 = DIRECTION ( 'NONE',  ( -2.698458740408365879E-16, 1.000000000000000000, 0.000000000000000000 ) ) ;
#19499 = CARTESIAN_POINT ( 'NONE',  ( 177.2287565553229172, -9.999999999999994671, -29.49038105676660493 ) ) ;
#19498 = PRODUCT_DEFINITION_FORMATION_WITH_SPECIFIED_SOURCE ( 'ANY', '', #28886, .NOT_KNOWN. ) ;
#19500 = AXIS2_PLACEMENT_3D ( 'NONE', #454, #28110, #21348 ) ;
#19501 = DIRECTION ( 'NONE',  ( 0.3090169943749472292, 8.338696094057992503E-17, -0.9510565162951536422 ) ) ;
#19502 = ADVANCED_FACE ( 'NONE', ( #23121 ), #25416, .T. ) ;
#19503 = CARTESIAN_POINT ( 'NONE',  ( 143.6922820468854525, -10.00000000000000355, -26.58683881228715506 ) ) ;
#19504 = FACE_OUTER_BOUND ( 'NONE', #10801, .T. ) ;
#19505 = CARTESIAN_POINT ( 'NONE',  ( 0.000000000000000000, 0.000000000000000000, 18.00000000000000000 ) ) ;
#19506 = DIRECTION ( 'NONE',  ( -0.000000000000000000, 0.000000000000000000, 1.000000000000000000 ) ) ;
#19507 = VECTOR ( 'NONE', #886, 1000.000000000000000 ) ;
#19508 = CARTESIAN_POINT ( 'NONE',  ( 12.02609123740286101, 9.325023229212996867, -16.69214155778140096 ) ) ;
#19509 = CARTESIAN_POINT ( 'NONE',  ( 33.47764622482974062, -12.08535443106849883, -18.57070694247861553 ) ) ;
#19510 = VERTEX_POINT ( 'NONE', #18835 ) ;
#19511 = CARTESIAN_POINT ( 'NONE',  ( 10.14999423553203606, 11.42343090068832190, -16.62569685487721571 ) ) ;
#19512 = ADVANCED_FACE ( 'NONE', ( #6647 ), #20973, .T. ) ;
#19513 = CARTESIAN_POINT ( 'NONE',  ( 23.60870351872479844, -7.222488552757559077, -14.83554404960226947 ) ) ;
#19514 = ADVANCED_FACE ( 'NONE', ( #11659 ), #6952, .T. ) ;
#19515 = CARTESIAN_POINT ( 'NONE',  ( 12.83192189813640738, 9.542137755788996145, -16.14117592875819440 ) ) ;
#19516 = FACE_BOUND ( 'NONE', #20146, .T. ) ;
#19517 = ADVANCED_FACE ( 'NONE', ( #30050 ), #16552, .T. ) ;
#19518 = ORIENTED_EDGE ( 'NONE', *, *, #7017, .F. ) ;
#19519 = MECHANICAL_DESIGN_GEOMETRIC_PRESENTATION_REPRESENTATION (  '', ( #20979 ), #5883 ) ;
#19520 = VERTEX_POINT ( 'NONE', #18693 ) ;
#19521 = CARTESIAN_POINT ( 'NONE',  ( 147.0152310637605240, -4.999999999999977796, -8.721423840594312082 ) ) ;
#19522 = CARTESIAN_POINT ( 'NONE',  ( 11.47155695691762212, 9.275332456566969697, -15.86145787682774078 ) ) ;
#19523 = FACE_OUTER_BOUND ( 'NONE', #15383, .T. ) ;
#19524 = ORIENTED_EDGE ( 'NONE', *, *, #25290, .F. ) ;
#19525 = FACE_OUTER_BOUND ( 'NONE', #19975, .T. ) ;
#19526 = EDGE_LOOP ( 'NONE', ( #23517, #11490, #18848, #21935 ) ) ;
#19527 = CARTESIAN_POINT ( 'NONE',  ( 11.86602117609799301, 10.05912493454434120, -16.75833615892761586 ) ) ;
#19528 = ORIENTED_EDGE ( 'NONE', *, *, #106, .F. ) ;
#19529 = CARTESIAN_POINT ( 'NONE',  ( 22.66942224714451370, 5.529188492372526298, -17.57712505567429773 ) ) ;
#19530 = CARTESIAN_POINT ( 'NONE',  ( 13.25083620024415332, 6.663885870737293438, -17.30077526834593016 ) ) ;
#19531 = EDGE_LOOP ( 'NONE', ( #16018, #3059, #8356, #15389 ) ) ;
#19532 = CARTESIAN_POINT ( 'NONE',  ( 20.00000000000017053, 41.64101615137744972, 12.00000000000000178 ) ) ;
#19533 = ORIENTED_EDGE ( 'NONE', *, *, #16270, .F. ) ;
#19534 = CARTESIAN_POINT ( 'NONE',  ( 36.18478257229246964, -20.55010421171508028, -20.40673782175607442 ) ) ;
#19535 = AXIS2_PLACEMENT_3D ( 'NONE', #15499, #6656, #10779 ) ;
#19536 = SHAPE_DEFINITION_REPRESENTATION ( #4251, #17708 ) ;
#19537 = VERTEX_POINT ( 'NONE', #23270 ) ;
#19538 = CARTESIAN_POINT ( 'NONE',  ( 19.19659130220728116, 4.347481709847851761, -15.16398724834160916 ) ) ;
#19539 = AXIS2_PLACEMENT_3D ( 'NONE', #22468, #10997, #12994 ) ;
#19540 = CARTESIAN_POINT ( 'NONE',  ( 21.66440995182641416, 5.535554982823286174, -17.57621636221614025 ) ) ;
#19541 = DIRECTION ( 'NONE',  ( 0.000000000000000000, 0.000000000000000000, 1.000000000000000000 ) ) ;
#19542 = EDGE_CURVE ( 'NONE', #5490, #29328, #13941, .T. ) ;
#19543 = DIRECTION ( 'NONE',  ( 2.698458740408365879E-16, -1.000000000000000000, 0.000000000000000000 ) ) ;
#19544 = CARTESIAN_POINT ( 'NONE',  ( 129.5152310637605524, -1.999999999999982236, -30.37205893520530964 ) ) ;
#19545 = DIRECTION ( 'NONE',  ( -2.698458740408365879E-16, 1.000000000000000000, 0.000000000000000000 ) ) ;
#19546 = CARTESIAN_POINT ( 'NONE',  ( 162.0152310637605240, -9.999999999999998224, -24.27857615940569502 ) ) ;
#19547 = PLANE ( 'NONE',  #21199 ) ;
#19548 = CARTESIAN_POINT ( 'NONE',  ( 11.23952829215726901, 14.25220214615140257, -15.73968358775164056 ) ) ;
#19549 = ADVANCED_FACE ( 'NONE', ( #7094 ), #28039, .T. ) ;
#19551 = VECTOR ( 'NONE', #25562, 1000.000000000000000 ) ;
#19550 = LINE ( 'NONE', #24293, #13374 ) ;
#19552 = FACE_OUTER_BOUND ( 'NONE', #29129, .T. ) ;
#19553 = ORIENTED_EDGE ( 'NONE', *, *, #29567, .T. ) ;
#19554 = VECTOR ( 'NONE', #21451, 1000.000000000000000 ) ;
#19555 = CARTESIAN_POINT ( 'NONE',  ( 12.55500454421123457, 8.595009676161804890, -15.08633542003848049 ) ) ;
#19556 = CARTESIAN_POINT ( 'NONE',  ( 10.67622114788023246, 9.011142735252827052, -16.40800301137445416 ) ) ;
#19557 = PLANE ( 'NONE',  #1507 ) ;
#19558 = LINE ( 'NONE', #28926, #18868 ) ;
#19559 = CARTESIAN_POINT ( 'NONE',  ( 162.2287565553228887, -10.00000000000000000, -3.509618943233403510 ) ) ;
#19560 = ORIENTED_EDGE ( 'NONE', *, *, #20735, .T. ) ;
#19561 = CARTESIAN_POINT ( 'NONE',  ( 2.500000000000000444, -2.357898499370430834, 3.469446951953614189E-15 ) ) ;
#19562 = VERTEX_POINT ( 'NONE', #13656 ) ;
#19563 = CARTESIAN_POINT ( 'NONE',  ( 12.83296646064745339, 9.537815246119466295, -16.14070827264395547 ) ) ;
#19564 = CARTESIAN_POINT ( 'NONE',  ( 32.48803055552120611, -10.90163289162770432, -13.69202896798154256 ) ) ;
#19565 = CARTESIAN_POINT ( 'NONE',  ( 19.51440197245297270, 8.071880087464508691, -17.28625796899888201 ) ) ;
#19566 = VERTEX_POINT ( 'NONE', #2083 ) ;
#19567 = PRODUCT_DEFINITION_SHAPE ( 'NONE', 'NONE',  #27455 ) ;
#19568 = LINE ( 'NONE', #29398, #10614 ) ;
#19569 = CARTESIAN_POINT ( 'NONE',  ( 26.40146419187390947, -13.39824708621661919, -13.49681364666919059 ) ) ;
#19570 = DIRECTION ( 'NONE',  ( -0.8090169943749474513, -2.183098979609982436E-16, 0.5877852522924731371 ) ) ;
#19571 = CARTESIAN_POINT ( 'NONE',  ( 152.0152310637604671, -1.999999999999976241, -17.38167787843870826 ) ) ;
#19572 = VERTEX_POINT ( 'NONE', #11502 ) ;
#19573 = FILL_AREA_STYLE_COLOUR ( '', #22960 ) ;
#19574 = CARTESIAN_POINT ( 'NONE',  ( 20.59283418570449697, -4.290598171560842111, -16.90930062131523215 ) ) ;
#19575 = CARTESIAN_POINT ( 'NONE',  ( 18.89276694006714052, 5.271756288042509730, -14.92826338805148190 ) ) ;
#19576 = ORIENTED_EDGE ( 'NONE', *, *, #24665, .F. ) ;
#19577 = ORIENTED_EDGE ( 'NONE', *, *, #3746, .F. ) ;
#19578 = EDGE_CURVE ( 'NONE', #8151, #20829, #20815, .T. ) ;
#19579 = LINE ( 'NONE', #25226, #12769 ) ;
#19580 = DIRECTION ( 'NONE',  ( -0.5877852522924731371, -1.586114251531760235E-16, 0.8090169943749474513 ) ) ;
#19581 = PLANE ( 'NONE',  #8615 ) ;
#19582 = FACE_OUTER_BOUND ( 'NONE', #21854, .T. ) ;
#19583 = DIRECTION ( 'NONE',  ( -2.698458740408365879E-16, 1.000000000000000000, 0.000000000000000000 ) ) ;
#19584 = CARTESIAN_POINT ( 'NONE',  ( 11.47511325496290624, 9.259230714725578792, -15.85997136665693041 ) ) ;
#19585 = CARTESIAN_POINT ( 'NONE',  ( 27.32111546295355708, -6.651148440249742499, -13.76656720552121982 ) ) ;
#19586 = CARTESIAN_POINT ( 'NONE',  ( 25.46127020808262387, -4.208148299910691392, -19.59612275642668777 ) ) ;
#19587 = ORIENTED_EDGE ( 'NONE', *, *, #11041, .T. ) ;
#19588 = LINE ( 'NONE', #10426, #6161 ) ;
#19589 = CARTESIAN_POINT ( 'NONE',  ( 24.55500000000002103, 0.000000000000000000, 0.000000000000000000 ) ) ;
#19590 = LINE ( 'NONE', #24487, #25316 ) ;
#19591 = DIRECTION ( 'NONE',  ( 0.000000000000000000, 0.000000000000000000, -1.000000000000000000 ) ) ;
#19592 = VECTOR ( 'NONE', #28408, 1000.000000000000000 ) ;
#19593 = LINE ( 'NONE', #21441, #29812 ) ;
#19594 = FACE_OUTER_BOUND ( 'NONE', #19979, .T. ) ;
#19595 = CARTESIAN_POINT ( 'NONE',  ( 21.48529164538665981, 5.106035544247377267, -18.65531623833433628 ) ) ;
#19596 = ORIENTED_EDGE ( 'NONE', *, *, #12444, .T. ) ;
#19597 = CARTESIAN_POINT ( 'NONE',  ( 172.7287565553229456, -4.999999999999970690, -36.50000000000000711 ) ) ;
#19598 = CARTESIAN_POINT ( 'NONE',  ( 12.27441163154304071, 9.506095234784829984, -15.31172292274672664 ) ) ;
#19599 = DIRECTION ( 'NONE',  ( -2.698458740408365879E-16, 1.000000000000000000, 0.000000000000000000 ) ) ;
#19600 = PLANE ( 'NONE',  #3474 ) ;
#19601 = CARTESIAN_POINT ( 'NONE',  ( 23.86551563699305234, 2.542095107771292106, -17.79649620197707094 ) ) ;
#19602 = CARTESIAN_POINT ( 'NONE',  ( 147.0152310637605240, -10.00000000000000355, 1.702185954127501066 ) ) ;
#19603 = CARTESIAN_POINT ( 'NONE',  ( 19.82966512453777952, 6.730073478465656400, -20.48479553209826065 ) ) ;
#19604 = ORIENTED_EDGE ( 'NONE', *, *, #14261, .F. ) ;
#19605 = CARTESIAN_POINT ( 'NONE',  ( 134.7287565553230024, -4.999999999999981348, -25.16025403784439973 ) ) ;
#19606 = DIRECTION ( 'NONE',  ( 0.000000000000000000, 0.000000000000000000, 1.000000000000000000 ) ) ;
#19607 = CARTESIAN_POINT ( 'NONE',  ( 25.62874891556376511, -2.832145142407604510, -18.00902499482074148 ) ) ;
#19608 = CIRCLE ( 'NONE', #20112, 2.749999999999999112 ) ;
#19609 = CARTESIAN_POINT ( 'NONE',  ( 22.91777464530744268, -8.256078323855359002, -14.14386909076557686 ) ) ;
#19610 = ORIENTED_EDGE ( 'NONE', *, *, #22492, .T. ) ;
#19611 = EDGE_CURVE ( 'NONE', #15277, #1403, #9512, .T. ) ;
#19612 = EDGE_CURVE ( 'NONE', #7334, #8969, #29514, .T. ) ;
#19613 = CARTESIAN_POINT ( 'NONE',  ( 26.36224721256908410, -8.875037662531589433, -13.49479840426202948 ) ) ;
#19614 = EDGE_CURVE ( 'NONE', #11987, #10350, #20521, .T. ) ;
#19615 = VECTOR ( 'NONE', #28344, 999.9999999999998863 ) ;
#19616 = EDGE_CURVE ( 'NONE', #25730, #1623, #25717, .T. ) ;
#19617 = CARTESIAN_POINT ( 'NONE',  ( 133.6922820468854241, -10.00000000000000711, -17.92658477444275533 ) ) ;
#19618 = ORIENTED_EDGE ( 'NONE', *, *, #6642, .T. ) ;
#19619 = LINE ( 'NONE', #3461, #16446 ) ;
#19620 = PLANE ( 'NONE',  #16785 ) ;
#19621 = DIRECTION ( 'NONE',  ( -0.000000000000000000, 0.000000000000000000, 1.000000000000000000 ) ) ;
#19622 = CARTESIAN_POINT ( 'NONE',  ( 33.78657425947636739, -10.78854458652579495, -19.16640759269550287 ) ) ;
#19623 = CARTESIAN_POINT ( 'NONE',  ( 9.936961226781097167, 16.31318409042999917, -16.49606719383117337 ) ) ;
#19624 = DIRECTION ( 'NONE',  ( -0.8090169943749474513, -2.183098979609982436E-16, 0.5877852522924731371 ) ) ;
#19625 = DIRECTION ( 'NONE',  ( 0.9510565162951536422, 2.566386769018988816E-16, 0.3090169943749472292 ) ) ;
#19626 = CARTESIAN_POINT ( 'NONE',  ( 13.12404665403065707, 8.571044468271947991, -15.91156272984762765 ) ) ;
#19627 = DIRECTION ( 'NONE',  ( 0.9510565162951536422, 0.000000000000000000, -0.3090169943749475623 ) ) ;
#19628 = DIRECTION ( 'NONE',  ( 0.9510565162951536422, 2.566386769018988816E-16, 0.3090169943749472292 ) ) ;
#19629 = VERTEX_POINT ( 'NONE', #2540 ) ;
#19630 = LINE ( 'NONE', #17343, #11494 ) ;
#19631 = DIRECTION ( 'NONE',  ( -2.698458740408365879E-16, 1.000000000000000000, 0.000000000000000000 ) ) ;
#19632 = DIRECTION ( 'NONE',  ( -2.698458740408365879E-16, 1.000000000000000000, 0.000000000000000000 ) ) ;
#19634 = ORIENTED_EDGE ( 'NONE', *, *, #12760, .F. ) ;
#19633 = AXIS2_PLACEMENT_3D ( 'NONE', #26396, #5475, #24097 ) ;
#19635 = VERTEX_POINT ( 'NONE', #11360 ) ;
#19636 = VERTEX_POINT ( 'NONE', #9211 ) ;
#19637 = CARTESIAN_POINT ( 'NONE',  ( 13.24589568141979612, 7.574869496316740225, -15.81383618087551746 ) ) ;
#19638 = VERTEX_POINT ( 'NONE', #25554 ) ;
#19639 = CARTESIAN_POINT ( 'NONE',  ( 17.25718654270123409, 10.07213275844434364, -20.48022200034118612 ) ) ;
#19640 = CARTESIAN_POINT ( 'NONE',  ( 26.35635630057183576, -13.06715036242849948, -16.03892985609963873 ) ) ;
#19641 = LINE ( 'NONE', #8045, #12095 ) ;
#19642 = DIRECTION ( 'NONE',  ( -0.000000000000000000, -0.000000000000000000, 1.000000000000000000 ) ) ;
#19643 = CARTESIAN_POINT ( 'NONE',  ( 91.90913672266484014, -4.999999999999992006, -66.77589654127525876 ) ) ;
#19644 = ADVANCED_FACE ( 'NONE', ( #21125 ), #27740, .T. ) ;
#19645 = ORIENTED_EDGE ( 'NONE', *, *, #27215, .T. ) ;
#19646 = EDGE_CURVE ( 'NONE', #16894, #11008, #27892, .T. ) ;
#19647 = CARTESIAN_POINT ( 'NONE',  ( 162.0152310637605240, -1.999999999999972244, -24.27857615940569502 ) ) ;
#19648 = ORIENTED_EDGE ( 'NONE', *, *, #27690, .F. ) ;
#19649 = DIRECTION ( 'NONE',  ( -2.698458740408365879E-16, 1.000000000000000000, 0.000000000000000000 ) ) ;
#19650 = DIRECTION ( 'NONE',  ( 6.938893903907227392E-16, -0.000000000000000000, 1.000000000000000000 ) ) ;
#19651 = ORIENTED_EDGE ( 'NONE', *, *, #9887, .F. ) ;
#19652 = DIRECTION ( 'NONE',  ( -0.9510565162951536422, -2.566386769018988816E-16, -0.3090169943749472292 ) ) ;
#19653 = DIRECTION ( 'NONE',  ( -2.698458740408365879E-16, 1.000000000000000000, 0.000000000000000000 ) ) ;
#19654 = VECTOR ( 'NONE', #11654, 1000.000000000000000 ) ;
#19655 = CARTESIAN_POINT ( 'NONE',  ( 12.02871927673971619, 9.312984558958580905, -16.69105371450780595 ) ) ;
#19656 = CARTESIAN_POINT ( 'NONE',  ( 33.06959603162382422, -11.76507887159725030, -17.56762491042838903 ) ) ;
#19657 = ORIENTED_EDGE ( 'NONE', *, *, #20203, .F. ) ;
#19658 = CARTESIAN_POINT ( 'NONE',  ( 8.945111769380243771, 16.94917547725161810, -17.84906893764549451 ) ) ;
#19659 = CARTESIAN_POINT ( 'NONE',  ( 25.21413058671614849, -1.115224416820481457, -18.44856734933592080 ) ) ;
#19660 = CARTESIAN_POINT ( 'NONE',  ( 12.82413367917259706, 9.577855520724041227, -16.14439663126654523 ) ) ;
#19661 = FACE_BOUND ( 'NONE', #12205, .T. ) ;
#19662 = ORIENTED_EDGE ( 'NONE', *, *, #8869, .T. ) ;
#19663 = LINE ( 'NONE', #621, #28712 ) ;
#19664 = ORIENTED_EDGE ( 'NONE', *, *, #5082, .T. ) ;
#19665 = CARTESIAN_POINT ( 'NONE',  ( 12.49428694376680049, 8.568214790255201052, -15.13472557389765072 ) ) ;
#19666 = CARTESIAN_POINT ( 'NONE',  ( 142.0152310637605808, -1.999999999999978018, -26.04193191628310800 ) ) ;
#19667 = ORIENTED_EDGE ( 'NONE', *, *, #483, .T. ) ;
#19668 = VERTEX_POINT ( 'NONE', #26178 ) ;
#19669 = DIRECTION ( 'NONE',  ( 0.5877852522924731371, 0.000000000000000000, 0.8090169943749474513 ) ) ;
#19670 = EDGE_LOOP ( 'NONE', ( #12039, #30221, #16106, #29028 ) ) ;
#19671 = CARTESIAN_POINT ( 'NONE',  ( 12.02001262747988797, 9.352900509162292764, -16.69465527681230199 ) ) ;
#19672 = VERTEX_POINT ( 'NONE', #3286 ) ;
#19673 = CARTESIAN_POINT ( 'NONE',  ( 13.51959648670337444, 7.024181567627514333, -18.72314150793285492 ) ) ;
#19674 = CARTESIAN_POINT ( 'NONE',  ( 28.47856004806874353, -11.16640101040803401, -12.66155532224275149 ) ) ;
#19675 = ORIENTED_EDGE ( 'NONE', *, *, #18075, .F. ) ;
#19676 = DIRECTION ( 'NONE',  ( -0.9510565162951536422, -2.566386769018988323E-16, 0.3090169943749475623 ) ) ;
#19677 = CIRCLE ( 'NONE', #2641, 4.250000000000003553 ) ;
#19678 = EDGE_LOOP ( 'NONE', ( #23472, #7926, #4242, #30066 ) ) ;
#19679 = CARTESIAN_POINT ( 'NONE',  ( 36.07559364978101968, -20.05957622185551870, -20.44697815928661200 ) ) ;
#19680 = CONTEXT_DEPENDENT_SHAPE_REPRESENTATION ( #2504, #19810 ) ;
#19681 = CARTESIAN_POINT ( 'NONE',  ( 18.53362878050275597, 1.800236982614616510, -15.18126852959267481 ) ) ;
#19682 = CARTESIAN_POINT ( 'NONE',  ( 21.04385110482095200, 5.766204710259658306, -15.30406332615466347 ) ) ;
#19683 = ADVANCED_FACE ( 'NONE', ( #12266 ), #14842, .F. ) ;
#19684 = ADVANCED_FACE ( 'NONE', ( #2831 ), #9971, .T. ) ;
#19685 = B_SPLINE_CURVE_WITH_KNOTS ( 'NONE', 3,
 ( #26959, #15006, #5572, #14706, #14850, #24635, #24194, #12571 ),
 .UNSPECIFIED., .F., .F.,
 ( 4, 2, 2, 4 ),
 ( 0.004673709593152193878, 0.005837709341827673759, 0.007001709090503152773, 0.009329708587854109933 ),
 .UNSPECIFIED. ) ;
#19686 = EDGE_CURVE ( 'NONE', #11956, #6838, #21728, .T. ) ;
#19687 = FACE_OUTER_BOUND ( 'NONE', #27460, .T. ) ;
#19688 = ADVANCED_FACE ( 'NONE', ( #7988 ), #21433, .F. ) ;
#19689 = FACE_BOUND ( 'NONE', #26765, .T. ) ;
#19690 = DIRECTION ( 'NONE',  ( 0.000000000000000000, 0.000000000000000000, -1.000000000000000000 ) ) ;
#19691 = CARTESIAN_POINT ( 'NONE',  ( 139.5152310637606092, -10.00000000000000533, -11.28819510263909542 ) ) ;
#19692 = DIRECTION ( 'NONE',  ( 0.5877852522924731371, 1.586114251531760728E-16, -0.8090169943749474513 ) ) ;
#19693 = ORIENTED_EDGE ( 'NONE', *, *, #7017, .T. ) ;
#19694 = LINE ( 'NONE', #17405, #6598 ) ;
#19695 = VECTOR ( 'NONE', #23611, 1000.000000000000000 ) ;
#19696 = CARTESIAN_POINT ( 'NONE',  ( 12.25660130062383146, 9.517454774955181662, -15.32445140518387028 ) ) ;
#19697 = FACE_OUTER_BOUND ( 'NONE', #6284, .T. ) ;
#19698 = ORIENTED_EDGE ( 'NONE', *, *, #24948, .T. ) ;
#19699 = DIRECTION ( 'NONE',  ( -1.000000000000000000, 0.000000000000000000, 0.000000000000000000 ) ) ;
#19700 = EDGE_LOOP ( 'NONE', ( #24575, #26955, #24281, #27052 ) ) ;
#19701 = CARTESIAN_POINT ( 'NONE',  ( 11.55687758731922798, 9.016417257711555777, -15.81607864292198329 ) ) ;
#19702 = ORIENTED_EDGE ( 'NONE', *, *, #16918, .F. ) ;
#19703 = CARTESIAN_POINT ( 'NONE',  ( 10.66838568802538845, 9.046021620013140918, -16.41132375377494057 ) ) ;
#19704 = CARTESIAN_POINT ( 'NONE',  ( 20.00000000000017053, 34.64101615137744972, 10.00000000000000178 ) ) ;
#19705 = CARTESIAN_POINT ( 'NONE',  ( 162.0152310637604671, -1.999999999999972689, -17.38167787843871182 ) ) ;
#19706 = PLANE ( 'NONE',  #9555 ) ;
#19707 = VERTEX_POINT ( 'NONE', #23576 ) ;
#19708 = CARTESIAN_POINT ( 'NONE',  ( 12.83225436833568089, 9.540613290865683993, -16.14103841883858337 ) ) ;
#19709 = CARTESIAN_POINT ( 'NONE',  ( 34.93112910557051976, -13.91810326443952306, -19.05872143998290014 ) ) ;
#19710 = CARTESIAN_POINT ( 'NONE',  ( 14.29829396236512729, 6.476847147513518088, -18.28004444394726491 ) ) ;
#19711 = VERTEX_POINT ( 'NONE', #19285 ) ;
#19712 = CARTESIAN_POINT ( 'NONE',  ( 78.64359365793785628, -4.999999999999996447, 57.13791534766453140 ) ) ;
#19713 = CARTESIAN_POINT ( 'NONE',  ( 16.02150382621726976, 6.204807860950024789, -14.00014022580063155 ) ) ;
#19714 = CARTESIAN_POINT ( 'NONE',  ( 173.6922820468852819, -9.999999999999996447, -6.413161187712876909 ) ) ;
#19715 = DIRECTION ( 'NONE',  ( 0.9510565162951536422, 0.000000000000000000, -0.3090169943749475623 ) ) ;
#19716 = SURFACE_SIDE_STYLE ('',( #12254 ) ) ;
#19717 = CARTESIAN_POINT ( 'NONE',  ( 24.77705064808911217, -2.604154092221317551, -13.46095375842554098 ) ) ;
#19718 = CARTESIAN_POINT ( 'NONE',  ( 16.84217415841480303, 1.412180072802544872, -16.35713574856416841 ) ) ;
#19719 = VECTOR ( 'NONE', #1896, 1000.000000000000000 ) ;
#19720 = ORIENTED_EDGE ( 'NONE', *, *, #9092, .T. ) ;
#19721 = EDGE_CURVE ( 'NONE', #19118, #27148, #23734, .T. ) ;
#19723 = ORIENTED_EDGE ( 'NONE', *, *, #24318, .T. ) ;
#19722 = EDGE_CURVE ( 'NONE', #24484, #9002, #24182, .T. ) ;
#19724 = CARTESIAN_POINT ( 'NONE',  ( -3.469446951953614189E-15, -4.618802153517058251, -2.450000000000000178 ) ) ;
#19725 = DIRECTION ( 'NONE',  ( -0.5877852522924731371, -1.586114251531760235E-16, 0.8090169943749474513 ) ) ;
#19726 = VECTOR ( 'NONE', #9560, 1000.000000000000000 ) ;
#19727 = CARTESIAN_POINT ( 'NONE',  ( 13.00000000000000178, -2.870178842070716726E-15, -23.00000000000000000 ) ) ;
#19728 = PLANE ( 'NONE',  #24817 ) ;
#19729 = CARTESIAN_POINT ( 'NONE',  ( 130.7287565553229456, -4.999999999999983125, 0.5000000000000052180 ) ) ;
#19730 = ORIENTED_EDGE ( 'NONE', *, *, #29401, .T. ) ;
#19731 = CARTESIAN_POINT ( 'NONE',  ( 11.47269659055779378, 9.270105954394804115, -15.86098659800193644 ) ) ;
#19732 = CARTESIAN_POINT ( 'NONE',  ( 15.87806330829146617, 7.947701475055697351, -19.83831759000646855 ) ) ;
#19733 = CARTESIAN_POINT ( 'NONE',  ( 25.71810023473615203, -5.953606672203104466, -12.71518937071605038 ) ) ;
#19734 = EDGE_LOOP ( 'NONE', ( #27208, #5651, #24984, #12143 ) ) ;
#19735 = DIRECTION ( 'NONE',  ( 1.000000000000000000, 0.000000000000000000, 0.000000000000000000 ) ) ;
#19736 = DIRECTION ( 'NONE',  ( 0.000000000000000000, 0.000000000000000000, -1.000000000000000000 ) ) ;
#19737 = LINE ( 'NONE', #10132, #7748 ) ;
#19738 = CARTESIAN_POINT ( 'NONE',  ( 172.0152310637604955, -1.999999999999969358, -34.70218595412750773 ) ) ;
#19739 = AXIS2_PLACEMENT_3D ( 'NONE', #24291, #10386, #15261 ) ;
#19740 = CARTESIAN_POINT ( 'NONE',  ( 3.999999999999996447, 0.000000000000000000, 8.673617379884035472E-16 ) ) ;
#19741 = CARTESIAN_POINT ( 'NONE',  ( 17.72480397827495224, 1.356124466512965476, -19.40231245121514903 ) ) ;
#19742 = ORIENTED_EDGE ( 'NONE', *, *, #25415, .F. ) ;
#19743 = LINE ( 'NONE', #19597, #29600 ) ;
#19744 = CARTESIAN_POINT ( 'NONE',  ( 12.27697253541231426, 9.494350595542041304, -15.31066389949581463 ) ) ;
#19745 = EDGE_CURVE ( 'NONE', #17144, #2569, #991, .T. ) ;
#19746 = FACE_OUTER_BOUND ( 'NONE', #20472, .T. ) ;
#19747 = CARTESIAN_POINT ( 'NONE',  ( 156.1922820468853388, -1.999999999999974909, -2.083034168790677043 ) ) ;
#19748 = CARTESIAN_POINT ( 'NONE',  ( 22.51149892830068211, -1.106640851078940502, -13.23823320067571885 ) ) ;
#19749 = CARTESIAN_POINT ( 'NONE',  ( 172.2287565553229456, -1.999999999999969358, -29.49038105676660493 ) ) ;
#19750 = CARTESIAN_POINT ( 'NONE',  ( 18.68528716101036480, 3.575476808761081760, -13.14399490972872186 ) ) ;
#19751 = EDGE_LOOP ( 'NONE', ( #26687, #19758, #15380, #22583 ) ) ;
#19752 = CARTESIAN_POINT ( 'NONE',  ( 0.000000000000000000, 0.000000000000000000, -5.000000000000000888 ) ) ;
#19753 = VECTOR ( 'NONE', #19770, 1000.000000000000000 ) ;
#19754 = CARTESIAN_POINT ( 'NONE',  ( 23.14387462191455214, -5.292040767005758539, -18.71731562455695297 ) ) ;
#19755 = CARTESIAN_POINT ( 'NONE',  ( 27.03394943597420408, -2.104382873295748801, -14.19367964525161163 ) ) ;
#19756 = LINE ( 'NONE', #24511, #27361 ) ;
#19757 = VECTOR ( 'NONE', #7448, 999.9999999999998863 ) ;
#19758 = ORIENTED_EDGE ( 'NONE', *, *, #17654, .F. ) ;
#19759 = AXIS2_PLACEMENT_3D ( 'NONE', #20226, #24828, #6204 ) ;
#19760 = CARTESIAN_POINT ( 'NONE',  ( 146.4575131106459196, -9.999999999999976907, -17.99999999999998934 ) ) ;
#19761 = EDGE_LOOP ( 'NONE', ( #9084, #19898, #19795, #6839 ) ) ;
#19762 = CARTESIAN_POINT ( 'NONE',  ( 136.1922820468854241, -4.999999999999981348, -2.083034168790677043 ) ) ;
#19763 = CARTESIAN_POINT ( 'NONE',  ( 154.5152310637605240, -1.999999999999974465, -21.71180489736091346 ) ) ;
#19764 = DIRECTION ( 'NONE',  ( -0.8090169943749474513, -2.183098979609982436E-16, 0.5877852522924731371 ) ) ;
#19765 = CARTESIAN_POINT ( 'NONE',  ( 13.78676817088038931, 5.425489125369224119, -17.89072192914586168 ) ) ;
#19766 = CARTESIAN_POINT ( 'NONE',  ( 34.35798975979065517, -12.34328324435382207, -19.92780167937219815 ) ) ;
#19767 = CARTESIAN_POINT ( 'NONE',  ( 11.14863080475985591, 10.75631295387255548, -15.99499920034263489 ) ) ;
#19768 = VECTOR ( 'NONE', #5308, 1000.000000000000000 ) ;
#19769 = DIRECTION ( 'NONE',  ( -1.000000000000000000, -4.440892098500622217E-16, 0.000000000000000000 ) ) ;
#19770 = DIRECTION ( 'NONE',  ( -0.5877852522924731371, -1.586114251531760235E-16, 0.8090169943749474513 ) ) ;
#19771 = CARTESIAN_POINT ( 'NONE',  ( 16.24089679924285790, 9.948436389806387226, -13.42737814189079337 ) ) ;
#19772 = CARTESIAN_POINT ( 'NONE',  ( 131.1922820468854241, -4.999999999999982236, -30.91696583120935671 ) ) ;
#19773 = DIRECTION ( 'NONE',  ( 0.000000000000000000, 0.000000000000000000, 1.000000000000000000 ) ) ;
#19774 = EDGE_CURVE ( 'NONE', #20748, #29240, #21584, .T. ) ;
#19775 = ADVANCED_FACE ( 'NONE', ( #682, #17153 ), #17296, .F. ) ;
#19776 = EDGE_CURVE ( 'NONE', #29672, #30260, #7692, .T. ) ;
#19777 = ORIENTED_EDGE ( 'NONE', *, *, #29006, .F. ) ;
#19778 = AXIS2_PLACEMENT_3D ( 'NONE', #9074, #18245, #15659 ) ;
#19779 = DIRECTION ( 'NONE',  ( 0.000000000000000000, 0.000000000000000000, 1.000000000000000000 ) ) ;
#19780 = LINE ( 'NONE', #3625, #16119 ) ;
#19781 = EDGE_CURVE ( 'NONE', #7028, #25406, #9825, .T. ) ;
#19782 = CONICAL_SURFACE ( 'NONE', #10039, 8.000000000000007105, 1.047197551196596077 ) ;
#19783 = FACE_OUTER_BOUND ( 'NONE', #26756, .T. ) ;
#19784 = ORIENTED_EDGE ( 'NONE', *, *, #21204, .T. ) ;
#19785 = ORIENTED_EDGE ( 'NONE', *, *, #25835, .T. ) ;
#19786 = ORIENTED_EDGE ( 'NONE', *, *, #3607, .T. ) ;
#19787 = CARTESIAN_POINT ( 'NONE',  ( 8.944584698556434788, 16.95159269123564272, -17.91535980893264224 ) ) ;
#19788 = CARTESIAN_POINT ( 'NONE',  ( 12.84881458348222516, 5.748695638350556969, -17.40385974964576477 ) ) ;
#19789 = CARTESIAN_POINT ( 'NONE',  ( 24.51672896724849338, -10.45039314358892035, -14.45231470433035170 ) ) ;
#19790 = CARTESIAN_POINT ( 'NONE',  ( 153.6922820468853388, -10.00000000000000178, -15.07341522555727309 ) ) ;
#19791 = CARTESIAN_POINT ( 'NONE',  ( 132.0152310637605808, -1.999999999999981348, -6.958068083716893781 ) ) ;
#19792 = LINE ( 'NONE', #26393, #2113 ) ;
#19793 = VECTOR ( 'NONE', #4373, 1000.000000000000000 ) ;
#19794 = B_SPLINE_CURVE_WITH_KNOTS ( 'NONE', 3,
 ( #7690, #24327, #989, #17000, #678, #540, #9823, #7545 ),
 .UNSPECIFIED., .F., .F.,
 ( 4, 2, 2, 4 ),
 ( 0.004673709593152137499, 0.005837709341827637330, 0.007001709090503138028, 0.009329708587854137689 ),
 .UNSPECIFIED. ) ;
#19795 = ORIENTED_EDGE ( 'NONE', *, *, #8865, .T. ) ;
#19796 = EDGE_LOOP ( 'NONE', ( #6275, #1792, #794, #3081, #20526 ) ) ;
#19797 = PLANE ( 'NONE',  #15739 ) ;
#19798 = VERTEX_POINT ( 'NONE', #26481 ) ;
#19800 = ORIENTED_EDGE ( 'NONE', *, *, #26054, .T. ) ;
#19799 = FACE_OUTER_BOUND ( 'NONE', #23675, .T. ) ;
#19801 = VECTOR ( 'NONE', #6133, 1000.000000000000000 ) ;
#19802 = APPLICATION_CONTEXT ( 'automotive_design' ) ;
#19803 = LINE ( 'NONE', #14913, #16607 ) ;
#19805 = LINE ( 'NONE', #24255, #6053 ) ;
#19804 = CONICAL_SURFACE ( 'NONE', #18831, 8.000000000000007105, 1.047197551196596077 ) ;
#19806 = CARTESIAN_POINT ( 'NONE',  ( 13.13744203029165369, 8.576964204390579383, -15.90088637244482150 ) ) ;
#19807 = CARTESIAN_POINT ( 'NONE',  ( 33.15992091288699584, -11.77879734164826786, -17.82291275646110407 ) ) ;
#19808 = ORIENTED_EDGE ( 'NONE', *, *, #10557, .F. ) ;
#19809 = CARTESIAN_POINT ( 'NONE',  ( 9.112894736278665420, 16.17970140370183785, -17.05457397994698709 ) ) ;
#19810 = PRODUCT_DEFINITION_SHAPE ( 'NONE', 'NONE',  #30266 ) ;
#19811 = CARTESIAN_POINT ( 'NONE',  ( 25.57370974413349884, -0.4222200280313516685, -16.88676729435558599 ) ) ;
#19812 = CARTESIAN_POINT ( 'NONE',  ( 10.35866308580767026, 16.97206128008099313, -17.90676409391864610 ) ) ;
#19813 = FACE_BOUND ( 'NONE', #6182, .T. ) ;
#19814 = EDGE_CURVE ( 'NONE', #29971, #28006, #26634, .T. ) ;
#19815 = ORIENTED_EDGE ( 'NONE', *, *, #7874, .F. ) ;
#19816 = LINE ( 'NONE', #1836, #26629 ) ;
#19817 = EDGE_CURVE ( 'NONE', #14810, #30215, #3175, .T. ) ;
#19818 = VECTOR ( 'NONE', #2663, 1000.000000000000000 ) ;
#19819 = CARTESIAN_POINT ( 'NONE',  ( 12.37169234869624646, 8.529253869913038244, -15.23127513898213081 ) ) ;
#19820 = LINE ( 'NONE', #17236, #4756 ) ;
#19821 = EDGE_CURVE ( 'NONE', #25494, #27706, #2214, .T. ) ;
#19822 = ORIENTED_EDGE ( 'NONE', *, *, #14363, .F. ) ;
#19823 = DIRECTION ( 'NONE',  ( -1.110223024625156540E-16, 0.000000000000000000, -1.000000000000000000 ) ) ;
#19824 = VERTEX_POINT ( 'NONE', #832 ) ;
#19825 = CARTESIAN_POINT ( 'NONE',  ( 12.03006260835556951, 9.306948544855226046, -16.69048869075990638 ) ) ;
#19826 = ORIENTED_EDGE ( 'NONE', *, *, #3857, .F. ) ;
#19827 = AXIS2_PLACEMENT_3D ( 'NONE', #2138, #7003, #16149 ) ;
#19828 = CARTESIAN_POINT ( 'NONE',  ( 18.86526831082781541, 1.353360947173176232, -20.65364330072180366 ) ) ;
#19829 = CARTESIAN_POINT ( 'NONE',  ( 20.04052888069229610, 8.940267654624740601, -17.40200224619232117 ) ) ;
#19830 = AXIS2_PLACEMENT_3D ( 'NONE', #1043, #22084, #27149 ) ;
#19831 = DIRECTION ( 'NONE',  ( 0.9510565162951536422, 2.566386769018988816E-16, 0.3090169943749472292 ) ) ;
#19832 = EDGE_LOOP ( 'NONE', ( #17575, #1402, #14975, #20307 ) ) ;
#19833 = CARTESIAN_POINT ( 'NONE',  ( 177.2287565553229172, -9.999999999999994671, -29.49038105676660493 ) ) ;
#19834 = CARTESIAN_POINT ( 'NONE',  ( 17.29421355564066332, 9.360779442694735053, -19.18964209290773937 ) ) ;
#19835 = CARTESIAN_POINT ( 'NONE',  ( 112.8128711859804554, -4.999999999999986677, -81.96334862300538759 ) ) ;
#19836 = FACE_BOUND ( 'NONE', #29955, .T. ) ;
#19837 = VECTOR ( 'NONE', #11304, 1000.000000000000000 ) ;
#19838 = ORIENTED_EDGE ( 'NONE', *, *, #10523, .F. ) ;
#19839 = DIRECTION ( 'NONE',  ( 0.000000000000000000, 0.000000000000000000, -1.000000000000000000 ) ) ;
#19840 = LINE ( 'NONE', #29205, #16962 ) ;
#19841 = DIRECTION ( 'NONE',  ( 1.000000000000000000, 2.698458740408365879E-16, -1.110223024625156540E-16 ) ) ;
#19842 = AXIS2_PLACEMENT_3D ( 'NONE', #4558, #23036, #13846 ) ;
#19843 = CARTESIAN_POINT ( 'NONE',  ( 133.7287565553229172, -4.999999999999982236, -36.50000000000000711 ) ) ;
#19844 = CARTESIAN_POINT ( 'NONE',  ( 11.05541533671906684, 17.68942329836457361, -17.91521986731755334 ) ) ;
#19845 = CARTESIAN_POINT ( 'NONE',  ( 147.2287565553230309, -10.00000000000000178, -29.49038105676660138 ) ) ;
#19846 = ORIENTED_EDGE ( 'NONE', *, *, #23172, .T. ) ;
#19847 = SHAPE_REPRESENTATION ( 'link rod', ( #13190 ), #12225 ) ;
#19848 = DIRECTION ( 'NONE',  ( -0.9510565162951536422, -2.566386769018988323E-16, 0.3090169943749475623 ) ) ;
#19849 = ORIENTED_EDGE ( 'NONE', *, *, #10480, .T. ) ;
#19850 = CARTESIAN_POINT ( 'NONE',  ( 12.50396148805030627, 8.572452836447732594, -15.12701763676990119 ) ) ;
#19851 = ORIENTED_EDGE ( 'NONE', *, *, #15240, .F. ) ;
#19852 = EDGE_CURVE ( 'NONE', #1397, #29646, #28805, .T. ) ;
#19853 = CARTESIAN_POINT ( 'NONE',  ( 12.49426214472998176, 7.541115143590324088, -15.13238550383361769 ) ) ;
#19854 = DIRECTION ( 'NONE',  ( -0.8090169943749474513, -2.183098979609982436E-16, -0.5877852522924731371 ) ) ;
#19855 = LINE ( 'NONE', #29385, #14951 ) ;
#19856 = EDGE_CURVE ( 'NONE', #26851, #16252, #21274, .T. ) ;
#19857 = EDGE_CURVE ( 'NONE', #5097, #16128, #14834, .T. ) ;
#19858 = ORIENTED_EDGE ( 'NONE', *, *, #14606, .F. ) ;
#19859 = CARTESIAN_POINT ( 'NONE',  ( 0.000000000000000000, 0.000000000000000000, -2.450000000000000622 ) ) ;
#19860 = EDGE_CURVE ( 'NONE', #10405, #25866, #17737, .T. ) ;
#19861 = VERTEX_POINT ( 'NONE', #6007 ) ;
#19862 = CARTESIAN_POINT ( 'NONE',  ( 12.76739998655820685, 9.838043466917183011, -16.16785800888773394 ) ) ;
#19863 = CARTESIAN_POINT ( 'NONE',  ( 33.78268718695997563, -11.09826429569044670, -17.35115476112383348 ) ) ;
#19864 = CARTESIAN_POINT ( 'NONE',  ( 19.18841159021359033, -2.222386543571284179, -18.22349448661670834 ) ) ;
#19865 = ORIENTED_EDGE ( 'NONE', *, *, #12830, .T. ) ;
#19866 = AXIS2_PLACEMENT_3D ( 'NONE', #26516, #22376, #10458 ) ;
#19867 = CARTESIAN_POINT ( 'NONE',  ( 0.000000000000000000, 0.000000000000000000, -15.00000000000000000 ) ) ;
#19868 = CARTESIAN_POINT ( 'NONE',  ( 15.10175627602374249, 9.741420229655037843, -13.89989488922661742 ) ) ;
#19869 = ORIENTED_EDGE ( 'NONE', *, *, #11828, .F. ) ;
#19870 = DIRECTION ( 'NONE',  ( 1.000000000000000000, 0.000000000000000000, 0.000000000000000000 ) ) ;
#19871 = CARTESIAN_POINT ( 'NONE',  ( 19.39248696316839116, -1.610358169686434193, -16.91126230894791860 ) ) ;
#19872 = VECTOR ( 'NONE', #17137, 1000.000000000000000 ) ;
#19873 = CARTESIAN_POINT ( 'NONE',  ( 19.38139026969670553, 5.460277215109251792, -15.14974238112136540 ) ) ;
#19874 = VERTEX_POINT ( 'NONE', #8436 ) ;
#19875 = ORIENTED_EDGE ( 'NONE', *, *, #19070, .F. ) ;
#19876 = DIRECTION ( 'NONE',  ( 1.000000000000000000, 0.000000000000000000, 0.000000000000000000 ) ) ;
#19877 = AXIS2_PLACEMENT_3D ( 'NONE', #21234, #11619, #20930 ) ;
#19878 = DIRECTION ( 'NONE',  ( 0.5877852522924731371, 1.586114251531760728E-16, 0.8090169943749474513 ) ) ;
#19879 = LINE ( 'NONE', #10726, #17694 ) ;
#19880 = EDGE_CURVE ( 'NONE', #14895, #7328, #29098, .T. ) ;
#19881 = CARTESIAN_POINT ( 'NONE',  ( 142.0152310637606092, -1.999999999999978018, -24.27857615940569147 ) ) ;
#19882 = DIRECTION ( 'NONE',  ( -0.9510565162951536422, -2.566386769018988816E-16, -0.3090169943749472292 ) ) ;
#19883 = LINE ( 'NONE', #17442, #28047 ) ;
#19884 = AXIS2_PLACEMENT_3D ( 'NONE', #6321, #28281, #18629 ) ;
#19885 = CARTESIAN_POINT ( 'NONE',  ( 11.22458689634746776, 9.088074461393535586, -17.24131758186684138 ) ) ;
#19886 = CARTESIAN_POINT ( 'NONE',  ( 11.47288049726737214, 9.269262779257836371, -15.86091052746238184 ) ) ;
#19887 = CARTESIAN_POINT ( 'NONE',  ( 23.87675077653036126, -6.787291307973906562, -13.16608595595566733 ) ) ;
#19888 = ORIENTED_EDGE ( 'NONE', *, *, #18481, .F. ) ;
#19889 = FACE_OUTER_BOUND ( 'NONE', #14426, .T. ) ;
#19890 = LINE ( 'NONE', #24192, #1901 ) ;
#19891 = CARTESIAN_POINT ( 'NONE',  ( 0.8120000000000002771, 7.511012776518210972E-16, -5.000000000000000000 ) ) ;
#19892 = CARTESIAN_POINT ( 'NONE',  ( 25.00000000000001066, 60.00000000000000711, 29.99999999999998579 ) ) ;
#19893 = EDGE_CURVE ( 'NONE', #22605, #20491, #29250, .T. ) ;
#19894 = LINE ( 'NONE', #15763, #4412 ) ;
#19895 = CARTESIAN_POINT ( 'NONE',  ( 159.5152310637605524, -4.999999999999975131, -28.60870317832789667 ) ) ;
#19896 = EDGE_CURVE ( 'NONE', #6528, #11987, #5864, .T. ) ;
#19898 = ORIENTED_EDGE ( 'NONE', *, *, #16304, .T. ) ;
#19897 = CARTESIAN_POINT ( 'NONE',  ( 19.61192361542596529, -2.405681417800469291, -14.70675912396028906 ) ) ;
#19899 = VECTOR ( 'NONE', #7755, 1000.000000000000000 ) ;
#19900 = ORIENTED_EDGE ( 'NONE', *, *, #23165, .T. ) ;
#19901 = DIRECTION ( 'NONE',  ( -0.000000000000000000, -0.000000000000000000, -1.000000000000000000 ) ) ;
#19902 = ADVANCED_FACE ( 'NONE', ( #27099 ), #22660, .T. ) ;
#19903 = CARTESIAN_POINT ( 'NONE',  ( 12.27187887740847039, 9.517710768097034091, -15.31277030567625452 ) ) ;
#19904 = VECTOR ( 'NONE', #2948, 1000.000000000000000 ) ;
#19905 = CARTESIAN_POINT ( 'NONE',  ( 132.0152310637605524, -10.00000000000000711, -17.38167787843870826 ) ) ;
#19906 = CARTESIAN_POINT ( 'NONE',  ( 148.6922820468854525, -10.00000000000000178, -35.24709285013155835 ) ) ;
#19907 = EDGE_LOOP ( 'NONE', ( #17187, #5483, #18787, #26605, #17906 ) ) ;
#19908 = CARTESIAN_POINT ( 'NONE',  ( 20.39549844898813191, -2.061726703908969505, -13.85117726305786512 ) ) ;
#19909 = DIRECTION ( 'NONE',  ( 0.9510565162951536422, 0.000000000000000000, -0.3090169943749475623 ) ) ;
#19910 = CARTESIAN_POINT ( 'NONE',  ( 15.90442531705523876, 3.007083446286336947, -19.83189509879157697 ) ) ;
#19911 = EDGE_LOOP ( 'NONE', ( #9952, #10491, #6128, #12456 ) ) ;
#19912 = CARTESIAN_POINT ( 'NONE',  ( 35.54859390953724585, -22.18451583373416014, -17.64281456791166036 ) ) ;
#19913 = ORIENTED_EDGE ( 'NONE', *, *, #5848, .T. ) ;
#19914 = SURFACE_STYLE_FILL_AREA ( #24653 ) ;
#19915 = CARTESIAN_POINT ( 'NONE',  ( 28.44965076230254653, -4.228683950944192027, -16.16799691904953562 ) ) ;
#19916 = CARTESIAN_POINT ( 'NONE',  ( 18.73701609394335321, -1.228702115187185973, -15.37238819164404369 ) ) ;
#19917 = VERTEX_POINT ( 'NONE', #18042 ) ;
#19918 = DIRECTION ( 'NONE',  ( -2.698458740408365879E-16, 1.000000000000000000, 0.000000000000000000 ) ) ;
#19919 = VECTOR ( 'NONE', #24486, 1000.000000000000000 ) ;
#19920 = CARTESIAN_POINT ( 'NONE',  ( 154.7287565553230024, -4.999999999999976019, -25.16025403784439973 ) ) ;
#19921 = VERTEX_POINT ( 'NONE', #19729 ) ;
#19922 = EDGE_CURVE ( 'NONE', #18375, #438, #17289, .T. ) ;
#19923 = VECTOR ( 'NONE', #8173, 1000.000000000000000 ) ;
#19924 = DIRECTION ( 'NONE',  ( -0.9510565162951536422, -2.566386769018988816E-16, -0.3090169943749472292 ) ) ;
#19925 = DIRECTION ( 'NONE',  ( -2.698458740408365879E-16, 1.000000000000000000, 0.000000000000000000 ) ) ;
#19926 = CARTESIAN_POINT ( 'NONE',  ( -4.000000000000005329, 2.309401076758490934, -0.3572655899081616515 ) ) ;
#19927 = CARTESIAN_POINT ( 'NONE',  ( 158.6922820468853388, -1.999999999999974465, -9.266330736598359152 ) ) ;
#19928 = CARTESIAN_POINT ( 'NONE',  ( 23.59197141788265384, -6.183129490800155281, -14.78464116683282015 ) ) ;
#19929 = LINE ( 'NONE', #10775, #19481 ) ;
#19930 = CARTESIAN_POINT ( 'NONE',  ( 34.49115424338278046, -12.94152926980570939, -19.96804914223585925 ) ) ;
#19931 = DIRECTION ( 'NONE',  ( 1.000000000000000000, 2.698458740408365879E-16, -1.110223024625156540E-16 ) ) ;
#19932 = CARTESIAN_POINT ( 'NONE',  ( 9.898178882064430084, 16.49104486689975246, -16.51464960819000893 ) ) ;
#19933 = DIRECTION ( 'NONE',  ( -0.9510565162951536422, -2.566386769018988323E-16, 0.3090169943749475623 ) ) ;
#19934 = LINE ( 'NONE', #1492, #22202 ) ;
#19935 = CARTESIAN_POINT ( 'NONE',  ( 9.661883061612440926, 16.25482663361732705, -17.91664992932185996 ) ) ;
#19936 = CARTESIAN_POINT ( 'NONE',  ( 3.362531273473086113, -5.000000000000016875, 10.34880714360505038 ) ) ;
#19937 = ORIENTED_EDGE ( 'NONE', *, *, #24280, .T. ) ;
#19938 = DIRECTION ( 'NONE',  ( 0.000000000000000000, -0.000000000000000000, 1.000000000000000000 ) ) ;
#19939 = CARTESIAN_POINT ( 'NONE',  ( 11.46471852075427478, 9.306694396509932687, -15.86428581073749378 ) ) ;
#19940 = ORIENTED_EDGE ( 'NONE', *, *, #22873, .F. ) ;
#19941 = VECTOR ( 'NONE', #19692, 1000.000000000000000 ) ;
#19942 = DIRECTION ( 'NONE',  ( 0.000000000000000000, 0.000000000000000000, 1.000000000000000000 ) ) ;
#19943 = CARTESIAN_POINT ( 'NONE',  ( 5.000000000000004441, 5.204748896376250699E-16, -4.250000000000000000 ) ) ;
#19944 = LINE ( 'NONE', #1049, #26379 ) ;
#19945 = STYLED_ITEM ( 'NONE', ( #3796 ), #1479 ) ;
#19946 = ORIENTED_EDGE ( 'NONE', *, *, #13248, .T. ) ;
#19947 = CARTESIAN_POINT ( 'NONE',  ( 13.37894900189793290, 7.625660844661456217, -15.70840104182326513 ) ) ;
#19948 = CARTESIAN_POINT ( 'NONE',  ( 31.02293300316137348, -10.15460426738793664, -15.78645847904462052 ) ) ;
#19949 = ORIENTED_EDGE ( 'NONE', *, *, #15163, .F. ) ;
#19950 = CARTESIAN_POINT ( 'NONE',  ( 29.60394739741320080, -6.827861936862228198, -14.22031441372854843 ) ) ;
#19951 = CARTESIAN_POINT ( 'NONE',  ( 24.97892660363778106, -6.291154998746494087, -12.74939059104742256 ) ) ;
#19952 = PLANE ( 'NONE',  #23337 ) ;
#19953 = LINE ( 'NONE', #1355, #4802 ) ;
#19954 = DIRECTION ( 'NONE',  ( 0.000000000000000000, -0.000000000000000000, -1.000000000000000000 ) ) ;
#19955 = VERTEX_POINT ( 'NONE', #14995 ) ;
#19956 = VERTEX_POINT ( 'NONE', #10731 ) ;
#19957 = CARTESIAN_POINT ( 'NONE',  ( 0.000000000000000000, 0.000000000000000000, 2.549999999999998490 ) ) ;
#19958 = EDGE_CURVE ( 'NONE', #3010, #23457, #20182, .T. ) ;
#19959 = VECTOR ( 'NONE', #8545, 1000.000000000000000 ) ;
#19960 = DIRECTION ( 'NONE',  ( -1.000000000000000000, -1.332267629550187651E-15, 0.000000000000000000 ) ) ;
#19961 = PRODUCT_RELATED_PRODUCT_CATEGORY ( 'part', '', ( #27439 ) ) ;
#19962 = ORIENTED_EDGE ( 'NONE', *, *, #2685, .T. ) ;
#19963 = DIRECTION ( 'NONE',  ( -0.9510565162951536422, 0.000000000000000000, -0.3090169943749472292 ) ) ;
#19964 = DIRECTION ( 'NONE',  ( -1.000000000000000000, -1.332267629550187651E-15, 0.000000000000000000 ) ) ;
#19965 = AXIS2_PLACEMENT_3D ( 'NONE', #22252, #19351, #7760 ) ;
#19966 = CARTESIAN_POINT ( 'NONE',  ( 13.12174330432777047, 8.570030634161971861, -15.91339823077023929 ) ) ;
#19967 = CARTESIAN_POINT ( 'NONE',  ( 33.40448403937627830, -11.94904316976568914, -18.43672998654903239 ) ) ;
#19968 = EDGE_LOOP ( 'NONE', ( #2532, #7146, #29354, #3480, #19082 ) ) ;
#19969 = CARTESIAN_POINT ( 'NONE',  ( 9.144997394934375023, 16.03247451896970688, -17.04129840131518492 ) ) ;
#19970 = EDGE_LOOP ( 'NONE', ( #19587, #18070, #21985, #16581, #24964 ) ) ;
#19971 = CARTESIAN_POINT ( 'NONE',  ( 26.47492910780048447, -3.130564378024159211, -15.09640780237150892 ) ) ;
#19972 = CARTESIAN_POINT ( 'NONE',  ( 12.87010724449035415, 9.516853939945930208, -16.11395691550788101 ) ) ;
#19973 = FACE_BOUND ( 'NONE', #10885, .T. ) ;
#19974 = ORIENTED_EDGE ( 'NONE', *, *, #20073, .T. ) ;
#19975 = EDGE_LOOP ( 'NONE', ( #8050, #22304, #11483, #29629 ) ) ;
#19976 = CARTESIAN_POINT ( 'NONE',  ( -13.00000000000001243, 55.00000000000000711, -23.00000000000000000 ) ) ;
#19977 = CARTESIAN_POINT ( 'NONE',  ( 11.51951884677450266, 9.108496074915260365, -15.83757232928968683 ) ) ;
#19978 = CARTESIAN_POINT ( 'NONE',  ( 8.000000000000001776, 4.336808689942017736E-15, 0.000000000000000000 ) ) ;
#19979 = EDGE_LOOP ( 'NONE', ( #28697, #3332, #11896, #16670 ) ) ;
#19980 = CARTESIAN_POINT ( 'NONE',  ( 143.6922820468854525, -1.999999999999978018, -35.24709285013155835 ) ) ;
#19981 = ORIENTED_EDGE ( 'NONE', *, *, #19542, .T. ) ;
#19982 = AXIS2_PLACEMENT_3D ( 'NONE', #18185, #23527, #21379 ) ;
#19983 = CARTESIAN_POINT ( 'NONE',  ( 13.19188795686497429, 8.601024833420110483, -15.85749200792911573 ) ) ;
#19984 = ORIENTED_EDGE ( 'NONE', *, *, #13188, .F. ) ;
#19985 = VECTOR ( 'NONE', #11854, 1000.000000000000000 ) ;
#19986 = CARTESIAN_POINT ( 'NONE',  ( 15.79264427988833219, 7.655968387373099482, -13.90199225654327897 ) ) ;
#19987 = CARTESIAN_POINT ( 'NONE',  ( 22.09051738352356153, 1.573095004317974333, -13.27920415769822426 ) ) ;
#19988 = CIRCLE ( 'NONE', #7809, 4.000000000000003553 ) ;
#19989 = LINE ( 'NONE', #5506, #10151 ) ;
#19990 = EDGE_LOOP ( 'NONE', ( #9103, #10389, #11713, #23659 ) ) ;
#19991 = AXIS2_PLACEMENT_3D ( 'NONE', #24072, #2869, #575 ) ;
#19992 = CARTESIAN_POINT ( 'NONE',  ( 36.54859390953724585, -22.18451583373416014, -17.64281456791166036 ) ) ;
#19993 = CARTESIAN_POINT ( 'NONE',  ( 15.94478687392618355, 4.193953704849600506, -19.05305658475056063 ) ) ;
#19994 = LINE ( 'NONE', #1695, #14893 ) ;
#19995 = VECTOR ( 'NONE', #3688, 1000.000000000000000 ) ;
#19996 = EDGE_CURVE ( 'NONE', #357, #18105, #6160, .T. ) ;
#19997 = FACE_BOUND ( 'NONE', #27639, .T. ) ;
#19998 = EDGE_CURVE ( 'NONE', #5507, #10809, #19883, .T. ) ;
#19999 = VECTOR ( 'NONE', #16366, 1000.000000000000000 ) ;
#20000 = ADVANCED_FACE ( 'NONE', ( #24783 ), #24477, .T. ) ;
#20001 = ADVANCED_FACE ( 'NONE', ( #3874 ), #17596, .T. ) ;
#20002 = ORIENTED_EDGE ( 'NONE', *, *, #12550, .T. ) ;
#20003 = FACE_OUTER_BOUND ( 'NONE', #28025, .T. ) ;
#20004 = CARTESIAN_POINT ( 'NONE',  ( 34.75406370242679799, -18.61511248754081294, -20.11778113987843852 ) ) ;
#20005 = DIRECTION ( 'NONE',  ( -2.698458740408365879E-16, 1.000000000000000000, 0.000000000000000000 ) ) ;
#20006 = EDGE_LOOP ( 'NONE', ( #21914, #180, #23684, #28563 ) ) ;
#20007 = CARTESIAN_POINT ( 'NONE',  ( 137.0152310637605808, -1.999999999999979572, -34.70218595412750773 ) ) ;
#20008 = CARTESIAN_POINT ( 'NONE',  ( 12.24710219714225268, 9.516853694884586545, -15.33174803936941366 ) ) ;
#20009 = CARTESIAN_POINT ( 'NONE',  ( 33.27037009343090546, -12.05169513820189309, -19.60996450177851713 ) ) ;
#20010 = CARTESIAN_POINT ( 'NONE',  ( 75.00000000000000000, 6.901118539064950623E-16, -4.188000000000025480 ) ) ;
#20011 = VERTEX_POINT ( 'NONE', #26793 ) ;
#20012 = EDGE_LOOP ( 'NONE', ( #12485, #29332, #20570, #22654, #20848 ) ) ;
#20013 = CARTESIAN_POINT ( 'NONE',  ( 12.54775956925048774, 7.553149829897631840, -15.09063234640338003 ) ) ;
#20014 = FACE_OUTER_BOUND ( 'NONE', #9397, .T. ) ;
#20015 = CARTESIAN_POINT ( 'NONE',  ( 157.2287565553229740, -4.999999999999975131, -12.16987298107780013 ) ) ;
#20016 = CARTESIAN_POINT ( 'NONE',  ( 106.9380661249224715, -4.999999999999988454, 77.69505290240560669 ) ) ;
#20017 = ORIENTED_EDGE ( 'NONE', *, *, #4156, .T. ) ;
#20018 = CARTESIAN_POINT ( 'NONE',  ( 12.86829554393394659, 9.516053645290590168, -16.11540084779614546 ) ) ;
#20019 = VECTOR ( 'NONE', #27490, 1000.000000000000000 ) ;
#20021 = CIRCLE ( 'NONE', #1046, 0.2500000000000002220 ) ;
#20020 = CARTESIAN_POINT ( 'NONE',  ( 36.29797175594614345, -20.05860325589622661, -19.47188034632657150 ) ) ;
#20022 = CARTESIAN_POINT ( 'NONE',  ( 22.51149892830068211, -1.106640851078940502, -13.23823320067571885 ) ) ;
#20023 = ORIENTED_EDGE ( 'NONE', *, *, #22360, .T. ) ;
#20024 = DIRECTION ( 'NONE',  ( 0.5877852522924731371, 1.586114251531760728E-16, -0.8090169943749474513 ) ) ;
#20025 = CARTESIAN_POINT ( 'NONE',  ( 25.00000000000000000, 0.000000000000000000, 2.055000000000000160 ) ) ;
#20026 = CARTESIAN_POINT ( 'NONE',  ( 167.0152310637604671, -1.999999999999971356, -17.38167787843871182 ) ) ;
#20027 = EDGE_CURVE ( 'NONE', #8429, #16190, #3575, .T. ) ;
#20028 = CARTESIAN_POINT ( 'NONE',  ( 22.75855789899217640, -7.280205122891536540, -14.30210469086359915 ) ) ;
#20029 = CARTESIAN_POINT ( 'NONE',  ( 17.05751464226099401, 1.788256342680895949, -18.14502383782993888 ) ) ;
#20030 = EDGE_LOOP ( 'NONE', ( #28441, #1680, #4766, #26596 ) ) ;
#20031 = ORIENTED_EDGE ( 'NONE', *, *, #7941, .F. ) ;
#20032 = DIRECTION ( 'NONE',  ( 1.000000000000000000, 0.000000000000000000, 0.000000000000000000 ) ) ;
#20033 = EDGE_CURVE ( 'NONE', #19224, #16563, #29030, .T. ) ;
#20034 = EDGE_CURVE ( 'NONE', #29341, #26603, #26564, .T. ) ;
#20035 = FILL_AREA_STYLE_COLOUR ( '', #24332 ) ;
#20036 = EDGE_CURVE ( 'NONE', #19188, #6532, #24330, .T. ) ;
#20037 = EDGE_CURVE ( 'NONE', #17144, #28891, #15147, .T. ) ;
#20038 = CARTESIAN_POINT ( 'NONE',  ( 144.5152310637606092, -10.00000000000000178, -28.60870317832789311 ) ) ;
#20039 = CIRCLE ( 'NONE', #15143, 1.500000000000001332 ) ;
#20040 = CARTESIAN_POINT ( 'NONE',  ( 177.2287565553228603, -9.999999999999994671, -12.16987298107780369 ) ) ;
#20041 = PLANE ( 'NONE',  #3852 ) ;
#20042 = VECTOR ( 'NONE', #18102, 1000.000000000000000 ) ;
#20043 = DIRECTION ( 'NONE',  ( -2.698458740408365879E-16, 1.000000000000000000, 0.000000000000000000 ) ) ;
#20044 = CARTESIAN_POINT ( 'NONE',  ( 11.22373969136065242, 9.091953032947756697, -17.24166845096988609 ) ) ;
#20045 = ORIENTED_EDGE ( 'NONE', *, *, #20781, .F. ) ;
#20046 = CARTESIAN_POINT ( 'NONE',  ( 10.33811693838771717, 18.38618951776012267, -17.91796598306941135 ) ) ;
#20047 = CARTESIAN_POINT ( 'NONE',  ( 26.86433939054618492, -2.362129714094441724, -16.96571632802953644 ) ) ;
#20048 = VERTEX_POINT ( 'NONE', #1288 ) ;
#20049 = FACE_OUTER_BOUND ( 'NONE', #5886, .T. ) ;
#20050 = CARTESIAN_POINT ( 'NONE',  ( -7.806255641895631925E-14, -4.618802153517044928, -0.3572655899081716435 ) ) ;
#20051 = VERTEX_POINT ( 'NONE', #30011 ) ;
#20052 = CARTESIAN_POINT ( 'NONE',  ( 9.910898653440767703, 16.43271037397421708, -16.50709950392603531 ) ) ;
#20053 = CARTESIAN_POINT ( 'NONE',  ( 172.0152310637604671, -1.999999999999969580, -26.04193191628311155 ) ) ;
#20054 = CARTESIAN_POINT ( 'NONE',  ( 24.81358459371387326, -5.676498915796258871, -18.90393244824272756 ) ) ;
#20055 = VERTEX_POINT ( 'NONE', #18657 ) ;
#20056 = CARTESIAN_POINT ( 'NONE',  ( 146.1922820468853956, -1.999999999999978018, -4.936203717676158398 ) ) ;
#20057 = CARTESIAN_POINT ( 'NONE',  ( 12.27670864112623583, 9.495496515443743846, -15.31077793565516565 ) ) ;
#20058 = CARTESIAN_POINT ( 'NONE',  ( 31.15806985163746390, -10.82494328065958911, -14.16671120874331358 ) ) ;
#20059 = CARTESIAN_POINT ( 'NONE',  ( 137.2287565553230309, -1.999999999999979572, -20.83012701892220164 ) ) ;
#20060 = CARTESIAN_POINT ( 'NONE',  ( 25.73595588610537277, -4.826321120321507507, -18.84379041344559269 ) ) ;
#20061 = DIRECTION ( 'NONE',  ( 1.110223024625156540E-16, 2.995891024602366092E-32, 1.000000000000000000 ) ) ;
#20062 = CARTESIAN_POINT ( 'NONE',  ( 22.65699622776610411, 4.567421951779635947, -17.29570926971318556 ) ) ;
#20063 = ORIENTED_EDGE ( 'NONE', *, *, #3790, .T. ) ;
#20064 = CARTESIAN_POINT ( 'NONE',  ( 35.54859390953724585, -22.18451583373416014, -17.22552805718784441 ) ) ;
#20065 = ORIENTED_EDGE ( 'NONE', *, *, #20203, .T. ) ;
#20066 = CARTESIAN_POINT ( 'NONE',  ( 18.35279563442798079, 9.979516425631709708, -19.26739628155305439 ) ) ;
#20067 = CARTESIAN_POINT ( 'NONE',  ( 27.84123584509972815, -2.508445798277625371, -17.45642919975013285 ) ) ;
#20068 = EDGE_LOOP ( 'NONE', ( #22816, #26730, #3907, #21307 ) ) ;
#20069 = CARTESIAN_POINT ( 'NONE',  ( 29.76939623719675510, -8.219725197086590995, -17.35520659559267287 ) ) ;
#20070 = PRODUCT ( 'link rod', 'link rod', '', ( #774 ) ) ;
#20071 = EDGE_CURVE ( 'NONE', #184, #6491, #28551, .T. ) ;
#20072 = CIRCLE ( 'NONE', #7894, 5.000000000000000000 ) ;
#20073 = EDGE_CURVE ( 'NONE', #8429, #21438, #20776, .T. ) ;
#20074 = EDGE_CURVE ( 'NONE', #12292, #28345, #25675, .T. ) ;
#20075 = CARTESIAN_POINT ( 'NONE',  ( 172.7287565553229456, -4.999999999999970690, 3.500000000000003109 ) ) ;
#20076 = EDGE_CURVE ( 'NONE', #3757, #16768, #15900, .T. ) ;
#20077 = EDGE_CURVE ( 'NONE', #8074, #28209, #22788, .T. ) ;
#20078 = CARTESIAN_POINT ( 'NONE',  ( 143.6922820468854525, -1.999999999999977573, -15.07341522555727664 ) ) ;
#20079 = CARTESIAN_POINT ( 'NONE',  ( 5.200000000000002842, 0.000000000000000000, 0.000000000000000000 ) ) ;
#20080 = DIRECTION ( 'NONE',  ( -2.698458740408365879E-16, 1.000000000000000000, 0.000000000000000000 ) ) ;
#20081 = VECTOR ( 'NONE', #22590, 999.9999999999998863 ) ;
#20082 = DIRECTION ( 'NONE',  ( 1.000000000000000000, -0.000000000000000000, 0.000000000000000000 ) ) ;
#20083 = CARTESIAN_POINT ( 'NONE',  ( 27.58270427615865472, -5.135490454175970498, -17.42064064436273085 ) ) ;
#20084 = CARTESIAN_POINT ( 'NONE',  ( 0.000000000000000000, 0.000000000000000000, 4.999999999999998224 ) ) ;
#20085 = CARTESIAN_POINT ( 'NONE',  ( 33.60507142094932931, -10.68002793468083134, -20.32431474444524255 ) ) ;
#20086 = CARTESIAN_POINT ( 'NONE',  ( 134.5152310637605808, -10.00000000000000533, -19.94844914048349338 ) ) ;
#20087 = CARTESIAN_POINT ( 'NONE',  ( 9.920751600319857033, 16.38752350362809551, -16.50277044458016107 ) ) ;
#20088 = DIRECTION ( 'NONE',  ( 0.9773680663943725699, 5.871577894680254031E-18, -0.2115458881484706954 ) ) ;
#20089 = LINE ( 'NONE', #29465, #19753 ) ;
#20090 = CARTESIAN_POINT ( 'NONE',  ( 13.13744203029165369, 8.576964204390579383, -15.90088637244482150 ) ) ;
#20091 = DIRECTION ( 'NONE',  ( -0.5877852522924731371, -1.586114251531760235E-16, 0.8090169943749474513 ) ) ;
#20092 = CARTESIAN_POINT ( 'NONE',  ( 2.500000000000000444, 1.768423874527823347, -1.021000000000001018 ) ) ;
#20093 = CARTESIAN_POINT ( 'NONE',  ( 9.936961226781097167, 16.31318409042999917, -16.49606719383117337 ) ) ;
#20094 = ORIENTED_EDGE ( 'NONE', *, *, #8983, .F. ) ;
#20095 = CARTESIAN_POINT ( 'NONE',  ( 172.7287565553229456, -9.999999999999980460, -33.50000000000000000 ) ) ;
#20096 = DIRECTION ( 'NONE',  ( -1.110223024625156540E-16, 0.000000000000000000, -1.000000000000000000 ) ) ;
#20097 = EDGE_LOOP ( 'NONE', ( #16307, #24027 ) ) ;
#20098 = CARTESIAN_POINT ( 'NONE',  ( 146.1922820468854525, -10.00000000000000178, -19.40354224447947828 ) ) ;
#20099 = EDGE_LOOP ( 'NONE', ( #6982, #22236, #15598, #21174 ) ) ;
#20100 = CARTESIAN_POINT ( 'NONE',  ( 8.944592922245861999, 16.95155497634765851, -17.90742740301624991 ) ) ;
#20101 = CARTESIAN_POINT ( 'NONE',  ( 34.83580697690636185, -15.48987143388560384, -21.11455094357481244 ) ) ;
#20102 = CARTESIAN_POINT ( 'NONE',  ( 12.89848499713582441, 9.804829593628518580, -14.81257543621576112 ) ) ;
#20103 = CARTESIAN_POINT ( 'NONE',  ( 28.67543231808702942, -10.82877479041544433, -19.00874469794426602 ) ) ;
#20104 = LINE ( 'NONE', #27017, #939 ) ;
#20105 = CARTESIAN_POINT ( 'NONE',  ( 22.60637239937631193, -5.000000000000011546, -69.57526016881355702 ) ) ;
#20106 = AXIS2_PLACEMENT_3D ( 'NONE', #28869, #1202, #10486 ) ;
#20107 = FACE_OUTER_BOUND ( 'NONE', #21762, .T. ) ;
#20108 = EDGE_LOOP ( 'NONE', ( #4044, #17831, #11785, #3376 ) ) ;
#20109 = VERTEX_POINT ( 'NONE', #2193 ) ;
#20110 = CARTESIAN_POINT ( 'NONE',  ( -19.99999999999999289, 60.00000000000000711, -30.00000000000000711 ) ) ;
#20111 = ADVANCED_FACE ( 'NONE', ( #9478 ), #9019, .T. ) ;
#20112 = AXIS2_PLACEMENT_3D ( 'NONE', #18456, #13279, #1859 ) ;
#20113 = DIRECTION ( 'NONE',  ( 0.3090169943749472292, 8.338696094057992503E-17, -0.9510565162951536422 ) ) ;
#20114 = DIRECTION ( 'NONE',  ( 0.3090169943749472292, 8.338696094057992503E-17, -0.9510565162951536422 ) ) ;
#20115 = CARTESIAN_POINT ( 'NONE',  ( 13.25994536507779742, 8.631100619704961119, -15.80324905228922994 ) ) ;
#20116 = CARTESIAN_POINT ( 'NONE',  ( 34.33808118748100924, -15.74632339993765484, -18.94971805680347998 ) ) ;
#20117 = CARTESIAN_POINT ( 'NONE',  ( 9.112830967032516938, 16.17999385759334885, -17.05460035006107589 ) ) ;
#20118 = ORIENTED_EDGE ( 'NONE', *, *, #21201, .F. ) ;
#20119 = LINE ( 'NONE', #29499, #20019 ) ;
#20120 = CARTESIAN_POINT ( 'NONE',  ( 12.86829554393394659, 9.516053645290590168, -16.11540084779614546 ) ) ;
#20121 = FACE_BOUND ( 'NONE', #15630, .T. ) ;
#20122 = VERTEX_POINT ( 'NONE', #11462 ) ;
#20123 = ORIENTED_EDGE ( 'NONE', *, *, #28580, .F. ) ;
#20124 = LINE ( 'NONE', #10505, #29595 ) ;
#20125 = ORIENTED_EDGE ( 'NONE', *, *, #19345, .F. ) ;
#20126 = CARTESIAN_POINT ( 'NONE',  ( 11.92109019680886206, 8.606374460406147620, -15.56934379943068336 ) ) ;
#20127 = LINE ( 'NONE', #4261, #16924 ) ;
#20128 = CARTESIAN_POINT ( 'NONE',  ( 5.000000000000006217, 2.220446049250313870E-15, -5.000000000000000888 ) ) ;
#20129 = ORIENTED_EDGE ( 'NONE', *, *, #23733, .T. ) ;
#20130 = CARTESIAN_POINT ( 'NONE',  ( 9.661883073086391605, 16.25482658099627642, -17.91571305590050400 ) ) ;
#20131 = ADVANCED_FACE ( 'NONE', ( #7062 ), #23232, .T. ) ;
#20132 = EDGE_CURVE ( 'NONE', #5003, #26592, #30167, .T. ) ;
#20133 = CARTESIAN_POINT ( 'NONE',  ( 17.64024190839899120, 8.465516882244152441, -14.08803959672746586 ) ) ;
#20134 = CARTESIAN_POINT ( 'NONE',  ( 16.96299543436377633, 3.857017182823994084, -13.23919852190412527 ) ) ;
#20135 = DIRECTION ( 'NONE',  ( -0.5877852522924731371, 0.000000000000000000, 0.8090169943749474513 ) ) ;
#20136 = VERTEX_POINT ( 'NONE', #21090 ) ;
#20137 = CARTESIAN_POINT ( 'NONE',  ( 176.1922820468853104, -9.999999999999994671, -19.40354224447947828 ) ) ;
#20138 = CARTESIAN_POINT ( 'NONE',  ( 22.51149892830068211, -1.106640851078940502, -13.23823320067571885 ) ) ;
#20139 = AXIS2_PLACEMENT_3D ( 'NONE', #7543, #24176, #2828 ) ;
#20140 = LINE ( 'NONE', #15254, #13462 ) ;
#20141 = CARTESIAN_POINT ( 'NONE',  ( -4.000000000000000000, -1.286498119741307703E-15, 1.699999999999996625 ) ) ;
#20142 = ORIENTED_EDGE ( 'NONE', *, *, #138, .F. ) ;
#20143 = DIRECTION ( 'NONE',  ( -0.8090169943749474513, -2.183098979609982436E-16, 0.5877852522924731371 ) ) ;
#20144 = CARTESIAN_POINT ( 'NONE',  ( 34.93238815599637803, -19.41622979634004764, -20.17168434421570922 ) ) ;
#20145 = DIRECTION ( 'NONE',  ( -0.5877852522924731371, 0.000000000000000000, 0.8090169943749474513 ) ) ;
#20146 = EDGE_LOOP ( 'NONE', ( #8821, #2964, #16332, #27485, #21977 ) ) ;
#20147 = ORIENTED_EDGE ( 'NONE', *, *, #16442, .F. ) ;
#20148 = DIRECTION ( 'NONE',  ( 0.9510565162951536422, 2.566386769018988816E-16, 0.3090169943749472292 ) ) ;
#20149 = CARTESIAN_POINT ( 'NONE',  ( 11.05541531668977662, 17.68942339022145305, -17.95086732675816776 ) ) ;
#20150 = CARTESIAN_POINT ( 'NONE',  ( 32.74314609665832165, -11.10724048739539782, -18.62249297335446840 ) ) ;
#20151 = ORIENTED_EDGE ( 'NONE', *, *, #22362, .T. ) ;
#20152 = CARTESIAN_POINT ( 'NONE',  ( 9.641350810849047548, 17.66889113945805789, -19.66666666666842644 ) ) ;
#20153 = VECTOR ( 'NONE', #29493, 1000.000000000000000 ) ;
#20154 = CARTESIAN_POINT ( 'NONE',  ( 10.63628302936969483, 9.193248504745362482, -16.42459933240677827 ) ) ;
#20155 = FACE_OUTER_BOUND ( 'NONE', #10857, .T. ) ;
#20156 = SURFACE_STYLE_USAGE ( .BOTH. , #1876 ) ;
#20157 = FACE_OUTER_BOUND ( 'NONE', #17411, .T. ) ;
#20158 = VERTEX_POINT ( 'NONE', #4314 ) ;
#20159 = CARTESIAN_POINT ( 'NONE',  ( 10.35864918915110877, 16.97212501191939538, -17.92279151347709032 ) ) ;
#20160 = EDGE_CURVE ( 'NONE', #6062, #28330, #2503, .T. ) ;
#20161 = EDGE_CURVE ( 'NONE', #4310, #23706, #16354, .T. ) ;
#20162 = CARTESIAN_POINT ( 'NONE',  ( 34.43765690731135720, -12.70119407716533111, -19.95187818093482335 ) ) ;
#20163 = CARTESIAN_POINT ( 'NONE',  ( 22.86252235622482587, -0.9498377794471745128, -13.29674124224850118 ) ) ;
#20164 = ORIENTED_EDGE ( 'NONE', *, *, #26323, .F. ) ;
#20165 = ORIENTED_EDGE ( 'NONE', *, *, #19781, .T. ) ;
#20166 = EDGE_CURVE ( 'NONE', #28008, #26448, #9174, .T. ) ;
#20167 = VERTEX_POINT ( 'NONE', #11324 ) ;
#20168 = LINE ( 'NONE', #13302, #13536 ) ;
#20169 = EDGE_CURVE ( 'NONE', #21151, #29771, #9328, .T. ) ;
#20170 = CARTESIAN_POINT ( 'NONE',  ( 174.7287565553228603, -9.999999999999996447, -7.839745962155603820 ) ) ;
#20171 = CARTESIAN_POINT ( 'NONE',  ( -20.00000000000017053, 34.64101615137744972, 0.000000000000000000 ) ) ;
#20172 = CARTESIAN_POINT ( 'NONE',  ( 27.15293434934692129, -9.258526923162836653, -12.62629486378885701 ) ) ;
#20173 = CARTESIAN_POINT ( 'NONE',  ( 28.35258904315412920, -6.370284285516064848, -14.91745349193007364 ) ) ;
#20174 = EDGE_LOOP ( 'NONE', ( #21028, #22472, #22300, #22509 ) ) ;
#20175 = ORIENTED_EDGE ( 'NONE', *, *, #11834, .F. ) ;
#20176 = DIRECTION ( 'NONE',  ( -0.5877852522924731371, -1.586114251531760235E-16, 0.8090169943749474513 ) ) ;
#20177 = LINE ( 'NONE', #10724, #11634 ) ;
#20178 = VECTOR ( 'NONE', #27135, 1000.000000000000000 ) ;
#20179 = CARTESIAN_POINT ( 'NONE',  ( 151.1922820468854525, -1.999999999999975353, -30.91696583120936026 ) ) ;
#20180 = CARTESIAN_POINT ( 'NONE',  ( 174.5152310637604387, -1.999999999999969358, -21.71180489736091346 ) ) ;
#20181 = CARTESIAN_POINT ( 'NONE',  ( -8.000000000000000000, 0.000000000000000000, 18.00000000000000000 ) ) ;
#20182 = LINE ( 'NONE', #10578, #4137 ) ;
#20183 = CARTESIAN_POINT ( 'NONE',  ( 11.22782251818125232, 9.073501160497098539, -17.23995927586370769 ) ) ;
#20184 = VECTOR ( 'NONE', #18660, 1000.000000000000000 ) ;
#20185 = CARTESIAN_POINT ( 'NONE',  ( 12.51417009928267099, 8.576964204390579383, -15.11888119342340353 ) ) ;
#20186 = CARTESIAN_POINT ( 'NONE',  ( 27.03191753302054323, -12.88672130028117735, -14.08881772908025454 ) ) ;
#20187 = ORIENTED_EDGE ( 'NONE', *, *, #8936, .F. ) ;
#20188 = DIRECTION ( 'NONE',  ( 1.000000000000000000, 2.698458740408365879E-16, -1.110223024625156540E-16 ) ) ;
#20189 = DIRECTION ( 'NONE',  ( 1.000000000000000000, 2.698458740408365879E-16, 0.000000000000000000 ) ) ;
#20190 = ORIENTED_EDGE ( 'NONE', *, *, #11445, .F. ) ;
#20191 = CARTESIAN_POINT ( 'NONE',  ( 9.641350835837977584, 17.66889102485563612, -17.91507476468484938 ) ) ;
#20192 = FACE_OUTER_BOUND ( 'NONE', #23942, .T. ) ;
#20193 = CYLINDRICAL_SURFACE ( 'NONE', #15104, 40.00000000000000711 ) ;
#20194 = DIRECTION ( 'NONE',  ( 0.000000000000000000, 0.4999999999999993894, -0.8660254037844389297 ) ) ;
#20196 = ORIENTED_EDGE ( 'NONE', *, *, #10994, .T. ) ;
#20195 = CARTESIAN_POINT ( 'NONE',  ( 26.72181814967143509, -3.137724904577397389, -15.69709663067708050 ) ) ;
#20197 = ORIENTED_EDGE ( 'NONE', *, *, #13854, .F. ) ;
#20198 = LINE ( 'NONE', #8598, #9077 ) ;
#20199 = CARTESIAN_POINT ( 'NONE',  ( 12.24513942169458858, 9.516104476910269838, -15.33330339355663519 ) ) ;
#20200 = EDGE_CURVE ( 'NONE', #25023, #20167, #28001, .T. ) ;
#20201 = CARTESIAN_POINT ( 'NONE',  ( -5.000000000000000000, 0.000000000000000000, 18.00000000000000000 ) ) ;
#20202 = LINE ( 'NONE', #19906, #1546 ) ;
#20203 = EDGE_CURVE ( 'NONE', #16222, #1559, #198, .T. ) ;
#20204 = ADVANCED_FACE ( 'NONE', ( #20631 ), #16209, .T. ) ;
#20205 = CARTESIAN_POINT ( 'NONE',  ( 24.14317479683219858, -6.286850201977149055, -18.60698471650063723 ) ) ;
#20206 = AXIS2_PLACEMENT_3D ( 'NONE', #8137, #22335, #24939 ) ;
#20207 = DIRECTION ( 'NONE',  ( -1.000000000000000000, 0.000000000000000000, 0.000000000000000000 ) ) ;
#20208 = EDGE_CURVE ( 'NONE', #12491, #13323, #12894, .T. ) ;
#20209 = CARTESIAN_POINT ( 'NONE',  ( 21.34664435287406903, -1.670712410592182895, -14.88600020661825063 ) ) ;
#20210 = ORIENTED_EDGE ( 'NONE', *, *, #20702, .F. ) ;
#20211 = DIRECTION ( 'NONE',  ( 1.000000000000000000, 4.440892098500622217E-16, 0.000000000000000000 ) ) ;
#20212 = CARTESIAN_POINT ( 'NONE',  ( 31.01114313885700824, -11.37490951371675507, -12.31627997798639917 ) ) ;
#20213 = CARTESIAN_POINT ( 'NONE',  ( 24.28706804496593463, -0.4963248009486594392, -19.74393692370418307 ) ) ;
#20214 = ORIENTED_EDGE ( 'NONE', *, *, #6329, .T. ) ;
#20215 = CARTESIAN_POINT ( 'NONE',  ( 24.62590367393082502, -9.567571807129121808, -15.85044010117769098 ) ) ;
#20216 = B_SPLINE_CURVE_WITH_KNOTS ( 'NONE', 3,
 ( #22624, #21182, #25475, #145, #4710, #445, #16300, #4566 ),
 .UNSPECIFIED., .F., .F.,
 ( 4, 2, 2, 4 ),
 ( 0.004673709593152147908, 0.005837709341827640799, 0.007001709090503132824, 0.009329708587854118607 ),
 .UNSPECIFIED. ) ;
#20217 = CARTESIAN_POINT ( 'NONE',  ( 164.5152310637604671, -9.999999999999998224, -13.05155085951651195 ) ) ;
#20218 = LINE ( 'NONE', #4352, #6343 ) ;
#20219 = LINE ( 'NONE', #25267, #22825 ) ;
#20220 = CARTESIAN_POINT ( 'NONE',  ( 134.5152310637605524, -4.999999999999981348, -1.493419066897600538E-14 ) ) ;
#20221 = CIRCLE ( 'NONE', #25600, 4.000000000000003553 ) ;
#20222 = PLANE ( 'NONE',  #15031 ) ;
#20223 = CARTESIAN_POINT ( 'NONE',  ( 27.43603605124483025, -4.716368786860208218, -15.63773258035017300 ) ) ;
#20224 = CARTESIAN_POINT ( 'NONE',  ( 16.63724033897865340, 2.930722838386041751, -15.17604395537502526 ) ) ;
#20225 = CARTESIAN_POINT ( 'NONE',  ( 33.34778169882233811, -10.20066162918134367, -19.85315749909214844 ) ) ;
#20226 = CARTESIAN_POINT ( 'NONE',  ( -8.000000000000003553, -4.618802153517028941, -5.000000000000000888 ) ) ;
#20227 = CARTESIAN_POINT ( 'NONE',  ( 11.46877092736959014, 9.288109543210406827, -15.86260999805022820 ) ) ;
#20228 = DIRECTION ( 'NONE',  ( 0.9510565162951536422, 2.566386769018988816E-16, 0.3090169943749472292 ) ) ;
#20229 = CARTESIAN_POINT ( 'NONE',  ( 119.9999999999999858, -30.00000000000000000, -186.4312945166758482 ) ) ;
#20230 = CARTESIAN_POINT ( 'NONE',  ( 9.661883060892410668, 16.25482663691947849, -17.91599866193395485 ) ) ;
#20231 = CARTESIAN_POINT ( 'NONE',  ( 92.57941663348161399, -4.999999999999992006, 67.26288340215127448 ) ) ;
#20232 = DIRECTION ( 'NONE',  ( -2.698458740408365879E-16, 1.000000000000000000, 0.000000000000000000 ) ) ;
#20233 = CARTESIAN_POINT ( 'NONE',  ( 12.51757296969303290, 8.578467993704791184, -15.11616904564172792 ) ) ;
#20234 = ORIENTED_EDGE ( 'NONE', *, *, #13818, .F. ) ;
#20235 = DIRECTION ( 'NONE',  ( 0.9510565162951536422, 2.566386769018988816E-16, 0.3090169943749472292 ) ) ;
#20236 = CARTESIAN_POINT ( 'NONE',  ( 158.6922820468853956, -4.999999999999975131, -26.58683881228715862 ) ) ;
#20237 = EDGE_CURVE ( 'NONE', #29592, #15878, #16665, .T. ) ;
#20238 = DIRECTION ( 'NONE',  ( 0.3090169943749475623, 8.338696094058001131E-17, 0.9510565162951536422 ) ) ;
#20239 = ADVANCED_FACE ( 'NONE', ( #17115 ), #26289, .T. ) ;
#20240 = EDGE_CURVE ( 'NONE', #6553, #22621, #16507, .T. ) ;
#20241 = ORIENTED_EDGE ( 'NONE', *, *, #7367, .T. ) ;
#20242 = EDGE_CURVE ( 'NONE', #3218, #14970, #21395, .T. ) ;
#20243 = CARTESIAN_POINT ( 'NONE',  ( 8.944584683310379702, 16.95159276115599667, -17.92981046679734547 ) ) ;
#20244 = CARTESIAN_POINT ( 'NONE',  ( 36.53927379715840829, -23.14264550581856739, -18.86160504153442830 ) ) ;
#20245 = CARTESIAN_POINT ( 'NONE',  ( 15.19363621961471722, 2.181190162186355419, -17.24139079752846015 ) ) ;
#20246 = CARTESIAN_POINT ( 'NONE',  ( 28.67999647541807207, -5.919990246138143952, -18.25217309140403188 ) ) ;
#20247 = LINE ( 'NONE', #29483, #2407 ) ;
#20248 = PLANE ( 'NONE',  #17658 ) ;
#20249 = CARTESIAN_POINT ( 'NONE',  ( 19.78633661418711043, -4.982883274218824710, -16.00186916550291727 ) ) ;
#20250 = EDGE_LOOP ( 'NONE', ( #17710, #4169, #21315, #25895 ) ) ;
#20251 = DIRECTION ( 'NONE',  ( -0.5877852522924731371, -1.586114251531760728E-16, -0.8090169943749474513 ) ) ;
#20252 = VECTOR ( 'NONE', #5423, 1000.000000000000000 ) ;
#20254 = VERTEX_POINT ( 'NONE', #26138 ) ;
#20253 = CARTESIAN_POINT ( 'NONE',  ( 146.1922820468853956, -10.00000000000000355, -2.083034168790677043 ) ) ;
#20255 = PLANE ( 'NONE',  #28340 ) ;
#20256 = DIRECTION ( 'NONE',  ( -0.000000000000000000, -0.000000000000000000, 1.000000000000000000 ) ) ;
#20257 = AXIS2_PLACEMENT_3D ( 'NONE', #11551, #15992, #30250 ) ;
#20258 = DIRECTION ( 'NONE',  ( 0.5877852522924731371, 1.586114251531760728E-16, 0.8090169943749474513 ) ) ;
#20259 = CARTESIAN_POINT ( 'NONE',  ( 34.76605987604303749, -17.66900494105776787, -19.07908574721388462 ) ) ;
#20260 = ORIENTED_EDGE ( 'NONE', *, *, #10905, .T. ) ;
#20261 = VECTOR ( 'NONE', #2397, 1000.000000000000000 ) ;
#20262 = CARTESIAN_POINT ( 'NONE',  ( 10.76353862942338147, 8.717528283631100550, -16.36374602157236779 ) ) ;
#20263 = ORIENTED_EDGE ( 'NONE', *, *, #10773, .T. ) ;
#20264 =( GEOMETRIC_REPRESENTATION_CONTEXT ( 3 ) GLOBAL_UNCERTAINTY_ASSIGNED_CONTEXT ( ( #28160 ) ) GLOBAL_UNIT_ASSIGNED_CONTEXT ( ( #19239, #21836, #7944 ) ) REPRESENTATION_CONTEXT ( 'NONE', 'WORKASPACE' ) );
#20265 = CARTESIAN_POINT ( 'NONE',  ( 29.82081855766934453, -7.722587238354316597, -15.76009366473342332 ) ) ;
#20266 = CARTESIAN_POINT ( 'NONE',  ( 12.97729766242475868, 9.564223303342972216, -16.02852426037668465 ) ) ;
#20267 = LINE ( 'NONE', #6699, #19474 ) ;
#20268 = ORIENTED_EDGE ( 'NONE', *, *, #5398, .T. ) ;
#20269 = CARTESIAN_POINT ( 'NONE',  ( 129.5152310637605524, -1.999999999999982236, -4.391296821672111328 ) ) ;
#20270 = EDGE_CURVE ( 'NONE', #3702, #4351, #20221, .T. ) ;
#20271 = CARTESIAN_POINT ( 'NONE',  ( 12.60945047077962933, 8.619070305187777947, -15.04294105552940231 ) ) ;
#20272 = DIRECTION ( 'NONE',  ( 0.000000000000000000, 0.000000000000000000, -1.000000000000000000 ) ) ;
#20273 = ORIENTED_EDGE ( 'NONE', *, *, #3077, .F. ) ;
#20274 = CARTESIAN_POINT ( 'NONE',  ( 133.7287565553229172, -4.999999999999981348, -33.50000000000000000 ) ) ;
#20275 = EDGE_LOOP ( 'NONE', ( #22112, #28027, #13527, #28510 ) ) ;
#20276 = EDGE_CURVE ( 'NONE', #29492, #13148, #5375, .T. ) ;
#20277 = CARTESIAN_POINT ( 'NONE',  ( 9.661883061612440926, 16.25482663361732705, -19.66666666666843000 ) ) ;
#20278 = CARTESIAN_POINT ( 'NONE',  ( 22.18718699900398761, -4.329393945612883599, -17.49580572735151307 ) ) ;
#20279 = CARTESIAN_POINT ( 'NONE',  ( 18.26434493437671946, 4.448125397982363616, -12.89349226661579273 ) ) ;
#20280 = VECTOR ( 'NONE', #9382, 1000.000000000000000 ) ;
#20281 = PLANE ( 'NONE',  #19413 ) ;
#20282 = LINE ( 'NONE', #16157, #13733 ) ;
#20283 = VECTOR ( 'NONE', #16370, 1000.000000000000000 ) ;
#20284 = CARTESIAN_POINT ( 'NONE',  ( 23.86551563699305234, 2.542095107771292106, -17.79649620197707094 ) ) ;
#20285 = AXIS2_PLACEMENT_3D ( 'NONE', #3581, #20188, #29569 ) ;
#20286 = PLANE ( 'NONE',  #12992 ) ;
#20287 = LINE ( 'NONE', #11289, #17666 ) ;
#20288 = ORIENTED_EDGE ( 'NONE', *, *, #28524, .F. ) ;
#20289 = EDGE_CURVE ( 'NONE', #21069, #13830, #14510, .T. ) ;
#20290 = CARTESIAN_POINT ( 'NONE',  ( 175.7287565553229456, -4.999999999999970690, 3.500000000000003109 ) ) ;
#20291 = CARTESIAN_POINT ( 'NONE',  ( 32.63711423693117553, -11.05166607373017484, -18.34576405707344549 ) ) ;
#20292 = DIRECTION ( 'NONE',  ( -0.9510565162951536422, 0.000000000000000000, -0.3090169943749472292 ) ) ;
#20293 = ORIENTED_EDGE ( 'NONE', *, *, #28413, .T. ) ;
#20294 = LINE ( 'NONE', #16174, #5623 ) ;
#20295 = AXIS2_PLACEMENT_3D ( 'NONE', #19752, #29122, #8162 ) ;
#20296 = CARTESIAN_POINT ( 'NONE',  ( 15.39489021548154568, 6.697694061803245447, -14.95590323207311734 ) ) ;
#20297 = CARTESIAN_POINT ( 'NONE',  ( 12.24525513380350539, 9.516155168367477657, -15.33321120281095773 ) ) ;
#20298 = CARTESIAN_POINT ( 'NONE',  ( 33.48796008207983022, -12.92717959506727965, -19.73506838908087246 ) ) ;
#20299 = ORIENTED_EDGE ( 'NONE', *, *, #22242, .F. ) ;
#20300 = VECTOR ( 'NONE', #2922, 1000.000000000000000 ) ;
#20301 = CARTESIAN_POINT ( 'NONE',  ( 9.641350810849047548, 17.66889113945805789, -17.98596209335946128 ) ) ;
#20302 = CIRCLE ( 'NONE', #5204, 4.000000000000004441 ) ;
#20303 = CARTESIAN_POINT ( 'NONE',  ( 9.641566850259106758, 17.66790035518494051, -17.86107206016944460 ) ) ;
#20304 = FACE_BOUND ( 'NONE', #16633, .T. ) ;
#20305 = ORIENTED_EDGE ( 'NONE', *, *, #27431, .F. ) ;
#20306 = DIRECTION ( 'NONE',  ( 0.5877852522924731371, 0.000000000000000000, 0.8090169943749474513 ) ) ;
#20307 = ORIENTED_EDGE ( 'NONE', *, *, #20883, .T. ) ;
#20308 = CARTESIAN_POINT ( 'NONE',  ( 10.35864918915110877, 16.97212501191939538, -19.66666666666842644 ) ) ;
#20309 = CARTESIAN_POINT ( 'NONE',  ( 33.30032953382602301, -10.37518355935928938, -17.98954529685971337 ) ) ;
#20310 = CARTESIAN_POINT ( 'NONE',  ( 19.25770813156441008, -2.543370271471735222, -15.40753146551623587 ) ) ;
#20311 = ORIENTED_EDGE ( 'NONE', *, *, #9412, .T. ) ;
#20312 = VERTEX_POINT ( 'NONE', #14353 ) ;
#20313 = DIRECTION ( 'NONE',  ( -0.5877852522924731371, -1.586114251531760235E-16, 0.8090169943749474513 ) ) ;
#20314 = DIRECTION ( 'NONE',  ( 0.9510565162951535312, 2.566386769018988816E-16, -0.3090169943749475623 ) ) ;
#20315 = LINE ( 'NONE', #11167, #14707 ) ;
#20316 =( NAMED_UNIT ( * ) SI_UNIT ( $, .STERADIAN. ) SOLID_ANGLE_UNIT ( ) );
#20317 = CARTESIAN_POINT ( 'NONE',  ( 26.09074415779471323, -5.786596670875995940, -12.76770422508296932 ) ) ;
#20318 = CARTESIAN_POINT ( 'NONE',  ( 26.04927874075684713, 0.2391533594452614209, -17.67486400872287788 ) ) ;
#20319 = AXIS2_PLACEMENT_3D ( 'NONE', #9942, #22152, #26600 ) ;
#20320 = ORIENTED_EDGE ( 'NONE', *, *, #12270, .T. ) ;
#20321 = ORIENTED_EDGE ( 'NONE', *, *, #26868, .F. ) ;
#20322 = CARTESIAN_POINT ( 'NONE',  ( 180.7287565553229456, -9.999999999999968026, 0.5000000000000029976 ) ) ;
#20323 = AXIS2_PLACEMENT_3D ( 'NONE', #20718, #5007, #14296 ) ;
#20324 = LINE ( 'NONE', #15288, #4827 ) ;
#20325 = DIRECTION ( 'NONE',  ( 1.000000000000000000, 0.000000000000000000, 0.000000000000000000 ) ) ;
#20326 = EDGE_CURVE ( 'NONE', #13853, #22891, #23690, .T. ) ;
#20327 = LINE ( 'NONE', #8579, #12028 ) ;
#20328 = CARTESIAN_POINT ( 'NONE',  ( 114.7516306444886141, -4.999999999999985789, 83.37193982118418489 ) ) ;
#20329 = EDGE_CURVE ( 'NONE', #29150, #22621, #21841, .T. ) ;
#20330 = DIRECTION ( 'NONE',  ( 0.000000000000000000, 0.000000000000000000, 1.000000000000000000 ) ) ;
#20331 = CARTESIAN_POINT ( 'NONE',  ( 11.20373435594124878, 9.183700057499073921, -17.24994136041982529 ) ) ;
#20332 = CARTESIAN_POINT ( 'NONE',  ( 12.47535353872619446, 8.560407331872438519, -15.14977315560688176 ) ) ;
#20333 = DIRECTION ( 'NONE',  ( -1.110223024625156540E-16, 0.000000000000000000, -1.000000000000000000 ) ) ;
#20334 = ORIENTED_EDGE ( 'NONE', *, *, #26225, .F. ) ;
#20335 = DIRECTION ( 'NONE',  ( -2.698458740408365879E-16, 1.000000000000000000, -0.000000000000000000 ) ) ;
#20336 = FACE_OUTER_BOUND ( 'NONE', #13291, .T. ) ;
#20337 = EDGE_LOOP ( 'NONE', ( #28117, #4463, #11307, #7055 ) ) ;
#20338 = CARTESIAN_POINT ( 'NONE',  ( 9.641350810849047548, 17.66889113945805789, -17.92454625180715766 ) ) ;
#20339 = CONICAL_SURFACE ( 'NONE', #8646, 4.000000000000003553, 1.047197551196597853 ) ;
#20340 = CYLINDRICAL_SURFACE ( 'NONE', #19884, 8.000000000000000000 ) ;
#20341 = CARTESIAN_POINT ( 'NONE',  ( 146.1922820468854525, -1.999999999999977573, -28.06379628232387446 ) ) ;
#20342 = DIRECTION ( 'NONE',  ( -1.110223024625156540E-16, 0.000000000000000000, -1.000000000000000000 ) ) ;
#20344 = VERTEX_POINT ( 'NONE', #5523 ) ;
#20343 = CARTESIAN_POINT ( 'NONE',  ( 21.43917814492346707, -4.799604530101110988, -17.97822123721208243 ) ) ;
#20345 = ORIENTED_EDGE ( 'NONE', *, *, #977, .T. ) ;
#20346 = CARTESIAN_POINT ( 'NONE',  ( 154.7287565553230024, -10.00000000000000000, -25.16025403784440329 ) ) ;
#20347 = CARTESIAN_POINT ( 'NONE',  ( 11.05541531668977662, 17.68942339022145305, -17.91928203681695564 ) ) ;
#20348 = VECTOR ( 'NONE', #8386, 1000.000000000000000 ) ;
#20349 = CARTESIAN_POINT ( 'NONE',  ( 35.12509383387676820, -20.28195432802065312, -20.22992657050740917 ) ) ;
#20350 = FACE_BOUND ( 'NONE', #22793, .T. ) ;
#20351 = VERTEX_POINT ( 'NONE', #12372 ) ;
#20352 = CARTESIAN_POINT ( 'NONE',  ( 26.04489551603160180, -6.130266781319400948, -13.71289979607875154 ) ) ;
#20353 = LINE ( 'NONE', #4490, #29664 ) ;
#20354 = CARTESIAN_POINT ( 'NONE',  ( 23.33733100364600688, 1.020658515592549609, -17.81090727445316446 ) ) ;
#20355 = VERTEX_POINT ( 'NONE', #14659 ) ;
#20356 = DIRECTION ( 'NONE',  ( 0.000000000000000000, 0.000000000000000000, -1.000000000000000000 ) ) ;
#20357 = CARTESIAN_POINT ( 'NONE',  ( 17.27944038698359464, 10.59897317215052226, -14.78577975581568360 ) ) ;
#20358 = CARTESIAN_POINT ( 'NONE',  ( 26.92475197568164802, -10.17130474311345800, -13.43658410890694732 ) ) ;
#20359 = EDGE_LOOP ( 'NONE', ( #26735, #26726, #10608, #15980 ) ) ;
#20360 = CARTESIAN_POINT ( 'NONE',  ( -2.000000000000026201, -3.464101615137764156, -2.450000000000000622 ) ) ;
#20361 = VECTOR ( 'NONE', #18083, 1000.000000000000000 ) ;
#20362 = DIRECTION ( 'NONE',  ( -2.698458740408365879E-16, 1.000000000000000000, 0.000000000000000000 ) ) ;
#20363 = ORIENTED_EDGE ( 'NONE', *, *, #23336, .T. ) ;
#20364 = VERTEX_POINT ( 'NONE', #23851 ) ;
#20365 = ADVANCED_FACE ( 'NONE', ( #7365, #2640 ), #351, .T. ) ;
#20366 = CARTESIAN_POINT ( 'NONE',  ( 172.0152310637604955, -1.999999999999969580, -24.27857615940569502 ) ) ;
#20367 = VECTOR ( 'NONE', #28406, 1000.000000000000000 ) ;
#20368 = DIRECTION ( 'NONE',  ( 1.000000000000000000, 4.440892098500622217E-16, 0.000000000000000000 ) ) ;
#20369 = EDGE_CURVE ( 'NONE', #11745, #12555, #9637, .T. ) ;
#20370 = DIRECTION ( 'NONE',  ( -0.5877852522924731371, 0.000000000000000000, 0.8090169943749474513 ) ) ;
#20371 = EDGE_CURVE ( 'NONE', #16793, #24538, #28458, .T. ) ;
#20372 = CARTESIAN_POINT ( 'NONE',  ( 25.27232213581778808, -7.536446408081735271, -18.87890555733638465 ) ) ;
#20373 = CARTESIAN_POINT ( 'NONE',  ( 21.63689124574611711, 4.661388338709377521, -16.95871344450652174 ) ) ;
#20374 = CARTESIAN_POINT ( 'NONE',  ( 34.01601630636088913, -11.85276864474937852, -20.84012540857256823 ) ) ;
#20375 = CARTESIAN_POINT ( 'NONE',  ( 172.0152310637605240, -1.999999999999969358, -32.93883019725009120 ) ) ;
#20376 = CARTESIAN_POINT ( 'NONE',  ( 12.49899259368311988, 8.570259324921714494, -15.13097775544467005 ) ) ;
#20377 = CARTESIAN_POINT ( 'NONE',  ( 153.6922820468854525, -10.00000000000000000, -32.39392330124607611 ) ) ;
#20378 = DIRECTION ( 'NONE',  ( 0.9510565162951535312, 2.566386769018988816E-16, -0.3090169943749475623 ) ) ;
#20379 = CARTESIAN_POINT ( 'NONE',  ( 9.672937757006597081, 16.20412839139380168, -17.88297960302892520 ) ) ;
#20380 = CARTESIAN_POINT ( 'NONE',  ( 4.000000000000008882, -6.928203230275510549, -5.000000000000000888 ) ) ;
#20381 = ORIENTED_EDGE ( 'NONE', *, *, #21384, .F. ) ;
#20382 = FACE_OUTER_BOUND ( 'NONE', #2327, .T. ) ;
#20383 = CARTESIAN_POINT ( 'NONE',  ( 12.50076791318051761, 8.571041463825640250, -15.12956297801270900 ) ) ;
#20384 = VERTEX_POINT ( 'NONE', #7507 ) ;
#20385 = LINE ( 'NONE', #27605, #29116 ) ;
#20386 = LINE ( 'NONE', #18250, #5411 ) ;
#20387 = VECTOR ( 'NONE', #5345, 1000.000000000000000 ) ;
#20388 = CARTESIAN_POINT ( 'NONE',  ( 163.6922820468853672, -9.999999999999998224, -26.58683881228715862 ) ) ;
#20389 = ORIENTED_EDGE ( 'NONE', *, *, #27219, .T. ) ;
#20390 = CARTESIAN_POINT ( 'NONE',  ( 13.37763225631166542, 7.625080029534266224, -15.70945042905673006 ) ) ;
#20391 = CARTESIAN_POINT ( 'NONE',  ( 34.47915806976548936, -13.88763681628941349, -21.00674453490027460 ) ) ;
#20392 = VECTOR ( 'NONE', #21432, 1000.000000000000000 ) ;
#20393 = CARTESIAN_POINT ( 'NONE',  ( 21.48460829514769799, 2.948577479130256584, -19.81588663513211657 ) ) ;
#20394 = CARTESIAN_POINT ( 'NONE',  ( 17.18133768520950255, 3.791981501156216350, -18.48732239789962506 ) ) ;
#20395 = DIRECTION ( 'NONE',  ( -0.5877852522924731371, -1.586114251531760235E-16, 0.8090169943749474513 ) ) ;
#20396 = TOROIDAL_SURFACE ( 'NONE', #30203, 7.000000000000000888, 2.000000000000000000 ) ;
#20397 = CARTESIAN_POINT ( 'NONE',  ( 91.84383324292713269, -4.999999999999992006, 66.72845078601908142 ) ) ;
#20398 = CARTESIAN_POINT ( 'NONE',  ( 18.73701609394335321, -1.228702115187185973, -15.37238819164404369 ) ) ;
#20399 = VECTOR ( 'NONE', #14314, 1000.000000000000000 ) ;
#20400 = ORIENTED_EDGE ( 'NONE', *, *, #2566, .T. ) ;
#20401 = CARTESIAN_POINT ( 'NONE',  ( 20.00000000000017053, 27.64101615137744972, 12.00000000000000178 ) ) ;
#20403 = VERTEX_POINT ( 'NONE', #12229 ) ;
#20402 = FACE_OUTER_BOUND ( 'NONE', #19761, .T. ) ;
#20404 = EDGE_CURVE ( 'NONE', #5129, #28015, #14803, .T. ) ;
#20405 = DIRECTION ( 'NONE',  ( 1.000000000000000000, 2.698458740408365879E-16, -1.110223024625156540E-16 ) ) ;
#20406 = LINE ( 'NONE', #22718, #20153 ) ;
#20407 = EDGE_CURVE ( 'NONE', #9856, #30027, #24143, .T. ) ;
#20408 = ADVANCED_FACE ( 'NONE', ( #3247 ), #24006, .T. ) ;
#20409 = ADVANCED_FACE ( 'NONE', ( #7658 ), #18800, .T. ) ;
#20410 = DIRECTION ( 'NONE',  ( 0.9510565162951535312, 2.566386769018988816E-16, -0.3090169943749475623 ) ) ;
#20411 = CARTESIAN_POINT ( 'NONE',  ( 35.54859390953724585, -21.18451583373416014, -16.11276402859391510 ) ) ;
#20412 = AXIS2_PLACEMENT_3D ( 'NONE', #3720, #8580, #7987 ) ;
#20413 = ORIENTED_EDGE ( 'NONE', *, *, #18138, .T. ) ;
#20414 = CARTESIAN_POINT ( 'NONE',  ( 10.66616952815763320, 9.056185211661334833, -16.41224021383828102 ) ) ;
#20415 = ORIENTED_EDGE ( 'NONE', *, *, #28621, .F. ) ;
#20416 = CARTESIAN_POINT ( 'NONE',  ( 27.89048517759004753, -11.43816616845083445, -12.79876095355805177 ) ) ;
#20417 = CARTESIAN_POINT ( 'NONE',  ( 167.0152310637604103, -9.999999999999998224, -0.06116980274991495881 ) ) ;
#20418 = CARTESIAN_POINT ( 'NONE',  ( 12.87053260329167692, 9.517041913610183812, -16.11361789703515868 ) ) ;
#20419 = DIRECTION ( 'NONE',  ( 0.9510565162951536422, 0.000000000000000000, -0.3090169943749475623 ) ) ;
#20420 = AXIS2_PLACEMENT_3D ( 'NONE', #6306, #10573, #16164 ) ;
#20421 = VERTEX_POINT ( 'NONE', #15110 ) ;
#20422 = DIRECTION ( 'NONE',  ( 0.5877852522924731371, 0.000000000000000000, 0.8090169943749474513 ) ) ;
#20423 = CARTESIAN_POINT ( 'NONE',  ( 130.7287565553229456, -4.999999999999982236, -13.44584919360585928 ) ) ;
#20425 = ORIENTED_EDGE ( 'NONE', *, *, #20702, .T. ) ;
#20424 = CARTESIAN_POINT ( 'NONE',  ( 424.0000000000002274, 34.64101615137744972, 10.00000000000000178 ) ) ;
#20426 = VERTEX_POINT ( 'NONE', #17259 ) ;
#20427 = LINE ( 'NONE', #3662, #6686 ) ;
#20428 = EDGE_LOOP ( 'NONE', ( #26943, #23211, #29194, #6738 ) ) ;
#20429 = CARTESIAN_POINT ( 'NONE',  ( 13.12595734265553205, 8.571888915454989544, -15.91003987120930319 ) ) ;
#20430 = CARTESIAN_POINT ( 'NONE',  ( 20.35037346166061312, -2.402462631129500092, -18.68063351227773694 ) ) ;
#20431 = CARTESIAN_POINT ( 'NONE',  ( 23.69691533927305116, -2.951365702903132604, -18.66995449711026822 ) ) ;
#20432 = CARTESIAN_POINT ( 'NONE',  ( 17.70500667399921824, 3.403337836861581867, -14.36321643528369663 ) ) ;
#20433 = LINE ( 'NONE', #10972, #4308 ) ;
#20434 = DIRECTION ( 'NONE',  ( 1.000000000000000000, 0.000000000000000000, 0.000000000000000000 ) ) ;
#20435 = AXIS2_PLACEMENT_3D ( 'NONE', #25022, #12160, #28083 ) ;
#20436 = CARTESIAN_POINT ( 'NONE',  ( 19.50856600871340873, -1.908691058934758100, -18.90332006808282728 ) ) ;
#20437 = EDGE_LOOP ( 'NONE', ( #14064, #21804, #15876, #689 ) ) ;
#20438 = VECTOR ( 'NONE', #25302, 1000.000000000000000 ) ;
#20439 = DIRECTION ( 'NONE',  ( 0.9510565162951536422, 0.000000000000000000, -0.3090169943749475623 ) ) ;
#20440 = CARTESIAN_POINT ( 'NONE',  ( 175.7287565553229456, -4.999999999999970690, 0.5000000000000029976 ) ) ;
#20441 = EDGE_CURVE ( 'NONE', #1081, #6635, #17559, .T. ) ;
#20442 = EDGE_LOOP ( 'NONE', ( #14839, #18166, #8909, #27251 ) ) ;
#20443 = EDGE_CURVE ( 'NONE', #10703, #22891, #1404, .T. ) ;
#20444 = CARTESIAN_POINT ( 'NONE',  ( 10.35864917552468611, 16.97212507441191320, -17.91611982430173455 ) ) ;
#20445 = CARTESIAN_POINT ( 'NONE',  ( 32.52799721746220740, -11.03300674309804386, -18.03857687357939099 ) ) ;
#20446 = DIRECTION ( 'NONE',  ( 1.110223024625156540E-16, 2.995891024602366092E-32, 1.000000000000000000 ) ) ;
#20447 = ORIENTED_EDGE ( 'NONE', *, *, #16442, .T. ) ;
#20448 = ORIENTED_EDGE ( 'NONE', *, *, #19860, .T. ) ;
#20449 = LINE ( 'NONE', #23060, #17305 ) ;
#20450 = CARTESIAN_POINT ( 'NONE',  ( 17.95327243003904982, 7.812726124483462264, -14.88485059575767266 ) ) ;
#20451 = CARTESIAN_POINT ( 'NONE',  ( 12.24938746628909492, 9.517981781931423413, -15.32991762565031202 ) ) ;
#20452 = CARTESIAN_POINT ( 'NONE',  ( 35.37764311538968087, -21.41652447078215005, -19.89511094362359955 ) ) ;
#20453 = VECTOR ( 'NONE', #2132, 1000.000000000000000 ) ;
#20454 = ORIENTED_EDGE ( 'NONE', *, *, #5850, .F. ) ;
#20455 = CARTESIAN_POINT ( 'NONE',  ( 0.000000000000000000, 0.000000000000000000, 23.00000000000000000 ) ) ;
#20456 = VECTOR ( 'NONE', #27557, 1000.000000000000000 ) ;
#20457 = CARTESIAN_POINT ( 'NONE',  ( 17.10490717348788081, 9.547663288818908356, -11.45998271326893381 ) ) ;
#20458 = DIRECTION ( 'NONE',  ( -2.698458740408365879E-16, 1.000000000000000000, 0.000000000000000000 ) ) ;
#20459 = FILL_AREA_STYLE ('',( #18319 ) ) ;
#20460 = AXIS2_PLACEMENT_3D ( 'NONE', #10006, #26370, #19028 ) ;
#20461 = ORIENTED_EDGE ( 'NONE', *, *, #5082, .F. ) ;
#20462 = AXIS2_PLACEMENT_3D ( 'NONE', #29905, #8913, #18229 ) ;
#20463 = CARTESIAN_POINT ( 'NONE',  ( 104.2637232758598316, -4.999999999999989342, -75.75202908809458791 ) ) ;
#20464 = ORIENTED_EDGE ( 'NONE', *, *, #16518, .F. ) ;
#20465 = CARTESIAN_POINT ( 'NONE',  ( 13.14063544215093948, 9.636405190433555035, -15.89834116682275145 ) ) ;
#20466 = CARTESIAN_POINT ( 'NONE',  ( 34.70514358766799745, -13.90287004036446739, -20.03273298744158737 ) ) ;
#20467 = CARTESIAN_POINT ( 'NONE',  ( 23.63863231746517712, -2.790269051896475450, -19.68844555248840678 ) ) ;
#20468 = ORIENTED_EDGE ( 'NONE', *, *, #9795, .T. ) ;
#20469 = DIRECTION ( 'NONE',  ( 0.3090169943749472292, 8.338696094057992503E-17, -0.9510565162951536422 ) ) ;
#20470 = DIRECTION ( 'NONE',  ( 0.000000000000000000, 0.000000000000000000, 1.000000000000000000 ) ) ;
#20471 = CIRCLE ( 'NONE', #28329, 8.000000000000003553 ) ;
#20472 = EDGE_LOOP ( 'NONE', ( #11611, #23365, #17136 ) ) ;
#20473 = FILL_AREA_STYLE_COLOUR ( '', #26342 ) ;
#20474 = CARTESIAN_POINT ( 'NONE',  ( 22.09907825138052218, -7.445301066569870230, -16.29136317631293807 ) ) ;
#20475 = VECTOR ( 'NONE', #7997, 1000.000000000000000 ) ;
#20476 = CARTESIAN_POINT ( 'NONE',  ( 28.68006932781580076, -6.484681432979621185, -16.07205306641353104 ) ) ;
#20477 = ORIENTED_EDGE ( 'NONE', *, *, #22797, .F. ) ;
#20478 = PLANE ( 'NONE',  #29396 ) ;
#20479 = AXIS2_PLACEMENT_3D ( 'NONE', #5688, #5385, #9943 ) ;
#20480 = VECTOR ( 'NONE', #2077, 1000.000000000000000 ) ;
#20481 = EDGE_CURVE ( 'NONE', #22503, #2774, #22298, .T. ) ;
#20482 = DIRECTION ( 'NONE',  ( -2.698458740408365879E-16, 1.000000000000000000, 0.000000000000000000 ) ) ;
#20483 = PLANE ( 'NONE',  #7273 ) ;
#20484 = DIRECTION ( 'NONE',  ( -0.9510565162951536422, -2.566386769018988323E-16, 0.3090169943749475623 ) ) ;
#20485 = UNCERTAINTY_MEASURE_WITH_UNIT (LENGTH_MEASURE( 1.000000000000000082E-05 ), #16538, 'distance_accuracy_value', 'NONE');
#20486 = CARTESIAN_POINT ( 'NONE',  ( 12.63667343406881294, 8.631100619704961119, -15.02124387326777111 ) ) ;
#20488 = AXIS2_PLACEMENT_3D ( 'NONE', #23778, #21019, #124 ) ;
#20487 = CARTESIAN_POINT ( 'NONE',  ( 162.0152310637604387, -9.999999999999998224, 1.702185954127501066 ) ) ;
#20489 = VERTEX_POINT ( 'NONE', #10696 ) ;
#20490 = LINE ( 'NONE', #15905, #14436 ) ;
#20491 = VERTEX_POINT ( 'NONE', #10235 ) ;
#20492 = AXIS2_PLACEMENT_3D ( 'NONE', #1649, #3777, #8639 ) ;
#20493 = CARTESIAN_POINT ( 'NONE',  ( 9.843778300897430000, 16.74053286659246709, -16.57516421589427225 ) ) ;
#20494 = CARTESIAN_POINT ( 'NONE',  ( 15.09270446591840731, 5.883488971450414162, -17.42782692652931331 ) ) ;
#20495 = CARTESIAN_POINT ( 'NONE',  ( 149.5152310637605240, -1.999999999999976241, -13.05155085951651195 ) ) ;
#20496 = LINE ( 'NONE', #25088, #11769 ) ;
#20498 = ORIENTED_EDGE ( 'NONE', *, *, #16268, .T. ) ;
#20497 = CARTESIAN_POINT ( 'NONE',  ( 24.00918528248616468, -0.5066965781341161712, -13.81223085940890627 ) ) ;
#20499 = ORIENTED_EDGE ( 'NONE', *, *, #1169, .F. ) ;
#20500 = CARTESIAN_POINT ( 'NONE',  ( 142.0152310637605808, -10.00000000000000355, -17.38167787843871182 ) ) ;
#20501 = CARTESIAN_POINT ( 'NONE',  ( 11.05541531668977662, 17.68942339022145305, -17.91752729848688830 ) ) ;
#20502 = VECTOR ( 'NONE', #16915, 1000.000000000000000 ) ;
#20503 = CARTESIAN_POINT ( 'NONE',  ( 31.77493940018505114, -11.56844746753418640, -13.90849911728625266 ) ) ;
#20504 = CARTESIAN_POINT ( 'NONE',  ( -4.000000000000003553, -6.938893903907228378E-15, 8.673617379884035472E-16 ) ) ;
#20505 = ORIENTED_EDGE ( 'NONE', *, *, #3958, .T. ) ;
#20506 = CARTESIAN_POINT ( 'NONE',  ( 21.57856661146780652, -4.666631351218505586, -18.28211233923166645 ) ) ;
#20507 = DIRECTION ( 'NONE',  ( 1.000000000000000000, 4.440892098500622217E-16, 0.000000000000000000 ) ) ;
#20508 = CARTESIAN_POINT ( 'NONE',  ( 24.07691212630517796, -1.086650970500502300, -17.53382830850624785 ) ) ;
#20509 = ORIENTED_EDGE ( 'NONE', *, *, #12547, .T. ) ;
#20510 = CARTESIAN_POINT ( 'NONE',  ( -1.310841663519413114, 7.511012776518212944E-16, -5.000000000000000888 ) ) ;
#20511 = EDGE_CURVE ( 'NONE', #2212, #2121, #22141, .T. ) ;
#20512 = CARTESIAN_POINT ( 'NONE',  ( 27.50131297508284334, -11.63919202702402167, -19.74788458503752864 ) ) ;
#20513 = CARTESIAN_POINT ( 'NONE',  ( 30.28771073495105881, -9.259452824753982014, -16.33981616121770131 ) ) ;
#20514 = ORIENTED_EDGE ( 'NONE', *, *, #13312, .T. ) ;
#20515 = ORIENTED_EDGE ( 'NONE', *, *, #7872, .F. ) ;
#20516 = DIRECTION ( 'NONE',  ( 2.908569913943825554E-16, -1.000000000000000000, 0.000000000000000000 ) ) ;
#20517 = CARTESIAN_POINT ( 'NONE',  ( 171.1922820468852819, -4.999999999999970690, -2.083034168790677043 ) ) ;
#20518 =( GEOMETRIC_REPRESENTATION_CONTEXT ( 3 ) GLOBAL_UNCERTAINTY_ASSIGNED_CONTEXT ( ( #14354 ) ) GLOBAL_UNIT_ASSIGNED_CONTEXT ( ( #8465, #6789, #30040 ) ) REPRESENTATION_CONTEXT ( 'NONE', 'WORKASPACE' ) );
#20519 = DIRECTION ( 'NONE',  ( 0.5877852522924731371, 1.586114251531760728E-16, 0.8090169943749474513 ) ) ;
#20520 = CARTESIAN_POINT ( 'NONE',  ( 173.6922820468852819, -1.999999999999970468, -6.413161187712876909 ) ) ;
#20521 = LINE ( 'NONE', #18231, #5095 ) ;
#20522 = DIRECTION ( 'NONE',  ( 0.3090169943749472292, 8.338696094057992503E-17, -0.9510565162951536422 ) ) ;
#20523 = CARTESIAN_POINT ( 'NONE',  ( 24.24519292511275737, -8.489478586693508078, -18.02380513063773648 ) ) ;
#20524 = CARTESIAN_POINT ( 'NONE',  ( 17.90640022563237110, 0.6078909361919438981, -17.24624654394265377 ) ) ;
#20526 = ORIENTED_EDGE ( 'NONE', *, *, #29365, .T. ) ;
#20525 = CARTESIAN_POINT ( 'NONE',  ( 35.54910479118309041, -18.69434066908399217, -21.33016376092627553 ) ) ;
#20527 = DIRECTION ( 'NONE',  ( 0.5877852522924731371, 1.586114251531760728E-16, -0.8090169943749474513 ) ) ;
#20528 = CARTESIAN_POINT ( 'NONE',  ( 12.50140887008201851, 8.571324787501421127, -15.12905211845398412 ) ) ;
#20529 = CARTESIAN_POINT ( 'NONE',  ( 149.7287565553229456, -4.999999999999976907, 0.8205080756888000204 ) ) ;
#20530 = DIRECTION ( 'NONE',  ( -0.8090169943749474513, -2.183098979609982436E-16, -0.5877852522924731371 ) ) ;
#20531 = CARTESIAN_POINT ( 'NONE',  ( 9.668122305056073174, 16.22621266786625327, -17.88497096177859191 ) ) ;
#20532 = CARTESIAN_POINT ( 'NONE',  ( -4.683753385137379155E-14, -9.237604307034027684, -4.285468820183664818 ) ) ;
#20533 = ORIENTED_EDGE ( 'NONE', *, *, #22360, .F. ) ;
#20534 = CARTESIAN_POINT ( 'NONE',  ( 149.5152310637605240, -10.00000000000000178, -13.05155085951651195 ) ) ;
#20535 = CARTESIAN_POINT ( 'NONE',  ( 12.56861602585598980, 8.601024833420110483, -15.07548682890769243 ) ) ;
#20536 = ORIENTED_EDGE ( 'NONE', *, *, #24043, .F. ) ;
#20537 = CARTESIAN_POINT ( 'NONE',  ( 172.0152310637604671, -1.999999999999970024, -15.61832212156129707 ) ) ;
#20538 = LINE ( 'NONE', #29626, #9285 ) ;
#20539 = VERTEX_POINT ( 'NONE', #20007 ) ;
#20540 = CARTESIAN_POINT ( 'NONE',  ( 13.77718166750866224, 8.859676595473322536, -15.39100258941132715 ) ) ;
#20541 = ORIENTED_EDGE ( 'NONE', *, *, #23769, .F. ) ;
#20542 = CARTESIAN_POINT ( 'NONE',  ( 9.177416647856844634, 15.88379569257361190, -17.02789189981719176 ) ) ;
#20543 = CARTESIAN_POINT ( 'NONE',  ( 33.31547190024930671, -13.15228156363260581, -20.72525089784059560 ) ) ;
#20544 = EDGE_CURVE ( 'NONE', #1647, #19572, #12679, .T. ) ;
#20545 = ADVANCED_FACE ( 'NONE', ( #6276 ), #19547, .F. ) ;
#20546 = CARTESIAN_POINT ( 'NONE',  ( 20.23665759668125474, 8.554704514664523529, -15.35188933034790182 ) ) ;
#20547 = ADVANCED_FACE ( 'NONE', ( #29529 ), #8399, .T. ) ;
#20548 = CARTESIAN_POINT ( 'NONE',  ( 16.66981565813235733, 9.362922448895053762, -13.87743608138566920 ) ) ;
#20549 = ADVANCED_FACE ( 'NONE', ( #10534 ), #27064, .T. ) ;
#20550 = LINE ( 'NONE', #13381, #8887 ) ;
#20551 = CARTESIAN_POINT ( 'NONE',  ( 27.27607810006200140, -2.061267822988343656, -14.60586277656102006 ) ) ;
#20552 = ORIENTED_EDGE ( 'NONE', *, *, #19821, .T. ) ;
#20553 = DIRECTION ( 'NONE',  ( 0.9510565162951536422, 0.000000000000000000, -0.3090169943749475623 ) ) ;
#20555 = ORIENTED_EDGE ( 'NONE', *, *, #18156, .F. ) ;
#20554 = SURFACE_STYLE_USAGE ( .BOTH. , #13689 ) ;
#20556 = DIRECTION ( 'NONE',  ( 1.000000000000000000, 0.000000000000000000, 0.000000000000000000 ) ) ;
#20557 = LINE ( 'NONE', #4100, #28310 ) ;
#20558 = ORIENTED_EDGE ( 'NONE', *, *, #22803, .T. ) ;
#20559 = CARTESIAN_POINT ( 'NONE',  ( 33.81279548071420038, -11.10283711904122050, -17.43625070980107594 ) ) ;
#20560 = ORIENTED_EDGE ( 'NONE', *, *, #6232, .F. ) ;
#20561 = CARTESIAN_POINT ( 'NONE',  ( 12.49426214472998176, 7.541115143590324088, -15.13238550383361769 ) ) ;
#20562 = PRODUCT_DEFINITION_SHAPE ( 'NONE', 'NONE',  #30269 ) ;
#20563 = ORIENTED_EDGE ( 'NONE', *, *, #12031, .T. ) ;
#20564 = AXIS2_PLACEMENT_3D ( 'NONE', #19724, #15140, #3567 ) ;
#20565 = CARTESIAN_POINT ( 'NONE',  ( 29.88803641097454999, -7.968445601786871002, -16.75847372370488131 ) ) ;
#20566 = CARTESIAN_POINT ( 'NONE',  ( 2.000000000000026201, 3.464101615137736623, 8.673617379884035472E-16 ) ) ;
#20567 = CARTESIAN_POINT ( 'NONE',  ( 10.48212431696843439, 16.40585233633115436, -17.33062619162406293 ) ) ;
#20568 = PLANE ( 'NONE',  #6816 ) ;
#20569 = LINE ( 'NONE', #25597, #10574 ) ;
#20570 = ORIENTED_EDGE ( 'NONE', *, *, #9718, .F. ) ;
#20571 = LINE ( 'NONE', #27941, #24175 ) ;
#20572 = CARTESIAN_POINT ( 'NONE',  ( 13.04501788334644630, 8.811555337407297017, -14.69578613943112799 ) ) ;
#20574 = ORIENTED_EDGE ( 'NONE', *, *, #12858, .T. ) ;
#20573 = CIRCLE ( 'NONE', #12276, 4.000000000000003553 ) ;
#20575 = ORIENTED_EDGE ( 'NONE', *, *, #303, .F. ) ;
#20576 = DIRECTION ( 'NONE',  ( -2.698458740408365879E-16, 1.000000000000000000, -0.000000000000000000 ) ) ;
#20577 = ORIENTED_EDGE ( 'NONE', *, *, #24705, .F. ) ;
#20578 = CARTESIAN_POINT ( 'NONE',  ( 9.661883061612440926, 16.25482663361732705, -17.92279151347708677 ) ) ;
#20579 = EDGE_CURVE ( 'NONE', #26897, #6453, #12828, .T. ) ;
#20580 = CARTESIAN_POINT ( 'NONE',  ( 24.36273546358933828, 1.710929640254579720, -17.54733717687237160 ) ) ;
#20581 = CARTESIAN_POINT ( 'NONE',  ( 22.87531825017061848, 1.851759407679815173, -13.77476424085121742 ) ) ;
#20582 = ORIENTED_EDGE ( 'NONE', *, *, #17215, .T. ) ;
#20583 = ADVANCED_FACE ( 'NONE', ( #15417 ), #24751, .T. ) ;
#20584 = CARTESIAN_POINT ( 'NONE',  ( 20.55949567978923298, 1.660703385868308235, -14.27713627412184039 ) ) ;
#20585 = DIRECTION ( 'NONE',  ( -2.698458740408365879E-16, 1.000000000000000000, 0.000000000000000000 ) ) ;
#20586 = ADVANCED_FACE ( 'NONE', ( #13288 ), #22461, .T. ) ;
#20587 = LINE ( 'NONE', #6716, #16685 ) ;
#20588 = CARTESIAN_POINT ( 'NONE',  ( 23.16390915794477223, 2.882539813099532555, -14.99485278278146438 ) ) ;
#20589 = CIRCLE ( 'NONE', #10830, 4.000000000000003553 ) ;
#20590 = DIRECTION ( 'NONE',  ( 1.110223024625156540E-16, 2.995891024602366092E-32, 1.000000000000000000 ) ) ;
#20591 = DIRECTION ( 'NONE',  ( -2.698458740408365879E-16, 1.000000000000000000, 0.000000000000000000 ) ) ;
#20592 = CIRCLE ( 'NONE', #25005, 2.055000000000000160 ) ;
#20593 = CARTESIAN_POINT ( 'NONE',  ( 10.36007019289729847, 16.96560810760319882, -17.82599398985513872 ) ) ;
#20594 = DIRECTION ( 'NONE',  ( -0.000000000000000000, 0.000000000000000000, 1.000000000000000000 ) ) ;
#20595 = PLANE ( 'NONE',  #5826 ) ;
#20596 = EDGE_LOOP ( 'NONE', ( #10612, #12500, #29120, #28884 ) ) ;
#20597 = ORIENTED_EDGE ( 'NONE', *, *, #21683, .F. ) ;
#20598 = LINE ( 'NONE', #15721, #12927 ) ;
#20599 = CARTESIAN_POINT ( 'NONE',  ( 19.51440197245297270, 8.071880087464508691, -17.28625796899888201 ) ) ;
#20600 = CARTESIAN_POINT ( 'NONE',  ( 11.53546837550287130, 15.48783886997274450, -16.67730506581143501 ) ) ;
#20601 = CARTESIAN_POINT ( 'NONE',  ( 35.54859390953724585, -22.18451583373416014, -16.94733705004010460 ) ) ;
#20602 = ORIENTED_EDGE ( 'NONE', *, *, #27691, .T. ) ;
#20603 = ORIENTED_EDGE ( 'NONE', *, *, #15589, .T. ) ;
#20604 = PLANE ( 'NONE',  #12184 ) ;
#20605 = CARTESIAN_POINT ( 'NONE',  ( 9.641404825192898542, 17.66864342279195199, -17.88841768828662282 ) ) ;
#20606 = CARTESIAN_POINT ( 'NONE',  ( 148.6922820468854525, -10.00000000000000178, -23.73366926340167637 ) ) ;
#20607 = DIRECTION ( 'NONE',  ( 0.000000000000000000, 0.000000000000000000, 1.000000000000000000 ) ) ;
#20608 = EDGE_LOOP ( 'NONE', ( #13467, #23947, #18219, #12388 ) ) ;
#20609 = PLANE ( 'NONE',  #5682 ) ;
#20610 = EDGE_LOOP ( 'NONE', ( #24383, #27874, #10060, #23628 ) ) ;
#20611 = CARTESIAN_POINT ( 'NONE',  ( 12.87180867969543385, 9.517605834602926862, -16.11260084161717998 ) ) ;
#20612 = CARTESIAN_POINT ( 'NONE',  ( 35.77509030908504428, -18.70957389315904962, -20.35615221346758474 ) ) ;
#20613 = CARTESIAN_POINT ( 'NONE',  ( 23.84106988684860440, -4.080291168153947545, -13.50610408985603250 ) ) ;
#20614 = ORIENTED_EDGE ( 'NONE', *, *, #10654, .T. ) ;
#20615 = EDGE_CURVE ( 'NONE', #26545, #16077, #5674, .T. ) ;
#20616 = ORIENTED_EDGE ( 'NONE', *, *, #8201, .F. ) ;
#20617 = EDGE_CURVE ( 'NONE', #12856, #27966, #1107, .T. ) ;
#20618 = FACE_OUTER_BOUND ( 'NONE', #15093, .T. ) ;
#20619 = VERTEX_POINT ( 'NONE', #5972 ) ;
#20620 = VECTOR ( 'NONE', #21343, 1000.000000000000000 ) ;
#20621 = EDGE_CURVE ( 'NONE', #7269, #8000, #4649, .T. ) ;
#20622 = EDGE_CURVE ( 'NONE', #18644, #20136, #19694, .T. ) ;
#20623 = DIRECTION ( 'NONE',  ( -2.698458740408365879E-16, 1.000000000000000000, 0.000000000000000000 ) ) ;
#20624 = SURFACE_SIDE_STYLE ('',( #4007 ) ) ;
#20625 = CARTESIAN_POINT ( 'NONE',  ( 24.97892660363778106, -6.291154998746494087, -12.74939059104742256 ) ) ;
#20626 = CARTESIAN_POINT ( 'NONE',  ( 28.66609726738115071, -6.663921799113727396, -16.65640135049372006 ) ) ;
#20627 = ORIENTED_EDGE ( 'NONE', *, *, #19646, .F. ) ;
#20628 = DIRECTION ( 'NONE',  ( 0.5877852522924731371, 0.000000000000000000, 0.8090169943749474513 ) ) ;
#20629 = DIRECTION ( 'NONE',  ( -0.9510565162951536422, -2.566386769018988323E-16, 0.3090169943749475623 ) ) ;
#20630 = LINE ( 'NONE', #24937, #17028 ) ;
#20631 = FACE_OUTER_BOUND ( 'NONE', #14289, .T. ) ;
#20632 = AXIS2_PLACEMENT_3D ( 'NONE', #12557, #14694, #677 ) ;
#20633 = CARTESIAN_POINT ( 'NONE',  ( 14.38576730248667701, 9.404056492746565965, -13.62718518646353161 ) ) ;
#20634 = CARTESIAN_POINT ( 'NONE',  ( 30.76698452600511402, -8.440788201038053273, -16.67119366161266925 ) ) ;
#20635 = FACE_BOUND ( 'NONE', #14384, .T. ) ;
#20636 = ORIENTED_EDGE ( 'NONE', *, *, #10381, .F. ) ;
#20637 = CARTESIAN_POINT ( 'NONE',  ( 9.641485839925177714, 17.66827187890266160, -17.87200850766020110 ) ) ;
#20638 = CARTESIAN_POINT ( 'NONE',  ( 15.41580380672748163, 5.935325531760808460, -16.22756139702874023 ) ) ;
#20639 = DIRECTION ( 'NONE',  ( 0.3090169943749475623, 8.338696094058001131E-17, 0.9510565162951536422 ) ) ;
#20640 = CARTESIAN_POINT ( 'NONE',  ( 49.00000000000000000, 0.000000000000000000, 0.000000000000000000 ) ) ;
#20642 = ORIENTED_EDGE ( 'NONE', *, *, #15294, .T. ) ;
#20641 = CARTESIAN_POINT ( 'NONE',  ( 24.95482030053459965, -6.624749414579512496, -13.76522253407564733 ) ) ;
#20643 = CARTESIAN_POINT ( 'NONE',  ( 104.0883501548822636, -4.999999999999989342, 75.62461305743535434 ) ) ;
#20644 = CARTESIAN_POINT ( 'NONE',  ( 12.25660130062383146, 9.517454774955181662, -15.32445140518387028 ) ) ;
#20645 = CARTESIAN_POINT ( 'NONE',  ( 35.54859569580823830, -22.18452385850428499, -18.27063337037174762 ) ) ;
#20646 = CARTESIAN_POINT ( 'NONE',  ( 15.87806330829146617, 7.947701475055697351, -19.83831759000646855 ) ) ;
#20647 = EDGE_CURVE ( 'NONE', #19412, #14559, #3683, .T. ) ;
#20648 = CARTESIAN_POINT ( 'NONE',  ( 26.47492910780048447, -3.130564378024159211, -15.09640780237150892 ) ) ;
#20649 = CARTESIAN_POINT ( 'NONE',  ( 172.7287565553229456, -4.999999999999971578, -36.50000000000000711 ) ) ;
#20650 = CARTESIAN_POINT ( 'NONE',  ( 21.43024726678804726, -3.720057188146618010, -16.74626013867020902 ) ) ;
#20651 = EDGE_CURVE ( 'NONE', #11863, #19198, #2015, .T. ) ;
#20652 = ORIENTED_EDGE ( 'NONE', *, *, #779, .F. ) ;
#20653 = EDGE_CURVE ( 'NONE', #11084, #19168, #1703, .T. ) ;
#20654 = PLANE ( 'NONE',  #23743 ) ;
#20655 =( BOUNDED_SURFACE ( )  B_SPLINE_SURFACE ( 3, 3, ( 
 ( #20952, #16683, #64, #9348, #11344, #28334, #28019, #11791, #16375, #4786, #9494, #14076, #23405, #5085, #21257, #14373, #2522, #9655, #7388, #23711, #20646, #30033, #9041, #27721, #19710, #26309, #21565, #12097, #664, #3266, #9949, #810, #12393, #17134, #7969, #26461, #21860, #5392, #23870, #28476, #7524, #21705, #14973, #19565, #28933, #17277, #26613, #17423, #14528, #12541, #12247, #19262, #28784, #5541, #5694, #2971, #14826, #24161, #28620, #24309, #3405, #7675, #12697, #3121, #10253, #22017, #1125, #19120, #26160, #10102, #19415, #16983, #7827, #10403, #29076, #970, #24021, #14678, #2813, #8118, #26772, #5842, #15129, #21413, #519, #9808, #16828, #5234, #22620, #18180, #8564, #8713, #24608, #29390, #8416, #26929, #5988, #18028, #11162, #17721, #13001, #3554, #22313, #24922, #1422, #22476, #3854, #17864, #29699, #27240, #13301, #27080, #15276, #19864, #29228, #13151, #6447, #11006, #20310, #27395, #15736, #8862, #3700, #4002, #10711, #20022, #20163, #6290, #25063, #6139, #15586, #1721, #15435, #4150, #13447, #24765, #22775, #1573, #1881, #20467, #29857, #10555, #17574, #10852, #29545, #27538, #6592, #24458, #12846, #22158, #1268, #8264, #18938, #20613, #18326, #30001, #16338, #6904, #18786, #13748, #9317, #9006, #27684, #28294, #23217, #23520, #23076, #16193, #4898, #21220, #25656, #28140, #4748, #14194, #30148, #27840, #4602, #16036, #6744, #11451, #335, #11310, #25361, #2629, #4457, #2175, #9620, #7047, #25817, #25511, #20760, #25215, #4303, #13602, #21075, #11904, #183, #14039, #22930, #11759, #9155, #20915, #13890, #15882, #2032, #11601, #29, #18484, #2332, #23368, #9462, #18641, #27987, #7197, #2484, #16491, #481, #23832, #12661, #2930, #9916, #19379, #14495, #9770, #21668, #19227, #28901, #14940, #5201, #7638, #12504, #19088, #28439, #21979, #12210, #21530, #1092, #16796, #631, #26574, #19674, #28584, #28743, #770, #21373, #24275 ),
 ( #17098, #5047, #3226, #7491, #12355, #16945, #10369, #26274, #26123, #7348, #3374, #5356, #7789, #10067, #14642, #26423, #23989, #3086, #16649, #5503, #25966, #14788, #21827, #24128, #927, #10219, #19530, #7932, #17243, #14338, #5658, #23674, #2778, #12060, #29512, #26895, #27049, #8384, #13114, #3972, #22440, #17834, #1387, #19829, #24426, #3521, #17690, #10970, #15552, #24887, #13271, #22588, #13414, #10515, #8533, #8229, #15247, #24732, #1540, #1689, #29192, #10823, #20134, #5959, #20279, #29666, #17539, #8681, #29358, #6257, #17987, #27359, #15090, #22127, #6104, #15398, #24579, #3820, #3667, #27206, #6415, #15704, #12963, #25033, #4119, #22278, #22739, #1852, #10678, #11130, #29039, #8079, #17388, #26733, #12814, #1231, #5805, #19987, #20581, #2143, #30259, #9271, #25471, #11417, #13998, #21035, #15848, #4269, #25178, #4562, #4421, #18599, #29966, #18450, #13569, #6557, #141, #20722, #4705, #8973, #13715, #16296, #23327, #13851, #27950, #23177, #25609, #6713, #25330, #30109, #1997, #22895, #18288, #2440, #11276, #27645, #11718, #16001, #23041, #20431, #2289, #29823, #9119, #27799, #18144, #27506, #6866, #7007, #8831, #16153, #11560, #20877, #13357, #17634, #22537, #27138, #22833, #8477, #26989, #17485, #25119, #8331, #17925, #1635, #17778, #27301, #3913, #13056, #1938, #15648, #11220, #10914, #1783, #6047, #22379, #1484, #19928, #29294, #11068, #4209, #10774, #15336, #26834, #24673, #6355, #3763, #15494, #6201, #20223, #22682, #29609, #24981, #20083, #29459, #12904, #22218, #24825, #29762, #4064, #20372, #8771, #18086, #20523, #13213, #27448, #8625, #6501, #15792, #13506, #29910, #5905, #15187, #24519, #3612, #1327, #10618, #9534, #9847, #23754, #4820, #28220, #17025, #28061, #14117, #704, #23447, #18858, #26351, #2851, #12286, #2695, #2559, #11679, #20994, #104, #7565, #9989, #16871, #12137, #9387, #28517, #11832, #7425, #11978, #7716, #23598 ),
 ( #18713, #5430, #4973, #28667, #21145, #21298, #9690, #256, #26200, #3009, #5278, #21454, #26046, #23915, #7270, #7114, #14565, #16573, #562, #19160, #16418, #21606, #19305, #25737, #25896, #14264, #14717, #405, #16725, #19015, #2404, #28370, #5123, #14414, #8310, #13043, #29437, #29119, #29274, #21751, #10295, #3593, #17466, #22359, #7863, #1464, #24649, #19603, #22059, #19456, #17615, #28826, #26975, #19910, #6032, #6181, #15317, #24505, #17173, #10755, #5736, #3308, #26502, #8460, #19750, #8160, #17764, #27119, #12885, #3743, #24349, #24059, #20062, #26814, #28973, #5583, #8010, #3160, #17316, #26657, #5889, #15170, #14865, #12432, #854, #10144, #12584, #21903, #10442, #1311, #24205, #1018, #15019, #3449, #12738, #1161, #22199, #10599, #13339, #4492, #9044, #22815, #27574, #18367, #20354, #20802, #13783, #22517, #30187, #18069, #11487, #6334, #25100, #1919, #4043, #30037, #16073, #11347, #25255, #8901, #6786, #15629, #20209, #27723, #22662, #4339, #22966, #29587, #23110, #13637, #8605, #24963, #1766, #2216, #17905, #20508, #27284, #25401, #11052, #9197, #1617, #18524, #27880, #15476, #29893, #20650, #13195, #29744, #2068, #18218, #24809, #8750, #3896, #10895, #27430, #13488, #6485, #15774, #4190, #11197, #6629, #15922, #19266, #21417, #7391, #20955, #26163, #18820, #16377, #68, #21568, #2661, #21259, #666, #9951, #26010, #12100, #7237, #6937, #523, #11940, #2525, #9351, #23407, #12250, #11796, #9498, #18979, #14078, #18676, #371, #28179, #28481, #14531, #4788, #16535, #9811, #4637, #28024, #5090, #25543, #21113, #16230, #25699, #219, #5239, #13927, #25859, #14377, #28337, #7082, #4937, #23259, #2370, #14229, #23874, #23563, #9658, #11643, #16687, #16834, #23714, #2817, #19124, #7527, #2974, #3558, #5993, #12850, #8122, #26311, #24462, #28786, #3409, #7973, #3705, #19569, #7830, #28624, #15280, #19418, #29082, #12700, #28937, #17427, #14978 ),
 ( #29233, #22163, #26775, #22021, #19868, #17138, #3123, #10561, #5548, #5845, #15133, #12396, #17578, #1272, #21708, #26466, #14829, #26936, #812, #1128, #10108, #8268, #24167, #24612, #14682, #13003, #22320, #1853, #10407, #11131, #5395, #3269, #7679, #19713, #16985, #12545, #24025, #21865, #973, #26617, #10256, #17281, #5697, #24313, #16298, #25613, #2591, #4707, #20878, #4271, #9421, #2146, #29967, #13571, #4855, #16154, #4564, #14156, #23484, #9272, #13999, #20724, #20432, #23328, #25473, #16002, #22896, #6714, #25777, #25331, #23043, #2290, #27646, #1998, #13855, #11418, #11719, #28094, #18289, #30111, #2442, #18146, #11277, #25179, #18747, #6559, #21037, #7158, #29825, #23178, #143, #27507, #4422, #30261, #11562, #16454, #20584, #8834, #15849, #13716, #18451, #8974, #9120, #27800, #6867, #18601, #27951, #7008, #26390, #12317, #25930, #893, #23793, #21335, #5012, #26540, #7600, #26236, #5620, #14900, #730, #14301, #23636, #21633, #2891, #14754, #9727, #5316, #16609, #2734, #24241, #19192, #19495, #19049, #12173, #10184, #17212, #10027, #24092, #19341, #28866, #7901, #28405, #28705, #3045, #12017, #7458, #11867, #7304, #443, #21180, #16762, #26084, #291, #7753, #21793, #21491, #5164, #9574, #18899, #28254, #17062, #14454, #5469, #3193, #595, #12470, #9880, #16905, #28548, #14600, #23955, #3489, #3342, #10936, #24390, #3786, #8352, #24544, #13081, #19951, #29154, #17949, #1508, #27326, #17655, #17800, #12777, #8195, #17505, #5773, #15054, #27163, #20246, #26859, #22094, #12624, #1199, #22403, #10481, #1352, #12924, #27016, #8501, #6071, #10796, #5926, #19789, #29007, #8044, #15211, #22559, #6222, #10641, #15357, #15519, #3631, #8645, #1658, #10332, #6381, #22243, #29633, #29320, #24696, #20103, #29482, #24850, #3937, #13239, #15670, #21943, #1056, #19640, #17353, #26698, #1960, #4530, #2257, #8797, #13966, #13821, #29784, #25141, #11242, #23296 ),
 ( #11529, #20842, #9391, #6525, #25439, #4233, #20548, #20691, #9089, #9234, #13532, #18413, #27765, #29934, #30225, #18566, #22858, #27917, #25295, #6976, #16264, #2410, #11092, #18109, #4383, #2112, #8941, #23007, #25579, #4675, #23146, #15966, #18717, #11684, #13683, #27471, #15815, #21001, #11386, #109, #18257, #6830, #27613, #6675, #7122, #30077, #28065, #16120, #25003, #4086, #13379, #22705, #1811, #20394, #5439, #3165, #23603, #23921, #7570, #18866, #11983, #859, #11837, #28224, #14722, #7275, #2699, #10149, #16876, #26356, #16730, #16577, #25742, #4826, #14122, #21610, #24064, #708, #26204, #23454, #12291, #25902, #21458, #26051, #21759, #21302, #14419, #21149, #9994, #260, #19311, #28672, #7720, #28830, #17030, #5282, #9539, #12436, #28377, #4978, #14269, #19462, #12145, #568, #5130, #16423, #19164, #9852, #23758, #2563, #412, #28521, #9695, #19020, #7429, #2855, #14570, #3015, #19916, #15023, #10302, #22206, #10449, #29444, #15483, #5740, #8164, #13047, #5589, #1023, #26980, #26507, #22064, #13201, #17322, #24355, #27125, #20213, #29125, #29279, #1316, #21909, #24813, #14870, #22366, #26663, #3453, #24510, #15323, #7869, #10759, #12745, #1165, #8467, #17769, #6187, #17181, #19755, #3902, #1469, #15175, #8315, #20067, #17470, #22524, #1622, #24211, #10900, #26820, #3312, #28980, #5893, #3597, #12890, #12589, #19609, #3750, #17620, #10606, #8014, #6038, #24655, #11493, #6489, #9048, #6791, #13343, #18531, #18373, #4049, #29749, #15779, #27885, #1771, #4344, #11057, #20807, #22667, #6942, #15636, #13788, #16234, #4642, #13643, #4497, #27290, #25104, #27729, #22971, #25548, #20358, #13933, #30192, #16080, #6339, #25405, #8758, #2075, #8908, #23265, #20513, #18074, #29594, #2374, #27436, #30042, #11352, #29898, #23114, #15927, #4194, #11647, #2223, #8611, #20657, #9201, #13493, #22821, #1924, #11203, #18224, #17910, #24970, #27578, #6633, #25259 ),
 ( #14382, #9816, #23567, #11800, #16382, #25708, #377, #2980, #7534, #16838, #26168, #5244, #5401, #2529, #21421, #224, #7243, #16693, #5094, #14536, #21117, #23719, #2822, #28186, #23881, #12256, #9502, #21573, #21263, #28485, #671, #19273, #7087, #14082, #9663, #28342, #18826, #18986, #9956, #28628, #531, #11944, #14687, #7684, #7395, #23413, #4792, #19128, #26017, #16991, #16540, #12107, #25864, #4942, #3127, #26316, #24031, #14234, #20962, #74, #9355, #18681, #28029, #2665, #1430, #29404, #19575, #19873, #3564, #14833, #7978, #27087, #7834, #24171, #10718, #3273, #28942, #6148, #12855, #22327, #12705, #12551, #21713, #818, #10113, #17586, #20029, #26941, #19718, #24468, #15285, #17288, #17728, #8427, #19424, #15444, #14984, #24774, #21871, #22026, #29089, #980, #5997, #13007, #8273, #22169, #5851, #3712, #10262, #17143, #24616, #26623, #1276, #29238, #26471, #12400, #10568, #5555, #5701, #24321, #28790, #3414, #17431, #1132, #10413, #8127, #26781, #15138, #18333, #23083, #9166, #8873, #9011, #1583, #20318, #13607, #27544, #2187, #17870, #11455, #4462, #29708, #1889, #29554, #27694, #8571, #6753, #30005, #16043, #16200, #25369, #4309, #27250, #20766, #15743, #13307, #6298, #18493, #29863, #18187, #4157, #3865, #6597, #15892, #13453, #27848, #13753, #25223, #8720, #15596, #18034, #6909, #27402, #6452, #22938, #11014, #24929, #2039, #25068, #30155, #13159, #1731, #22781, #22483, #10864, #4009, #11314, #20173, #11169, #22629, #20476, #20626, #14501, #7649, #16499, #7356, #9625, #9323, #2936, #2338, #493, #14046, #4755, #11909, #2784, #25517, #28446, #23374, #190, #16801, #26132, #5209, #4608, #2496, #23840, #19093, #5055, #18948, #12222, #25667, #39, #7501, #11766, #14344, #12066, #18648, #21536, #23681, #27994, #21083, #9470, #637, #7054, #341, #16343, #9924, #18792, #19237, #11609, #9779, #28594, #13899, #28300, #23224, #20925, #28148 ),
 ( #7206, #25824, #4905, #14204, #23529, #21382, #2634, #21226, #16655, #25977, #17253, #24284, #5516, #14946, #10526, #19834, #26739, #7939, #1392, #17548, #26582, #19386, #780, #17393, #5665, #29197, #14796, #10376, #21676, #10072, #29366, #3380, #24583, #24135, #12669, #5963, #22285, #5816, #8234, #15099, #15252, #3672, #3235, #24434, #8086, #28755, #12514, #10683, #12364, #7799, #12970, #17106, #21834, #19993, #3526, #26903, #21988, #26431, #26281, #5365, #14649, #22132, #16952, #1238, #12819, #23999, #3094, #940, #1099, #19682, #10226, #29049, #19540, #28908, #16008, #29519, #8839, #13417, #29671, #18149, #25037, #3977, #23046, #6564, #2150, #22745, #22900, #8537, #13274, #22593, #1693, #6421, #3827, #2001, #13120, #11282, #4275, #13574, #20728, #20588, #27510, #22445, #27654, #20284, #17839, #1547, #11422, #4125, #1857, #8684, #8389, #11135, #20436, #17993, #17693, #29970, #29828, #10977, #10829, #24892, #13720, #27366, #15708, #15855, #15558, #20138, #25185, #8978, #18294, #25335, #6262, #6717, #4425, #6109, #27212, #27054, #15404, #24737, #5590, #9278, #16303, #19465, #12595, #21043, #11871, #14161, #13861, #7873, #6871, #5016, #18605, #27955, #16458, #7310, #30117, #2738, #7012, #4713, #21339, #448, #9733, #9127, #25620, #28831, #23641, #7165, #21185, #12023, #14003, #14871, #17183, #16159, #24214, #2450, #26510, #20884, #9425, #25781, #23332, #14306, #3313, #25935, #9580, #23488, #18455, #21918, #4568, #27807, #11723, #18905, #16613, #23182, #25478, #28258, #2296, #147, #18752, #11566, #28099, #4861, #2597, #296, #26666, #10908, #8017, #6192, #20215, #27292, #26981, #27128, #19613, #8165, #1473, #15325, #29599, #5743, #8614, #22527, #6345, #10762, #3905, #20069, #17915, #15639, #29127, #29451, #13048, #24362, #17472, #24972, #17323, #3456, #4053, #12746, #26822, #21911, #22369, #1625, #22209, #22066, #1025, #10303, #28983, #15485, #15025, #24816 ) ),
 .UNSPECIFIED., .T., .F., .F. ) 
 B_SPLINE_SURFACE_WITH_KNOTS ( ( 4, 3, 4 ),
 ( 4, 2, 2, 2, 2, 2, 2, 2, 2, 2, 2, 2, 2, 2, 2, 2, 2, 2, 2, 2, 2, 2, 2, 2, 2, 2, 2, 2, 2, 2, 2, 2, 2, 2, 2, 2, 2, 2, 2, 2, 2, 2, 2, 2, 2, 2, 2, 2, 2, 2, 2, 2, 2, 2, 2, 2, 2, 2, 2, 2, 2, 2, 2, 2, 2, 2, 2, 2, 2, 2, 2, 2, 2, 2, 2, 2, 2, 2, 2, 2, 2, 2, 2, 2, 2, 2, 2, 2, 2, 2, 2, 2, 2, 2, 2, 2, 2, 2, 2, 2, 2, 2, 2, 2, 2, 2, 2, 2, 2, 2, 2, 2, 2, 2, 2, 2, 2, 2, 2, 2, 2, 2, 4 ),
 ( 0.000000000000000000, 0.5000000000000000000, 1.000000000000000000 ),
 ( 0.000000000000000000, 0.007812500000000000000, 0.01464843750000000000, 0.02148437500000000000, 0.02832031250000000000, 0.03515625000000000000, 0.04882812500000000000, 0.05566406250000000000, 0.06250000000000000000, 0.06933593750000000000, 0.07617187500000000000, 0.08984375000000000000, 0.09667968750000000000, 0.1035156250000000000, 0.1103515625000000000, 0.1171875000000000000, 0.1240234375000000000, 0.1308593750000000000, 0.1376953125000000000, 0.1445312500000000000, 0.1513671875000000000, 0.1582031250000000000, 0.1718750000000000000, 0.1787109375000000000, 0.1855468750000000000, 0.1992187500000000000, 0.2060546875000000000, 0.2128906250000000000, 0.2197265625000000000, 0.2265625000000000000, 0.2402343750000000000, 0.2470703125000000000, 0.2539062500000000000, 0.2607421875000000000, 0.2675781250000000000, 0.2812500000000000000, 0.2880859375000000000, 0.2949218750000000000, 0.3017578125000000000, 0.3085937500000000000, 0.3154296875000000000, 0.3222656250000000000, 0.3291015625000000000, 0.3359375000000000000, 0.3496093750000000000, 0.3564453125000000000, 0.3632812500000000000, 0.3701171875000000000, 0.3769531250000000000, 0.3906250000000000000, 0.3974609375000000000, 0.4042968750000000000, 0.4179687500000000000, 0.4316406250000000000, 0.4384765625000000000, 0.4453125000000000000, 0.4521484375000000000, 0.4589843750000000000, 0.4658203125000000000, 0.4726562500000000000, 0.4794921875000000000, 0.4863281250000000000, 0.4931640625000000000, 0.5000000000000000000, 0.5078125000000000000, 0.5156250000000000000, 0.5234375000000000000, 0.5312500000000000000, 0.5390625000000000000, 0.5468750000000000000, 0.5625000000000000000, 0.5693359375000000000, 0.5761718750000000000, 0.5898437500000000000, 0.5966796875000000000, 0.6035156250000000000, 0.6103515625000000000, 0.6171875000000000000, 0.6308593750000000000, 0.6376953125000000000, 0.6445312500000000000, 0.6513671875000000000, 0.6582031250000000000, 0.6718750000000000000, 0.6787109375000000000, 0.6855468750000000000, 0.6992187500000000000, 0.7128906250000000000, 0.7197265625000000000, 0.7265625000000000000, 0.7333984375000000000, 0.7402343750000000000, 0.7470703125000000000, 0.7539062500000000000, 0.7607421875000000000, 0.7675781250000000000, 0.7744140625000000000, 0.7812500000000000000, 0.7890625000000000000, 0.7968750000000000000, 0.8046875000000000000, 0.8125000000000000000, 0.8203125000000000000, 0.8281250000000000000, 0.8437500000000000000, 0.8505859375000000000, 0.8574218750000000000, 0.8710937500000000000, 0.8779296875000000000, 0.8847656250000000000, 0.8916015625000000000, 0.8984375000000000000, 0.9121093750000000000, 0.9189453125000000000, 0.9257812500000000000, 0.9326171875000000000, 0.9394531250000000000, 0.9531250000000000000, 0.9589843750000000000, 0.9648437500000000000, 0.9765625000000000000, 0.9882812500000000000, 1.000000000000000000 ),
 .UNSPECIFIED. ) 
 GEOMETRIC_REPRESENTATION_ITEM ( )  RATIONAL_B_SPLINE_SURFACE ( (
 ( 1.000000000000000000, 1.000000000000000000, 1.000000000000000000, 1.000000000000000000, 1.000000000000000000, 1.000000000000000000, 1.000000000000000000, 1.000000000000000000, 1.000000000000000000, 1.000000000000000000, 1.000000000000000000, 1.000000000000000000, 1.000000000000000000, 1.000000000000000000, 1.000000000000000000, 1.000000000000000000, 1.000000000000000000, 1.000000000000000000, 1.000000000000000000, 1.000000000000000000, 1.000000000000000000, 1.000000000000000000, 1.000000000000000000, 1.000000000000000000, 1.000000000000000000, 1.000000000000000000, 1.000000000000000000, 1.000000000000000000, 1.000000000000000000, 1.000000000000000000, 1.000000000000000000, 1.000000000000000000, 1.000000000000000000, 1.000000000000000000, 1.000000000000000000, 1.000000000000000000, 1.000000000000000000, 1.000000000000000000, 1.000000000000000000, 1.000000000000000000, 1.000000000000000000, 1.000000000000000000, 1.000000000000000000, 1.000000000000000000, 1.000000000000000000, 1.000000000000000000, 1.000000000000000000, 1.000000000000000000, 1.000000000000000000, 1.000000000000000000, 1.000000000000000000, 1.000000000000000000, 1.000000000000000000, 1.000000000000000000, 1.000000000000000000, 1.000000000000000000, 1.000000000000000000, 1.000000000000000000, 1.000000000000000000, 1.000000000000000000, 1.000000000000000000, 1.000000000000000000, 1.000000000000000000, 1.000000000000000000, 1.000000000000000000, 1.000000000000000000, 1.000000000000000000, 1.000000000000000000, 1.000000000000000000, 1.000000000000000000, 1.000000000000000000, 1.000000000000000000, 1.000000000000000000, 1.000000000000000000, 1.000000000000000000, 1.000000000000000000, 1.000000000000000000, 1.000000000000000000, 1.000000000000000000, 1.000000000000000000, 1.000000000000000000, 1.000000000000000000, 1.000000000000000000, 1.000000000000000000, 1.000000000000000000, 1.000000000000000000, 1.000000000000000000, 1.000000000000000000, 1.000000000000000000, 1.000000000000000000, 1.000000000000000000, 1.000000000000000000, 1.000000000000000000, 1.000000000000000000, 1.000000000000000000, 1.000000000000000000, 1.000000000000000000, 1.000000000000000000, 1.000000000000000000, 1.000000000000000000, 1.000000000000000000, 1.000000000000000000, 1.000000000000000000, 1.000000000000000000, 1.000000000000000000, 1.000000000000000000, 1.000000000000000000, 1.000000000000000000, 1.000000000000000000, 1.000000000000000000, 1.000000000000000000, 1.000000000000000000, 1.000000000000000000, 1.000000000000000000, 1.000000000000000000, 1.000000000000000000, 1.000000000000000000, 1.000000000000000000, 1.000000000000000000, 1.000000000000000000, 1.000000000000000000, 1.000000000000000000, 1.000000000000000000, 1.000000000000000000, 1.000000000000000000, 1.000000000000000000, 1.000000000000000000, 1.000000000000000000, 1.000000000000000000, 1.000000000000000000, 1.000000000000000000, 1.000000000000000000, 1.000000000000000000, 1.000000000000000000, 1.000000000000000000, 1.000000000000000000, 1.000000000000000000, 1.000000000000000000, 1.000000000000000000, 1.000000000000000000, 1.000000000000000000, 1.000000000000000000, 1.000000000000000000, 1.000000000000000000, 1.000000000000000000, 1.000000000000000000, 1.000000000000000000, 1.000000000000000000, 1.000000000000000000, 1.000000000000000000, 1.000000000000000000, 1.000000000000000000, 1.000000000000000000, 1.000000000000000000, 1.000000000000000000, 1.000000000000000000, 1.000000000000000000, 1.000000000000000000, 1.000000000000000000, 1.000000000000000000, 1.000000000000000000, 1.000000000000000000, 1.000000000000000000, 1.000000000000000000, 1.000000000000000000, 1.000000000000000000, 1.000000000000000000, 1.000000000000000000, 1.000000000000000000, 1.000000000000000000, 1.000000000000000000, 1.000000000000000000, 1.000000000000000000, 1.000000000000000000, 1.000000000000000000, 1.000000000000000000, 1.000000000000000000, 1.000000000000000000, 1.000000000000000000, 1.000000000000000000, 1.000000000000000000, 1.000000000000000000, 1.000000000000000000, 1.000000000000000000, 1.000000000000000000, 1.000000000000000000, 1.000000000000000000, 1.000000000000000000, 1.000000000000000000, 1.000000000000000000, 1.000000000000000000, 1.000000000000000000, 1.000000000000000000, 1.000000000000000000, 1.000000000000000000, 1.000000000000000000, 1.000000000000000000, 1.000000000000000000, 1.000000000000000000, 1.000000000000000000, 1.000000000000000000, 1.000000000000000000, 1.000000000000000000, 1.000000000000000000, 1.000000000000000000, 1.000000000000000000, 1.000000000000000000, 1.000000000000000000, 1.000000000000000000, 1.000000000000000000, 1.000000000000000000, 1.000000000000000000, 1.000000000000000000, 1.000000000000000000, 1.000000000000000000, 1.000000000000000000, 1.000000000000000000, 1.000000000000000000, 1.000000000000000000, 1.000000000000000000, 1.000000000000000000, 1.000000000000000000, 1.000000000000000000, 1.000000000000000000, 1.000000000000000000, 1.000000000000000000, 1.000000000000000000, 1.000000000000000000, 1.000000000000000000, 1.000000000000000000, 1.000000000000000000, 1.000000000000000000, 1.000000000000000000, 1.000000000000000000, 1.000000000000000000, 1.000000000000000000, 1.000000000000000000, 1.000000000000000000, 1.000000000000000000, 1.000000000000000000, 1.000000000000000000, 1.000000000000000000, 1.000000000000000000, 1.000000000000000000, 1.000000000000000000, 1.000000000000000000),
 ( 0.3333333333333333703, 0.3333333333333333703, 0.3333333333333333703, 0.3333333333333333703, 0.3333333333333333703, 0.3333333333333333703, 0.3333333333333333703, 0.3333333333333333703, 0.3333333333333333703, 0.3333333333333333703, 0.3333333333333333703, 0.3333333333333333703, 0.3333333333333333703, 0.3333333333333333703, 0.3333333333333333703, 0.3333333333333333703, 0.3333333333333333703, 0.3333333333333333703, 0.3333333333333333703, 0.3333333333333333703, 0.3333333333333333703, 0.3333333333333333703, 0.3333333333333333703, 0.3333333333333333703, 0.3333333333333333703, 0.3333333333333333703, 0.3333333333333333703, 0.3333333333333333703, 0.3333333333333333703, 0.3333333333333333703, 0.3333333333333333703, 0.3333333333333333703, 0.3333333333333333703, 0.3333333333333333703, 0.3333333333333333703, 0.3333333333333333703, 0.3333333333333333703, 0.3333333333333333703, 0.3333333333333333703, 0.3333333333333333703, 0.3333333333333333703, 0.3333333333333333703, 0.3333333333333333703, 0.3333333333333333703, 0.3333333333333333703, 0.3333333333333333703, 0.3333333333333333703, 0.3333333333333333703, 0.3333333333333333703, 0.3333333333333333703, 0.3333333333333333703, 0.3333333333333333703, 0.3333333333333333703, 0.3333333333333333703, 0.3333333333333333703, 0.3333333333333333703, 0.3333333333333333703, 0.3333333333333333703, 0.3333333333333333703, 0.3333333333333333703, 0.3333333333333333703, 0.3333333333333333703, 0.3333333333333333703, 0.3333333333333333703, 0.3333333333333333703, 0.3333333333333333703, 0.3333333333333333703, 0.3333333333333333703, 0.3333333333333333703, 0.3333333333333333703, 0.3333333333333333703, 0.3333333333333333703, 0.3333333333333333703, 0.3333333333333333703, 0.3333333333333333703, 0.3333333333333333703, 0.3333333333333333703, 0.3333333333333333703, 0.3333333333333333703, 0.3333333333333333703, 0.3333333333333333703, 0.3333333333333333703, 0.3333333333333333703, 0.3333333333333333703, 0.3333333333333333703, 0.3333333333333333703, 0.3333333333333333703, 0.3333333333333333703, 0.3333333333333333703, 0.3333333333333333703, 0.3333333333333333703, 0.3333333333333333703, 0.3333333333333333703, 0.3333333333333333703, 0.3333333333333333703, 0.3333333333333333703, 0.3333333333333333703, 0.3333333333333333703, 0.3333333333333333703, 0.3333333333333333703, 0.3333333333333333703, 0.3333333333333333703, 0.3333333333333333703, 0.3333333333333333703, 0.3333333333333333703, 0.3333333333333333703, 0.3333333333333333703, 0.3333333333333333703, 0.3333333333333333703, 0.3333333333333333703, 0.3333333333333333703, 0.3333333333333333703, 0.3333333333333333703, 0.3333333333333333703, 0.3333333333333333703, 0.3333333333333333703, 0.3333333333333333703, 0.3333333333333333703, 0.3333333333333333703, 0.3333333333333333703, 0.3333333333333333703, 0.3333333333333333703, 0.3333333333333333703, 0.3333333333333333703, 0.3333333333333333703, 0.3333333333333333703, 0.3333333333333333703, 0.3333333333333333703, 0.3333333333333333703, 0.3333333333333333703, 0.3333333333333333703, 0.3333333333333333703, 0.3333333333333333703, 0.3333333333333333703, 0.3333333333333333703, 0.3333333333333333703, 0.3333333333333333703, 0.3333333333333333703, 0.3333333333333333703, 0.3333333333333333703, 0.3333333333333333703, 0.3333333333333333703, 0.3333333333333333703, 0.3333333333333333703, 0.3333333333333333703, 0.3333333333333333703, 0.3333333333333333703, 0.3333333333333333703, 0.3333333333333333703, 0.3333333333333333703, 0.3333333333333333703, 0.3333333333333333703, 0.3333333333333333703, 0.3333333333333333703, 0.3333333333333333703, 0.3333333333333333703, 0.3333333333333333703, 0.3333333333333333703, 0.3333333333333333703, 0.3333333333333333703, 0.3333333333333333703, 0.3333333333333333703, 0.3333333333333333703, 0.3333333333333333703, 0.3333333333333333703, 0.3333333333333333703, 0.3333333333333333703, 0.3333333333333333703, 0.3333333333333333703, 0.3333333333333333703, 0.3333333333333333703, 0.3333333333333333703, 0.3333333333333333703, 0.3333333333333333703, 0.3333333333333333703, 0.3333333333333333703, 0.3333333333333333703, 0.3333333333333333703, 0.3333333333333333703, 0.3333333333333333703, 0.3333333333333333703, 0.3333333333333333703, 0.3333333333333333703, 0.3333333333333333703, 0.3333333333333333703, 0.3333333333333333703, 0.3333333333333333703, 0.3333333333333333703, 0.3333333333333333703, 0.3333333333333333703, 0.3333333333333333703, 0.3333333333333333703, 0.3333333333333333703, 0.3333333333333333703, 0.3333333333333333703, 0.3333333333333333703, 0.3333333333333333703, 0.3333333333333333703, 0.3333333333333333703, 0.3333333333333333703, 0.3333333333333333703, 0.3333333333333333703, 0.3333333333333333703, 0.3333333333333333703, 0.3333333333333333703, 0.3333333333333333703, 0.3333333333333333703, 0.3333333333333333703, 0.3333333333333333703, 0.3333333333333333703, 0.3333333333333333703, 0.3333333333333333703, 0.3333333333333333703, 0.3333333333333333703, 0.3333333333333333703, 0.3333333333333333703, 0.3333333333333333703, 0.3333333333333333703, 0.3333333333333333703, 0.3333333333333333703, 0.3333333333333333703, 0.3333333333333333703, 0.3333333333333333703, 0.3333333333333333703, 0.3333333333333333703, 0.3333333333333333703, 0.3333333333333333703, 0.3333333333333333703, 0.3333333333333333703, 0.3333333333333333703, 0.3333333333333333703, 0.3333333333333333703, 0.3333333333333333703, 0.3333333333333333703, 0.3333333333333333703, 0.3333333333333333703, 0.3333333333333333703, 0.3333333333333333703, 0.3333333333333333703, 0.3333333333333333703, 0.3333333333333333703, 0.3333333333333333703, 0.3333333333333333703, 0.3333333333333333703, 0.3333333333333333703, 0.3333333333333333703),
 ( 0.3333333333333333703, 0.3333333333333333703, 0.3333333333333333703, 0.3333333333333333703, 0.3333333333333333703, 0.3333333333333333703, 0.3333333333333333703, 0.3333333333333333703, 0.3333333333333333703, 0.3333333333333333703, 0.3333333333333333703, 0.3333333333333333703, 0.3333333333333333703, 0.3333333333333333703, 0.3333333333333333703, 0.3333333333333333703, 0.3333333333333333703, 0.3333333333333333703, 0.3333333333333333703, 0.3333333333333333703, 0.3333333333333333703, 0.3333333333333333703, 0.3333333333333333703, 0.3333333333333333703, 0.3333333333333333703, 0.3333333333333333703, 0.3333333333333333703, 0.3333333333333333703, 0.3333333333333333703, 0.3333333333333333703, 0.3333333333333333703, 0.3333333333333333703, 0.3333333333333333703, 0.3333333333333333703, 0.3333333333333333703, 0.3333333333333333703, 0.3333333333333333703, 0.3333333333333333703, 0.3333333333333333703, 0.3333333333333333703, 0.3333333333333333703, 0.3333333333333333703, 0.3333333333333333703, 0.3333333333333333703, 0.3333333333333333703, 0.3333333333333333703, 0.3333333333333333703, 0.3333333333333333703, 0.3333333333333333703, 0.3333333333333333703, 0.3333333333333333703, 0.3333333333333333703, 0.3333333333333333703, 0.3333333333333333703, 0.3333333333333333703, 0.3333333333333333703, 0.3333333333333333703, 0.3333333333333333703, 0.3333333333333333703, 0.3333333333333333703, 0.3333333333333333703, 0.3333333333333333703, 0.3333333333333333703, 0.3333333333333333703, 0.3333333333333333703, 0.3333333333333333703, 0.3333333333333333703, 0.3333333333333333703, 0.3333333333333333703, 0.3333333333333333703, 0.3333333333333333703, 0.3333333333333333703, 0.3333333333333333703, 0.3333333333333333703, 0.3333333333333333703, 0.3333333333333333703, 0.3333333333333333703, 0.3333333333333333703, 0.3333333333333333703, 0.3333333333333333703, 0.3333333333333333703, 0.3333333333333333703, 0.3333333333333333703, 0.3333333333333333703, 0.3333333333333333703, 0.3333333333333333703, 0.3333333333333333703, 0.3333333333333333703, 0.3333333333333333703, 0.3333333333333333703, 0.3333333333333333703, 0.3333333333333333703, 0.3333333333333333703, 0.3333333333333333703, 0.3333333333333333703, 0.3333333333333333703, 0.3333333333333333703, 0.3333333333333333703, 0.3333333333333333703, 0.3333333333333333703, 0.3333333333333333703, 0.3333333333333333703, 0.3333333333333333703, 0.3333333333333333703, 0.3333333333333333703, 0.3333333333333333703, 0.3333333333333333703, 0.3333333333333333703, 0.3333333333333333703, 0.3333333333333333703, 0.3333333333333333703, 0.3333333333333333703, 0.3333333333333333703, 0.3333333333333333703, 0.3333333333333333703, 0.3333333333333333703, 0.3333333333333333703, 0.3333333333333333703, 0.3333333333333333703, 0.3333333333333333703, 0.3333333333333333703, 0.3333333333333333703, 0.3333333333333333703, 0.3333333333333333703, 0.3333333333333333703, 0.3333333333333333703, 0.3333333333333333703, 0.3333333333333333703, 0.3333333333333333703, 0.3333333333333333703, 0.3333333333333333703, 0.3333333333333333703, 0.3333333333333333703, 0.3333333333333333703, 0.3333333333333333703, 0.3333333333333333703, 0.3333333333333333703, 0.3333333333333333703, 0.3333333333333333703, 0.3333333333333333703, 0.3333333333333333703, 0.3333333333333333703, 0.3333333333333333703, 0.3333333333333333703, 0.3333333333333333703, 0.3333333333333333703, 0.3333333333333333703, 0.3333333333333333703, 0.3333333333333333703, 0.3333333333333333703, 0.3333333333333333703, 0.3333333333333333703, 0.3333333333333333703, 0.3333333333333333703, 0.3333333333333333703, 0.3333333333333333703, 0.3333333333333333703, 0.3333333333333333703, 0.3333333333333333703, 0.3333333333333333703, 0.3333333333333333703, 0.3333333333333333703, 0.3333333333333333703, 0.3333333333333333703, 0.3333333333333333703, 0.3333333333333333703, 0.3333333333333333703, 0.3333333333333333703, 0.3333333333333333703, 0.3333333333333333703, 0.3333333333333333703, 0.3333333333333333703, 0.3333333333333333703, 0.3333333333333333703, 0.3333333333333333703, 0.3333333333333333703, 0.3333333333333333703, 0.3333333333333333703, 0.3333333333333333703, 0.3333333333333333703, 0.3333333333333333703, 0.3333333333333333703, 0.3333333333333333703, 0.3333333333333333703, 0.3333333333333333703, 0.3333333333333333703, 0.3333333333333333703, 0.3333333333333333703, 0.3333333333333333703, 0.3333333333333333703, 0.3333333333333333703, 0.3333333333333333703, 0.3333333333333333703, 0.3333333333333333703, 0.3333333333333333703, 0.3333333333333333703, 0.3333333333333333703, 0.3333333333333333703, 0.3333333333333333703, 0.3333333333333333703, 0.3333333333333333703, 0.3333333333333333703, 0.3333333333333333703, 0.3333333333333333703, 0.3333333333333333703, 0.3333333333333333703, 0.3333333333333333703, 0.3333333333333333703, 0.3333333333333333703, 0.3333333333333333703, 0.3333333333333333703, 0.3333333333333333703, 0.3333333333333333703, 0.3333333333333333703, 0.3333333333333333703, 0.3333333333333333703, 0.3333333333333333703, 0.3333333333333333703, 0.3333333333333333703, 0.3333333333333333703, 0.3333333333333333703, 0.3333333333333333703, 0.3333333333333333703, 0.3333333333333333703, 0.3333333333333333703, 0.3333333333333333703, 0.3333333333333333703, 0.3333333333333333703, 0.3333333333333333703, 0.3333333333333333703, 0.3333333333333333703, 0.3333333333333333703, 0.3333333333333333703, 0.3333333333333333703, 0.3333333333333333703, 0.3333333333333333703, 0.3333333333333333703, 0.3333333333333333703, 0.3333333333333333703, 0.3333333333333333703, 0.3333333333333333703, 0.3333333333333333703, 0.3333333333333333703, 0.3333333333333333703, 0.3333333333333333703, 0.3333333333333333703),
 ( 1.000000000000000000, 1.000000000000000000, 1.000000000000000000, 1.000000000000000000, 1.000000000000000000, 1.000000000000000000, 1.000000000000000000, 1.000000000000000000, 1.000000000000000000, 1.000000000000000000, 1.000000000000000000, 1.000000000000000000, 1.000000000000000000, 1.000000000000000000, 1.000000000000000000, 1.000000000000000000, 1.000000000000000000, 1.000000000000000000, 1.000000000000000000, 1.000000000000000000, 1.000000000000000000, 1.000000000000000000, 1.000000000000000000, 1.000000000000000000, 1.000000000000000000, 1.000000000000000000, 1.000000000000000000, 1.000000000000000000, 1.000000000000000000, 1.000000000000000000, 1.000000000000000000, 1.000000000000000000, 1.000000000000000000, 1.000000000000000000, 1.000000000000000000, 1.000000000000000000, 1.000000000000000000, 1.000000000000000000, 1.000000000000000000, 1.000000000000000000, 1.000000000000000000, 1.000000000000000000, 1.000000000000000000, 1.000000000000000000, 1.000000000000000000, 1.000000000000000000, 1.000000000000000000, 1.000000000000000000, 1.000000000000000000, 1.000000000000000000, 1.000000000000000000, 1.000000000000000000, 1.000000000000000000, 1.000000000000000000, 1.000000000000000000, 1.000000000000000000, 1.000000000000000000, 1.000000000000000000, 1.000000000000000000, 1.000000000000000000, 1.000000000000000000, 1.000000000000000000, 1.000000000000000000, 1.000000000000000000, 1.000000000000000000, 1.000000000000000000, 1.000000000000000000, 1.000000000000000000, 1.000000000000000000, 1.000000000000000000, 1.000000000000000000, 1.000000000000000000, 1.000000000000000000, 1.000000000000000000, 1.000000000000000000, 1.000000000000000000, 1.000000000000000000, 1.000000000000000000, 1.000000000000000000, 1.000000000000000000, 1.000000000000000000, 1.000000000000000000, 1.000000000000000000, 1.000000000000000000, 1.000000000000000000, 1.000000000000000000, 1.000000000000000000, 1.000000000000000000, 1.000000000000000000, 1.000000000000000000, 1.000000000000000000, 1.000000000000000000, 1.000000000000000000, 1.000000000000000000, 1.000000000000000000, 1.000000000000000000, 1.000000000000000000, 1.000000000000000000, 1.000000000000000000, 1.000000000000000000, 1.000000000000000000, 1.000000000000000000, 1.000000000000000000, 1.000000000000000000, 1.000000000000000000, 1.000000000000000000, 1.000000000000000000, 1.000000000000000000, 1.000000000000000000, 1.000000000000000000, 1.000000000000000000, 1.000000000000000000, 1.000000000000000000, 1.000000000000000000, 1.000000000000000000, 1.000000000000000000, 1.000000000000000000, 1.000000000000000000, 1.000000000000000000, 1.000000000000000000, 1.000000000000000000, 1.000000000000000000, 1.000000000000000000, 1.000000000000000000, 1.000000000000000000, 1.000000000000000000, 1.000000000000000000, 1.000000000000000000, 1.000000000000000000, 1.000000000000000000, 1.000000000000000000, 1.000000000000000000, 1.000000000000000000, 1.000000000000000000, 1.000000000000000000, 1.000000000000000000, 1.000000000000000000, 1.000000000000000000, 1.000000000000000000, 1.000000000000000000, 1.000000000000000000, 1.000000000000000000, 1.000000000000000000, 1.000000000000000000, 1.000000000000000000, 1.000000000000000000, 1.000000000000000000, 1.000000000000000000, 1.000000000000000000, 1.000000000000000000, 1.000000000000000000, 1.000000000000000000, 1.000000000000000000, 1.000000000000000000, 1.000000000000000000, 1.000000000000000000, 1.000000000000000000, 1.000000000000000000, 1.000000000000000000, 1.000000000000000000, 1.000000000000000000, 1.000000000000000000, 1.000000000000000000, 1.000000000000000000, 1.000000000000000000, 1.000000000000000000, 1.000000000000000000, 1.000000000000000000, 1.000000000000000000, 1.000000000000000000, 1.000000000000000000, 1.000000000000000000, 1.000000000000000000, 1.000000000000000000, 1.000000000000000000, 1.000000000000000000, 1.000000000000000000, 1.000000000000000000, 1.000000000000000000, 1.000000000000000000, 1.000000000000000000, 1.000000000000000000, 1.000000000000000000, 1.000000000000000000, 1.000000000000000000, 1.000000000000000000, 1.000000000000000000, 1.000000000000000000, 1.000000000000000000, 1.000000000000000000, 1.000000000000000000, 1.000000000000000000, 1.000000000000000000, 1.000000000000000000, 1.000000000000000000, 1.000000000000000000, 1.000000000000000000, 1.000000000000000000, 1.000000000000000000, 1.000000000000000000, 1.000000000000000000, 1.000000000000000000, 1.000000000000000000, 1.000000000000000000, 1.000000000000000000, 1.000000000000000000, 1.000000000000000000, 1.000000000000000000, 1.000000000000000000, 1.000000000000000000, 1.000000000000000000, 1.000000000000000000, 1.000000000000000000, 1.000000000000000000, 1.000000000000000000, 1.000000000000000000, 1.000000000000000000, 1.000000000000000000, 1.000000000000000000, 1.000000000000000000, 1.000000000000000000, 1.000000000000000000, 1.000000000000000000, 1.000000000000000000, 1.000000000000000000, 1.000000000000000000, 1.000000000000000000, 1.000000000000000000, 1.000000000000000000, 1.000000000000000000, 1.000000000000000000, 1.000000000000000000, 1.000000000000000000, 1.000000000000000000, 1.000000000000000000, 1.000000000000000000, 1.000000000000000000, 1.000000000000000000, 1.000000000000000000, 1.000000000000000000, 1.000000000000000000, 1.000000000000000000, 1.000000000000000000, 1.000000000000000000, 1.000000000000000000, 1.000000000000000000),
 ( 0.3333333333333333703, 0.3333333333333333703, 0.3333333333333333703, 0.3333333333333333703, 0.3333333333333333703, 0.3333333333333333703, 0.3333333333333333703, 0.3333333333333333703, 0.3333333333333333703, 0.3333333333333333703, 0.3333333333333333703, 0.3333333333333333703, 0.3333333333333333703, 0.3333333333333333703, 0.3333333333333333703, 0.3333333333333333703, 0.3333333333333333703, 0.3333333333333333703, 0.3333333333333333703, 0.3333333333333333703, 0.3333333333333333703, 0.3333333333333333703, 0.3333333333333333703, 0.3333333333333333703, 0.3333333333333333703, 0.3333333333333333703, 0.3333333333333333703, 0.3333333333333333703, 0.3333333333333333703, 0.3333333333333333703, 0.3333333333333333703, 0.3333333333333333703, 0.3333333333333333703, 0.3333333333333333703, 0.3333333333333333703, 0.3333333333333333703, 0.3333333333333333703, 0.3333333333333333703, 0.3333333333333333703, 0.3333333333333333703, 0.3333333333333333703, 0.3333333333333333703, 0.3333333333333333703, 0.3333333333333333703, 0.3333333333333333703, 0.3333333333333333703, 0.3333333333333333703, 0.3333333333333333703, 0.3333333333333333703, 0.3333333333333333703, 0.3333333333333333703, 0.3333333333333333703, 0.3333333333333333703, 0.3333333333333333703, 0.3333333333333333703, 0.3333333333333333703, 0.3333333333333333703, 0.3333333333333333703, 0.3333333333333333703, 0.3333333333333333703, 0.3333333333333333703, 0.3333333333333333703, 0.3333333333333333703, 0.3333333333333333703, 0.3333333333333333703, 0.3333333333333333703, 0.3333333333333333703, 0.3333333333333333703, 0.3333333333333333703, 0.3333333333333333703, 0.3333333333333333703, 0.3333333333333333703, 0.3333333333333333703, 0.3333333333333333703, 0.3333333333333333703, 0.3333333333333333703, 0.3333333333333333703, 0.3333333333333333703, 0.3333333333333333703, 0.3333333333333333703, 0.3333333333333333703, 0.3333333333333333703, 0.3333333333333333703, 0.3333333333333333703, 0.3333333333333333703, 0.3333333333333333703, 0.3333333333333333703, 0.3333333333333333703, 0.3333333333333333703, 0.3333333333333333703, 0.3333333333333333703, 0.3333333333333333703, 0.3333333333333333703, 0.3333333333333333703, 0.3333333333333333703, 0.3333333333333333703, 0.3333333333333333703, 0.3333333333333333703, 0.3333333333333333703, 0.3333333333333333703, 0.3333333333333333703, 0.3333333333333333703, 0.3333333333333333703, 0.3333333333333333703, 0.3333333333333333703, 0.3333333333333333703, 0.3333333333333333703, 0.3333333333333333703, 0.3333333333333333703, 0.3333333333333333703, 0.3333333333333333703, 0.3333333333333333703, 0.3333333333333333703, 0.3333333333333333703, 0.3333333333333333703, 0.3333333333333333703, 0.3333333333333333703, 0.3333333333333333703, 0.3333333333333333703, 0.3333333333333333703, 0.3333333333333333703, 0.3333333333333333703, 0.3333333333333333703, 0.3333333333333333703, 0.3333333333333333703, 0.3333333333333333703, 0.3333333333333333703, 0.3333333333333333703, 0.3333333333333333703, 0.3333333333333333703, 0.3333333333333333703, 0.3333333333333333703, 0.3333333333333333703, 0.3333333333333333703, 0.3333333333333333703, 0.3333333333333333703, 0.3333333333333333703, 0.3333333333333333703, 0.3333333333333333703, 0.3333333333333333703, 0.3333333333333333703, 0.3333333333333333703, 0.3333333333333333703, 0.3333333333333333703, 0.3333333333333333703, 0.3333333333333333703, 0.3333333333333333703, 0.3333333333333333703, 0.3333333333333333703, 0.3333333333333333703, 0.3333333333333333703, 0.3333333333333333703, 0.3333333333333333703, 0.3333333333333333703, 0.3333333333333333703, 0.3333333333333333703, 0.3333333333333333703, 0.3333333333333333703, 0.3333333333333333703, 0.3333333333333333703, 0.3333333333333333703, 0.3333333333333333703, 0.3333333333333333703, 0.3333333333333333703, 0.3333333333333333703, 0.3333333333333333703, 0.3333333333333333703, 0.3333333333333333703, 0.3333333333333333703, 0.3333333333333333703, 0.3333333333333333703, 0.3333333333333333703, 0.3333333333333333703, 0.3333333333333333703, 0.3333333333333333703, 0.3333333333333333703, 0.3333333333333333703, 0.3333333333333333703, 0.3333333333333333703, 0.3333333333333333703, 0.3333333333333333703, 0.3333333333333333703, 0.3333333333333333703, 0.3333333333333333703, 0.3333333333333333703, 0.3333333333333333703, 0.3333333333333333703, 0.3333333333333333703, 0.3333333333333333703, 0.3333333333333333703, 0.3333333333333333703, 0.3333333333333333703, 0.3333333333333333703, 0.3333333333333333703, 0.3333333333333333703, 0.3333333333333333703, 0.3333333333333333703, 0.3333333333333333703, 0.3333333333333333703, 0.3333333333333333703, 0.3333333333333333703, 0.3333333333333333703, 0.3333333333333333703, 0.3333333333333333703, 0.3333333333333333703, 0.3333333333333333703, 0.3333333333333333703, 0.3333333333333333703, 0.3333333333333333703, 0.3333333333333333703, 0.3333333333333333703, 0.3333333333333333703, 0.3333333333333333703, 0.3333333333333333703, 0.3333333333333333703, 0.3333333333333333703, 0.3333333333333333703, 0.3333333333333333703, 0.3333333333333333703, 0.3333333333333333703, 0.3333333333333333703, 0.3333333333333333703, 0.3333333333333333703, 0.3333333333333333703, 0.3333333333333333703, 0.3333333333333333703, 0.3333333333333333703, 0.3333333333333333703, 0.3333333333333333703, 0.3333333333333333703, 0.3333333333333333703, 0.3333333333333333703, 0.3333333333333333703, 0.3333333333333333703, 0.3333333333333333703, 0.3333333333333333703, 0.3333333333333333703, 0.3333333333333333703, 0.3333333333333333703, 0.3333333333333333703, 0.3333333333333333703, 0.3333333333333333703, 0.3333333333333333703, 0.3333333333333333703, 0.3333333333333333703, 0.3333333333333333703),
 ( 0.3333333333333333703, 0.3333333333333333703, 0.3333333333333333703, 0.3333333333333333703, 0.3333333333333333703, 0.3333333333333333703, 0.3333333333333333703, 0.3333333333333333703, 0.3333333333333333703, 0.3333333333333333703, 0.3333333333333333703, 0.3333333333333333703, 0.3333333333333333703, 0.3333333333333333703, 0.3333333333333333703, 0.3333333333333333703, 0.3333333333333333703, 0.3333333333333333703, 0.3333333333333333703, 0.3333333333333333703, 0.3333333333333333703, 0.3333333333333333703, 0.3333333333333333703, 0.3333333333333333703, 0.3333333333333333703, 0.3333333333333333703, 0.3333333333333333703, 0.3333333333333333703, 0.3333333333333333703, 0.3333333333333333703, 0.3333333333333333703, 0.3333333333333333703, 0.3333333333333333703, 0.3333333333333333703, 0.3333333333333333703, 0.3333333333333333703, 0.3333333333333333703, 0.3333333333333333703, 0.3333333333333333703, 0.3333333333333333703, 0.3333333333333333703, 0.3333333333333333703, 0.3333333333333333703, 0.3333333333333333703, 0.3333333333333333703, 0.3333333333333333703, 0.3333333333333333703, 0.3333333333333333703, 0.3333333333333333703, 0.3333333333333333703, 0.3333333333333333703, 0.3333333333333333703, 0.3333333333333333703, 0.3333333333333333703, 0.3333333333333333703, 0.3333333333333333703, 0.3333333333333333703, 0.3333333333333333703, 0.3333333333333333703, 0.3333333333333333703, 0.3333333333333333703, 0.3333333333333333703, 0.3333333333333333703, 0.3333333333333333703, 0.3333333333333333703, 0.3333333333333333703, 0.3333333333333333703, 0.3333333333333333703, 0.3333333333333333703, 0.3333333333333333703, 0.3333333333333333703, 0.3333333333333333703, 0.3333333333333333703, 0.3333333333333333703, 0.3333333333333333703, 0.3333333333333333703, 0.3333333333333333703, 0.3333333333333333703, 0.3333333333333333703, 0.3333333333333333703, 0.3333333333333333703, 0.3333333333333333703, 0.3333333333333333703, 0.3333333333333333703, 0.3333333333333333703, 0.3333333333333333703, 0.3333333333333333703, 0.3333333333333333703, 0.3333333333333333703, 0.3333333333333333703, 0.3333333333333333703, 0.3333333333333333703, 0.3333333333333333703, 0.3333333333333333703, 0.3333333333333333703, 0.3333333333333333703, 0.3333333333333333703, 0.3333333333333333703, 0.3333333333333333703, 0.3333333333333333703, 0.3333333333333333703, 0.3333333333333333703, 0.3333333333333333703, 0.3333333333333333703, 0.3333333333333333703, 0.3333333333333333703, 0.3333333333333333703, 0.3333333333333333703, 0.3333333333333333703, 0.3333333333333333703, 0.3333333333333333703, 0.3333333333333333703, 0.3333333333333333703, 0.3333333333333333703, 0.3333333333333333703, 0.3333333333333333703, 0.3333333333333333703, 0.3333333333333333703, 0.3333333333333333703, 0.3333333333333333703, 0.3333333333333333703, 0.3333333333333333703, 0.3333333333333333703, 0.3333333333333333703, 0.3333333333333333703, 0.3333333333333333703, 0.3333333333333333703, 0.3333333333333333703, 0.3333333333333333703, 0.3333333333333333703, 0.3333333333333333703, 0.3333333333333333703, 0.3333333333333333703, 0.3333333333333333703, 0.3333333333333333703, 0.3333333333333333703, 0.3333333333333333703, 0.3333333333333333703, 0.3333333333333333703, 0.3333333333333333703, 0.3333333333333333703, 0.3333333333333333703, 0.3333333333333333703, 0.3333333333333333703, 0.3333333333333333703, 0.3333333333333333703, 0.3333333333333333703, 0.3333333333333333703, 0.3333333333333333703, 0.3333333333333333703, 0.3333333333333333703, 0.3333333333333333703, 0.3333333333333333703, 0.3333333333333333703, 0.3333333333333333703, 0.3333333333333333703, 0.3333333333333333703, 0.3333333333333333703, 0.3333333333333333703, 0.3333333333333333703, 0.3333333333333333703, 0.3333333333333333703, 0.3333333333333333703, 0.3333333333333333703, 0.3333333333333333703, 0.3333333333333333703, 0.3333333333333333703, 0.3333333333333333703, 0.3333333333333333703, 0.3333333333333333703, 0.3333333333333333703, 0.3333333333333333703, 0.3333333333333333703, 0.3333333333333333703, 0.3333333333333333703, 0.3333333333333333703, 0.3333333333333333703, 0.3333333333333333703, 0.3333333333333333703, 0.3333333333333333703, 0.3333333333333333703, 0.3333333333333333703, 0.3333333333333333703, 0.3333333333333333703, 0.3333333333333333703, 0.3333333333333333703, 0.3333333333333333703, 0.3333333333333333703, 0.3333333333333333703, 0.3333333333333333703, 0.3333333333333333703, 0.3333333333333333703, 0.3333333333333333703, 0.3333333333333333703, 0.3333333333333333703, 0.3333333333333333703, 0.3333333333333333703, 0.3333333333333333703, 0.3333333333333333703, 0.3333333333333333703, 0.3333333333333333703, 0.3333333333333333703, 0.3333333333333333703, 0.3333333333333333703, 0.3333333333333333703, 0.3333333333333333703, 0.3333333333333333703, 0.3333333333333333703, 0.3333333333333333703, 0.3333333333333333703, 0.3333333333333333703, 0.3333333333333333703, 0.3333333333333333703, 0.3333333333333333703, 0.3333333333333333703, 0.3333333333333333703, 0.3333333333333333703, 0.3333333333333333703, 0.3333333333333333703, 0.3333333333333333703, 0.3333333333333333703, 0.3333333333333333703, 0.3333333333333333703, 0.3333333333333333703, 0.3333333333333333703, 0.3333333333333333703, 0.3333333333333333703, 0.3333333333333333703, 0.3333333333333333703, 0.3333333333333333703, 0.3333333333333333703, 0.3333333333333333703, 0.3333333333333333703, 0.3333333333333333703, 0.3333333333333333703, 0.3333333333333333703, 0.3333333333333333703, 0.3333333333333333703, 0.3333333333333333703, 0.3333333333333333703, 0.3333333333333333703, 0.3333333333333333703, 0.3333333333333333703, 0.3333333333333333703, 0.3333333333333333703, 0.3333333333333333703),
 ( 1.000000000000000000, 1.000000000000000000, 1.000000000000000000, 1.000000000000000000, 1.000000000000000000, 1.000000000000000000, 1.000000000000000000, 1.000000000000000000, 1.000000000000000000, 1.000000000000000000, 1.000000000000000000, 1.000000000000000000, 1.000000000000000000, 1.000000000000000000, 1.000000000000000000, 1.000000000000000000, 1.000000000000000000, 1.000000000000000000, 1.000000000000000000, 1.000000000000000000, 1.000000000000000000, 1.000000000000000000, 1.000000000000000000, 1.000000000000000000, 1.000000000000000000, 1.000000000000000000, 1.000000000000000000, 1.000000000000000000, 1.000000000000000000, 1.000000000000000000, 1.000000000000000000, 1.000000000000000000, 1.000000000000000000, 1.000000000000000000, 1.000000000000000000, 1.000000000000000000, 1.000000000000000000, 1.000000000000000000, 1.000000000000000000, 1.000000000000000000, 1.000000000000000000, 1.000000000000000000, 1.000000000000000000, 1.000000000000000000, 1.000000000000000000, 1.000000000000000000, 1.000000000000000000, 1.000000000000000000, 1.000000000000000000, 1.000000000000000000, 1.000000000000000000, 1.000000000000000000, 1.000000000000000000, 1.000000000000000000, 1.000000000000000000, 1.000000000000000000, 1.000000000000000000, 1.000000000000000000, 1.000000000000000000, 1.000000000000000000, 1.000000000000000000, 1.000000000000000000, 1.000000000000000000, 1.000000000000000000, 1.000000000000000000, 1.000000000000000000, 1.000000000000000000, 1.000000000000000000, 1.000000000000000000, 1.000000000000000000, 1.000000000000000000, 1.000000000000000000, 1.000000000000000000, 1.000000000000000000, 1.000000000000000000, 1.000000000000000000, 1.000000000000000000, 1.000000000000000000, 1.000000000000000000, 1.000000000000000000, 1.000000000000000000, 1.000000000000000000, 1.000000000000000000, 1.000000000000000000, 1.000000000000000000, 1.000000000000000000, 1.000000000000000000, 1.000000000000000000, 1.000000000000000000, 1.000000000000000000, 1.000000000000000000, 1.000000000000000000, 1.000000000000000000, 1.000000000000000000, 1.000000000000000000, 1.000000000000000000, 1.000000000000000000, 1.000000000000000000, 1.000000000000000000, 1.000000000000000000, 1.000000000000000000, 1.000000000000000000, 1.000000000000000000, 1.000000000000000000, 1.000000000000000000, 1.000000000000000000, 1.000000000000000000, 1.000000000000000000, 1.000000000000000000, 1.000000000000000000, 1.000000000000000000, 1.000000000000000000, 1.000000000000000000, 1.000000000000000000, 1.000000000000000000, 1.000000000000000000, 1.000000000000000000, 1.000000000000000000, 1.000000000000000000, 1.000000000000000000, 1.000000000000000000, 1.000000000000000000, 1.000000000000000000, 1.000000000000000000, 1.000000000000000000, 1.000000000000000000, 1.000000000000000000, 1.000000000000000000, 1.000000000000000000, 1.000000000000000000, 1.000000000000000000, 1.000000000000000000, 1.000000000000000000, 1.000000000000000000, 1.000000000000000000, 1.000000000000000000, 1.000000000000000000, 1.000000000000000000, 1.000000000000000000, 1.000000000000000000, 1.000000000000000000, 1.000000000000000000, 1.000000000000000000, 1.000000000000000000, 1.000000000000000000, 1.000000000000000000, 1.000000000000000000, 1.000000000000000000, 1.000000000000000000, 1.000000000000000000, 1.000000000000000000, 1.000000000000000000, 1.000000000000000000, 1.000000000000000000, 1.000000000000000000, 1.000000000000000000, 1.000000000000000000, 1.000000000000000000, 1.000000000000000000, 1.000000000000000000, 1.000000000000000000, 1.000000000000000000, 1.000000000000000000, 1.000000000000000000, 1.000000000000000000, 1.000000000000000000, 1.000000000000000000, 1.000000000000000000, 1.000000000000000000, 1.000000000000000000, 1.000000000000000000, 1.000000000000000000, 1.000000000000000000, 1.000000000000000000, 1.000000000000000000, 1.000000000000000000, 1.000000000000000000, 1.000000000000000000, 1.000000000000000000, 1.000000000000000000, 1.000000000000000000, 1.000000000000000000, 1.000000000000000000, 1.000000000000000000, 1.000000000000000000, 1.000000000000000000, 1.000000000000000000, 1.000000000000000000, 1.000000000000000000, 1.000000000000000000, 1.000000000000000000, 1.000000000000000000, 1.000000000000000000, 1.000000000000000000, 1.000000000000000000, 1.000000000000000000, 1.000000000000000000, 1.000000000000000000, 1.000000000000000000, 1.000000000000000000, 1.000000000000000000, 1.000000000000000000, 1.000000000000000000, 1.000000000000000000, 1.000000000000000000, 1.000000000000000000, 1.000000000000000000, 1.000000000000000000, 1.000000000000000000, 1.000000000000000000, 1.000000000000000000, 1.000000000000000000, 1.000000000000000000, 1.000000000000000000, 1.000000000000000000, 1.000000000000000000, 1.000000000000000000, 1.000000000000000000, 1.000000000000000000, 1.000000000000000000, 1.000000000000000000, 1.000000000000000000, 1.000000000000000000, 1.000000000000000000, 1.000000000000000000, 1.000000000000000000, 1.000000000000000000, 1.000000000000000000, 1.000000000000000000, 1.000000000000000000, 1.000000000000000000, 1.000000000000000000, 1.000000000000000000, 1.000000000000000000, 1.000000000000000000, 1.000000000000000000, 1.000000000000000000, 1.000000000000000000, 1.000000000000000000, 1.000000000000000000, 1.000000000000000000, 1.000000000000000000, 1.000000000000000000, 1.000000000000000000, 1.000000000000000000, 1.000000000000000000) ) ) 
 REPRESENTATION_ITEM ( '' )  SURFACE ( )  );
#20656 = CARTESIAN_POINT ( 'NONE',  ( 25.50411877999659893, -13.63830170496968996, -16.08255890605547123 ) ) ;
#20657 = CARTESIAN_POINT ( 'NONE',  ( 27.28133297882270014, -12.52022702279392874, -15.45456112525011427 ) ) ;
#20658 = CIRCLE ( 'NONE', #7508, 5.000000000000006217 ) ;
#20659 = ORIENTED_EDGE ( 'NONE', *, *, #1587, .T. ) ;
#20660 = DIRECTION ( 'NONE',  ( 0.3090169943749475623, 8.338696094058001131E-17, 0.9510565162951536422 ) ) ;
#20661 = DIRECTION ( 'NONE',  ( -2.698458740408365879E-16, 1.000000000000000000, 0.000000000000000000 ) ) ;
#20662 = DIRECTION ( 'NONE',  ( 1.000000000000000000, 4.440892098500622217E-16, 0.000000000000000000 ) ) ;
#20663 = DIRECTION ( 'NONE',  ( -1.000000000000000000, 0.000000000000000000, 0.000000000000000000 ) ) ;
#20664 = CARTESIAN_POINT ( 'NONE',  ( 168.6922820468853956, -4.999999999999971578, -32.39392330124607611 ) ) ;
#20665 = DIRECTION ( 'NONE',  ( -2.698458740408365879E-16, 1.000000000000000000, 0.000000000000000000 ) ) ;
#20666 = CARTESIAN_POINT ( 'NONE',  ( 23.76792026503975919, -8.198361753721227885, -14.67730844950409441 ) ) ;
#20667 = CARTESIAN_POINT ( 'NONE',  ( 18.39996379557756256, 0.6904185378075045065, -15.43317298867526866 ) ) ;
#20668 = EDGE_CURVE ( 'NONE', #14905, #14471, #17803, .T. ) ;
#20669 = EDGE_CURVE ( 'NONE', #29571, #12856, #3196, .T. ) ;
#20670 = CARTESIAN_POINT ( 'NONE',  ( 33.74345058881453241, -15.07496310474945922, -20.85461858825047798 ) ) ;
#20671 = DIRECTION ( 'NONE',  ( 1.000000000000000000, 0.000000000000000000, 0.000000000000000000 ) ) ;
#20672 = CARTESIAN_POINT ( 'NONE',  ( 11.46775782571576130, 9.292755756535285627, -15.86302895122203616 ) ) ;
#20673 = VECTOR ( 'NONE', #21917, 1000.000000000000000 ) ;
#20674 = CARTESIAN_POINT ( 'NONE',  ( 157.2287565553229172, -1.999999999999974465, -3.509618943233403510 ) ) ;
#20675 = DIRECTION ( 'NONE',  ( -1.000000000000000000, -1.332267629550187651E-15, 0.000000000000000000 ) ) ;
#20676 = CARTESIAN_POINT ( 'NONE',  ( 9.668378799564367299, 16.22503635135577227, -17.88486489230207965 ) ) ;
#20677 = CARTESIAN_POINT ( 'NONE',  ( 172.0152310637604955, -4.999999999999970690, -34.70218595412750773 ) ) ;
#20678 = DIRECTION ( 'NONE',  ( -0.000000000000000000, -0.000000000000000000, -1.000000000000000000 ) ) ;
#20679 = CARTESIAN_POINT ( 'NONE',  ( 12.51417009928267099, 8.576964204390579383, -15.11888119342340353 ) ) ;
#20680 = ORIENTED_EDGE ( 'NONE', *, *, #3604, .T. ) ;
#20681 = CARTESIAN_POINT ( 'NONE',  ( 158.6922820468853104, -1.999999999999974465, 2.247092850131519715 ) ) ;
#20682 = PLANE ( 'NONE',  #14648 ) ;
#20683 = LINE ( 'NONE', #27607, #8791 ) ;
#20684 = ORIENTED_EDGE ( 'NONE', *, *, #17148, .F. ) ;
#20685 = EDGE_CURVE ( 'NONE', #22122, #3594, #8847, .T. ) ;
#20686 = ORIENTED_EDGE ( 'NONE', *, *, #9092, .F. ) ;
#20687 = CARTESIAN_POINT ( 'NONE',  ( 9.120682955242472190, 16.14398363876680520, -17.05135327743868245 ) ) ;
#20688 = CARTESIAN_POINT ( 'NONE',  ( 32.00110207675911767, -10.95298233446834502, -16.54939777171900417 ) ) ;
#20689 = ORIENTED_EDGE ( 'NONE', *, *, #27170, .T. ) ;
#20690 = CARTESIAN_POINT ( 'NONE',  ( 18.53087132295907935, 5.398958961476600038, -21.24745519132487459 ) ) ;
#20691 = CARTESIAN_POINT ( 'NONE',  ( 17.40794641162625567, 9.636182090832996039, -14.27881468665684395 ) ) ;
#20692 = CARTESIAN_POINT ( 'NONE',  ( -2.309976723937612331, 7.903938623646880046, -4.869346954796183624 ) ) ;
#20693 = CARTESIAN_POINT ( 'NONE',  ( 25.10166869626759123, -5.595937160916529152, -20.34551573546397307 ) ) ;
#20694 = VECTOR ( 'NONE', #15295, 1000.000000000000000 ) ;
#20695 = ORIENTED_EDGE ( 'NONE', *, *, #24360, .T. ) ;
#20696 = CARTESIAN_POINT ( 'NONE',  ( 156.1922820468853956, -4.999999999999975131, -22.25671179336496053 ) ) ;
#20698 = ORIENTED_EDGE ( 'NONE', *, *, #16385, .F. ) ;
#20697 = LINE ( 'NONE', #16126, #23370 ) ;
#20699 = VERTEX_POINT ( 'NONE', #13429 ) ;
#20700 = DIRECTION ( 'NONE',  ( -0.5877852522924731371, 0.000000000000000000, 0.8090169943749474513 ) ) ;
#20701 = CARTESIAN_POINT ( 'NONE',  ( 142.2287565553230309, -4.999999999999979572, -20.83012701892219454 ) ) ;
#20702 = EDGE_CURVE ( 'NONE', #11337, #23759, #13874, .T. ) ;
#20703 = CARTESIAN_POINT ( 'NONE',  ( 35.54859390953724585, -21.18451583373416014, -18.06010107863414405 ) ) ;
#20704 = CARTESIAN_POINT ( 'NONE',  ( 11.28991474634619863, 7.910464746135025926, -16.02350989558273753 ) ) ;
#20705 = EDGE_CURVE ( 'NONE', #25132, #28670, #4726, .T. ) ;
#20706 = ORIENTED_EDGE ( 'NONE', *, *, #21385, .T. ) ;
#20707 = CARTESIAN_POINT ( 'NONE',  ( 28.01381056668970260, -10.10121741814351459, -18.82353034625045041 ) ) ;
#20708 = CARTESIAN_POINT ( 'NONE',  ( 3.344563996438202569, 2.687817229851458212, -0.1586754815284793507 ) ) ;
#20709 = CARTESIAN_POINT ( 'NONE',  ( 11.37973238226026318, 12.28930733048782642, -16.95943368139929319 ) ) ;
#20710 = FACE_BOUND ( 'NONE', #9343, .T. ) ;
#20711 = LINE ( 'NONE', #18437, #18855 ) ;
#20712 = VERTEX_POINT ( 'NONE', #2312 ) ;
#20713 = PLANE ( 'NONE',  #20257 ) ;
#20714 = VECTOR ( 'NONE', #13588, 1000.000000000000000 ) ;
#20715 = CARTESIAN_POINT ( 'NONE',  ( 12.51417009928267099, 8.576964204390579383, -15.11888119342340353 ) ) ;
#20716 = EDGE_LOOP ( 'NONE', ( #5661, #15242, #10073, #15587, #18886, #922 ) ) ;
#20717 = ORIENTED_EDGE ( 'NONE', *, *, #12072, .T. ) ;
#20718 = CARTESIAN_POINT ( 'NONE',  ( 172.7287565553229456, -1.999999999999970468, 6.499999999999977796 ) ) ;
#20719 = ORIENTED_EDGE ( 'NONE', *, *, #26826, .T. ) ;
#20720 = CARTESIAN_POINT ( 'NONE',  ( 9.667809135389937580, 16.22764890387498227, -17.88510185254740747 ) ) ;
#20721 = CARTESIAN_POINT ( 'NONE',  ( 22.74932893098897324, -1.793276863599028381, -13.92998459126509836 ) ) ;
#20722 = CARTESIAN_POINT ( 'NONE',  ( 20.01442678821067034, -2.980627454636011198, -16.03144472681325183 ) ) ;
#20723 = VERTEX_POINT ( 'NONE', #25195 ) ;
#20724 = CARTESIAN_POINT ( 'NONE',  ( 17.40782953567980229, 3.270613820851801190, -14.52895612053623609 ) ) ;
#20725 = DIRECTION ( 'NONE',  ( 1.000000000000000000, 0.000000000000000000, 0.000000000000000000 ) ) ;
#20726 = DIRECTION ( 'NONE',  ( -2.698458740408365879E-16, 1.000000000000000000, 0.000000000000000000 ) ) ;
#20727 = VECTOR ( 'NONE', #91, 1000.000000000000000 ) ;
#20728 = CARTESIAN_POINT ( 'NONE',  ( 22.39939798857497877, 2.694615832958070722, -14.02792042734668065 ) ) ;
#20729 = CIRCLE ( 'NONE', #1772, 4.250000000000000000 ) ;
#20730 = CARTESIAN_POINT ( 'NONE',  ( 139.7287565553230024, -1.999999999999979128, 0.8205080756887930260 ) ) ;
#20731 = CARTESIAN_POINT ( 'NONE',  ( 168.6922820468852819, -4.999999999999971578, 2.247092850131519715 ) ) ;
#20732 = VECTOR ( 'NONE', #25317, 1000.000000000000000 ) ;
#20733 = VECTOR ( 'NONE', #5569, 1000.000000000000000 ) ;
#20734 = CARTESIAN_POINT ( 'NONE',  ( 10.35865474790814211, 16.97209951875106526, -17.91014213605047445 ) ) ;
#20735 = EDGE_CURVE ( 'NONE', #2371, #9664, #20294, .T. ) ;
#20736 = DIRECTION ( 'NONE',  ( 1.000000000000000000, 4.440892098500622217E-16, 0.000000000000000000 ) ) ;
#20737 = CARTESIAN_POINT ( 'NONE',  ( 133.7287565553229172, -9.999999999999982236, -36.50000000000000711 ) ) ;
#20738 = AXIS2_PLACEMENT_3D ( 'NONE', #23424, #21272, #18536 ) ;
#20739 = ORIENTED_EDGE ( 'NONE', *, *, #24061, .F. ) ;
#20740 = EDGE_CURVE ( 'NONE', #14836, #22599, #20598, .T. ) ;
#20741 = VERTEX_POINT ( 'NONE', #11584 ) ;
#20742 = DIRECTION ( 'NONE',  ( 2.908569913943826047E-16, -1.000000000000000000, 6.826925868028107924E-18 ) ) ;
#20743 = EDGE_CURVE ( 'NONE', #3603, #4340, #29981, .T. ) ;
#20744 = CARTESIAN_POINT ( 'NONE',  ( 17.32873655921053313, 10.26331207550778579, -16.20725374984683143 ) ) ;
#20745 = CARTESIAN_POINT ( 'NONE',  ( 11.05714535396004727, 17.68148921877153157, -17.77574279453144968 ) ) ;
#20746 = CARTESIAN_POINT ( 'NONE',  ( 34.11209566957792561, -15.73109017586260272, -19.92372960426217787 ) ) ;
#20747 = ORIENTED_EDGE ( 'NONE', *, *, #7573, .F. ) ;
#20748 = VERTEX_POINT ( 'NONE', #29683 ) ;
#20749 = VERTEX_POINT ( 'NONE', #20898 ) ;
#20750 = CARTESIAN_POINT ( 'NONE',  ( 9.641350810849047548, 17.66889113945805789, -17.91796598306941135 ) ) ;
#20751 = VECTOR ( 'NONE', #23750, 1000.000000000000000 ) ;
#20752 = CARTESIAN_POINT ( 'NONE',  ( 12.86487521014348623, 7.673917307032582791, -14.83936302970355037 ) ) ;
#20753 = CYLINDRICAL_SURFACE ( 'NONE', #27394, 5.000000000000000000 ) ;
#20754 = ORIENTED_EDGE ( 'NONE', *, *, #25979, .T. ) ;
#20755 = DIRECTION ( 'NONE',  ( 1.000000000000000000, 0.000000000000000000, 0.000000000000000000 ) ) ;
#20756 = ORIENTED_EDGE ( 'NONE', *, *, #15683, .T. ) ;
#20757 = CARTESIAN_POINT ( 'NONE',  ( 10.47151541139924547, 16.45450612959241354, -17.33501744001014444 ) ) ;
#20759 = CARTESIAN_POINT ( 'NONE',  ( 36.54859390953724585, -21.18451583373416014, -18.06010107863414405 ) ) ;
#20758 = AXIS2_PLACEMENT_3D ( 'NONE', #7420, #26040, #28658 ) ;
#20760 = CARTESIAN_POINT ( 'NONE',  ( 28.16462234717350199, -5.661059359726887230, -16.30864077692347536 ) ) ;
#20761 = ORIENTED_EDGE ( 'NONE', *, *, #25489, .T. ) ;
#20762 = AXIS2_PLACEMENT_3D ( 'NONE', #5109, #14400, #14847 ) ;
#20763 = CARTESIAN_POINT ( 'NONE',  ( 137.0152310637606092, -10.00000000000000533, -15.61832212156129351 ) ) ;
#20764 = CARTESIAN_POINT ( 'NONE',  ( 110.6987386064946293, -4.999999999999987566, -80.42734139416724304 ) ) ;
#20765 = CARTESIAN_POINT ( 'NONE',  ( 26.88053589187069292, -12.95240298029966119, -14.33176627689639382 ) ) ;
#20766 = CARTESIAN_POINT ( 'NONE',  ( 23.87837110222071502, -4.315358902625421322, -12.52832693522684693 ) ) ;
#20767 = ORIENTED_EDGE ( 'NONE', *, *, #26361, .T. ) ;
#20768 = EDGE_CURVE ( 'NONE', #22008, #24060, #16019, .T. ) ;
#20769 = CARTESIAN_POINT ( 'NONE',  ( -24.99999999999998934, 60.00000000000000711, 29.99999999999999289 ) ) ;
#20770 = EDGE_CURVE ( 'NONE', #2286, #1194, #27819, .T. ) ;
#20771 = DIRECTION ( 'NONE',  ( -0.5877852522924731371, -1.586114251531760728E-16, -0.8090169943749474513 ) ) ;
#20772 = CARTESIAN_POINT ( 'NONE',  ( 147.2287565553230309, -1.999999999999976241, -29.49038105676660138 ) ) ;
#20773 = AXIS2_PLACEMENT_3D ( 'NONE', #21106, #21560, #7520 ) ;
#20774 = EDGE_LOOP ( 'NONE', ( #20311, #28316, #16819, #14539 ) ) ;
#20775 = EDGE_CURVE ( 'NONE', #17796, #2286, #4136, .T. ) ;
#20776 = LINE ( 'NONE', #20934, #13875 ) ;
#20777 =( REPRESENTATION_RELATIONSHIP ('NONE','NONE', #5250, #29092 ) REPRESENTATION_RELATIONSHIP_WITH_TRANSFORMATION ( #5363 )SHAPE_REPRESENTATION_RELATIONSHIP( ) );
#20778 = CIRCLE ( 'NONE', #7640, 3.000000000000002665 ) ;
#20779 = PRODUCT_DEFINITION_CONTEXT ( 'detailed design', #1518, 'design' ) ;
#20780 = ADVANCED_FACE ( 'NONE', ( #1868 ), #18620, .T. ) ;
#20781 = EDGE_CURVE ( 'NONE', #13500, #12515, #20449, .T. ) ;
#20782 = CARTESIAN_POINT ( 'NONE',  ( 10.33811723165831786, 18.38618817278374706, -17.91339614244408907 ) ) ;
#20783 = EDGE_CURVE ( 'NONE', #16407, #19094, #18162, .T. ) ;
#20784 = CARTESIAN_POINT ( 'NONE',  ( 175.7287565553229456, -4.999999999999970690, -28.21440484423853334 ) ) ;
#20785 = EDGE_LOOP ( 'NONE', ( #12296, #13627, #13710, #26580 ) ) ;
#20786 = PLANE ( 'NONE',  #23233 ) ;
#20787 = ORIENTED_EDGE ( 'NONE', *, *, #9236, .T. ) ;
#20788 = CARTESIAN_POINT ( 'NONE',  ( 11.45661370752365116, 9.343864103108954211, -15.86763743611193789 ) ) ;
#20789 = ORIENTED_EDGE ( 'NONE', *, *, #29829, .T. ) ;
#20790 = CARTESIAN_POINT ( 'NONE',  ( 17.31141255128542511, 8.026854538702009378, -19.31233526832781777 ) ) ;
#20791 = DIRECTION ( 'NONE',  ( 1.000000000000000000, 4.440892098500622217E-16, 0.000000000000000000 ) ) ;
#20792 = CARTESIAN_POINT ( 'NONE',  ( 88.57129075698978227, -4.999999999999992895, 64.35080949528121153 ) ) ;
#20794 = ORIENTED_EDGE ( 'NONE', *, *, #26560, .T. ) ;
#20793 = CARTESIAN_POINT ( 'NONE',  ( 24.60501232743784783, -9.531698448777172317, -16.22453333552994792 ) ) ;
#20795 = EDGE_LOOP ( 'NONE', ( #14742, #19080, #14421, #27981, #7519 ) ) ;
#20796 = DIRECTION ( 'NONE',  ( 1.000000000000000000, 2.698458740408365879E-16, -1.110223024625156540E-16 ) ) ;
#20797 = CARTESIAN_POINT ( 'NONE',  ( 12.24518234991790955, 9.516123393600787850, -15.33326918312795328 ) ) ;
#20798 = CARTESIAN_POINT ( 'NONE',  ( 34.75406370242679799, -18.61511248754081294, -20.11778113987843852 ) ) ;
#20799 = DIRECTION ( 'NONE',  ( -1.110223024625156540E-16, 0.000000000000000000, -1.000000000000000000 ) ) ;
#20800 = VECTOR ( 'NONE', #25688, 1000.000000000000000 ) ;
#20801 = DIRECTION ( 'NONE',  ( -0.000000000000000000, -0.000000000000000000, -1.000000000000000000 ) ) ;
#20802 = CARTESIAN_POINT ( 'NONE',  ( 22.82249278870453679, 0.4072072893072278821, -18.57859108775207702 ) ) ;
#20803 = ORIENTED_EDGE ( 'NONE', *, *, #8034, .T. ) ;
#20804 = CARTESIAN_POINT ( 'NONE',  ( 24.59515107160807190, -5.000000000000010658, -75.69609154742651924 ) ) ;
#20805 = CARTESIAN_POINT ( 'NONE',  ( 21.92441584138004984, 2.204866226087792924, -14.79409581392398110 ) ) ;
#20806 = VECTOR ( 'NONE', #23513, 1000.000000000000000 ) ;
#20807 = CARTESIAN_POINT ( 'NONE',  ( 28.29154804861901340, -7.753790107393749409, -19.00671289252072782 ) ) ;
#20808 = ORIENTED_EDGE ( 'NONE', *, *, #3068, .T. ) ;
#20809 = EDGE_CURVE ( 'NONE', #2921, #17847, #22912, .T. ) ;
#20810 = DIRECTION ( 'NONE',  ( 0.000000000000000000, 0.000000000000000000, -1.000000000000000000 ) ) ;
#20811 = DIRECTION ( 'NONE',  ( -0.8090169943749474513, -2.183098979609982436E-16, 0.5877852522924731371 ) ) ;
#20812 = CARTESIAN_POINT ( 'NONE',  ( 88.88404763164710687, -4.999999999999992895, 64.57804066564578704 ) ) ;
#20813 = LINE ( 'NONE', #25085, #21347 ) ;
#20814 = ADVANCED_FACE ( 'NONE', ( #4436 ), #4158, .T. ) ;
#20815 = LINE ( 'NONE', #16242, #8008 ) ;
#20816 = VECTOR ( 'NONE', #3076, 1000.000000000000000 ) ;
#20817 = EDGE_CURVE ( 'NONE', #15401, #21438, #18766, .T. ) ;
#20818 = CARTESIAN_POINT ( 'NONE',  ( 9.641351338355821810, 17.66888872024471624, -17.91303689663363130 ) ) ;
#20819 = EDGE_CURVE ( 'NONE', #12466, #30027, #16923, .T. ) ;
#20820 = CARTESIAN_POINT ( 'NONE',  ( 24.28190956353967422, -4.127413435877471670, -12.52835809790152766 ) ) ;
#20821 = CARTESIAN_POINT ( 'NONE',  ( 17.10097030076851610, 6.697663726599960121, -13.82760435466811089 ) ) ;
#20822 = CARTESIAN_POINT ( 'NONE',  ( 34.59940796595157053, -18.92032618698594248, -21.11335396907232465 ) ) ;
#20823 = FILL_AREA_STYLE_COLOUR ( '', #3236 ) ;
#20824 = VECTOR ( 'NONE', #28335, 1000.000000000000000 ) ;
#20825 = PLANE ( 'NONE',  #18535 ) ;
#20826 = DIRECTION ( 'NONE',  ( -0.8090169943749474513, -2.183098979609982436E-16, -0.5877852522924731371 ) ) ;
#20827 = FACE_OUTER_BOUND ( 'NONE', #27265, .T. ) ;
#20828 = CARTESIAN_POINT ( 'NONE',  ( 16.21960234321935701, 7.070186740785398882, -14.59618053200276044 ) ) ;
#20829 = VERTEX_POINT ( 'NONE', #26254 ) ;
#20830 = FACE_OUTER_BOUND ( 'NONE', #6126, .T. ) ;
#20831 = CARTESIAN_POINT ( 'NONE',  ( 12.50736435846123484, 8.573956625762026107, -15.12430548898761806 ) ) ;
#20832 = EDGE_LOOP ( 'NONE', ( #3701, #25028, #14346, #11991 ) ) ;
#20833 = CARTESIAN_POINT ( 'NONE',  ( 168.6922820468853672, -4.999999999999971578, -26.58683881228715862 ) ) ;
#20834 = CARTESIAN_POINT ( 'NONE',  ( 3.999999999999980904, -2.309401076758567317, -2.092734410091829034 ) ) ;
#20835 = CARTESIAN_POINT ( 'NONE',  ( 17.69365662292968366, 10.27476822432933545, -17.01437286930526227 ) ) ;
#20836 = VERTEX_POINT ( 'NONE', #5908 ) ;
#20837 = VERTEX_POINT ( 'NONE', #23654 ) ;
#20838 = CARTESIAN_POINT ( 'NONE',  ( 9.110807846758516959, 16.18927214505777812, -17.05547580459120383 ) ) ;
#20839 = CARTESIAN_POINT ( 'NONE',  ( 33.18306031693006730, -12.55741664378837896, -20.68523176094931415 ) ) ;
#20840 = ORIENTED_EDGE ( 'NONE', *, *, #3989, .F. ) ;
#20841 = CARTESIAN_POINT ( 'NONE',  ( 19.48958755759471728, 3.937961857331544469, -13.19130291127160959 ) ) ;
#20842 = CARTESIAN_POINT ( 'NONE',  ( 13.80032290073870449, 8.087308377618120048, -14.09379472307618641 ) ) ;
#20843 = VECTOR ( 'NONE', #13469, 1000.000000000000000 ) ;
#20844 = LINE ( 'NONE', #12258, #27943 ) ;
#20845 = CARTESIAN_POINT ( 'NONE',  ( 19.75542110462093959, -4.861139154975066212, -17.07234110396024818 ) ) ;
#20846 = ADVANCED_FACE ( 'NONE', ( #613 ), #7179, .T. ) ;
#20847 = VECTOR ( 'NONE', #8420, 1000.000000000000000 ) ;
#20848 = ORIENTED_EDGE ( 'NONE', *, *, #22803, .F. ) ;
#20849 = CARTESIAN_POINT ( 'NONE',  ( 153.6922820468853388, -10.00000000000000178, -17.92658477444275533 ) ) ;
#20850 = CIRCLE ( 'NONE', #25749, 2.749999999999999112 ) ;
#20852 = ORIENTED_EDGE ( 'NONE', *, *, #26284, .F. ) ;
#20851 = FACE_OUTER_BOUND ( 'NONE', #25430, .T. ) ;
#20853 = CARTESIAN_POINT ( 'NONE',  ( 136.1922820468854241, -4.999999999999980460, -19.40354224447947473 ) ) ;
#20854 = EDGE_CURVE ( 'NONE', #19668, #20364, #162, .T. ) ;
#20855 = CARTESIAN_POINT ( 'NONE',  ( 142.2287565553230309, -1.999999999999978018, -29.49038105676660138 ) ) ;
#20856 = CARTESIAN_POINT ( 'NONE',  ( 34.75280465199809043, -13.11698595563971459, -19.00481823564506101 ) ) ;
#20857 = CARTESIAN_POINT ( 'NONE',  ( 12.72406076201818870, 7.612173793771704666, -14.95155764689848965 ) ) ;
#20858 = ORIENTED_EDGE ( 'NONE', *, *, #16826, .T. ) ;
#20859 = AXIS2_PLACEMENT_3D ( 'NONE', #14953, #5371, #16960 ) ;
#20860 = DIRECTION ( 'NONE',  ( -2.698458740408365879E-16, 1.000000000000000000, 0.000000000000000000 ) ) ;
#20861 = CARTESIAN_POINT ( 'NONE',  ( 159.5152310637604671, -9.999999999999998224, -13.05155085951651195 ) ) ;
#20862 = CARTESIAN_POINT ( 'NONE',  ( 10.35900481074863322, 16.97049408594186914, -17.87076805301065363 ) ) ;
#20863 = FACE_OUTER_BOUND ( 'NONE', #24568, .T. ) ;
#20864 = LINE ( 'NONE', #13706, #5151 ) ;
#20865 = ORIENTED_EDGE ( 'NONE', *, *, #19857, .T. ) ;
#20866 = VECTOR ( 'NONE', #25931, 1000.000000000000000 ) ;
#20867 = DIRECTION ( 'NONE',  ( -2.698458740408365879E-16, 1.000000000000000000, 0.000000000000000000 ) ) ;
#20868 = CARTESIAN_POINT ( 'NONE',  ( 177.2287565553228319, -9.999999999999994671, -3.509618943233403510 ) ) ;
#20869 = ORIENTED_EDGE ( 'NONE', *, *, #17005, .T. ) ;
#20870 = ORIENTED_EDGE ( 'NONE', *, *, #15518, .T. ) ;
#20871 = LINE ( 'NONE', #27946, #11558 ) ;
#20872 = VECTOR ( 'NONE', #7161, 1000.000000000000000 ) ;
#20873 = EDGE_LOOP ( 'NONE', ( #19139, #13690, #15267 ) ) ;
#20874 = CARTESIAN_POINT ( 'NONE',  ( 9.829968513350019421, 15.48396532603707421, -17.81804186139787660 ) ) ;
#20875 = AXIS2_PLACEMENT_3D ( 'NONE', #26988, #3762, #23810 ) ;
#20876 = CARTESIAN_POINT ( 'NONE',  ( 23.01595892079019379, -1.674233493421072305, -13.97569732891719241 ) ) ;
#20877 = CARTESIAN_POINT ( 'NONE',  ( 23.17017814088865535, -4.132587038751921682, -14.65442522582375240 ) ) ;
#20878 = CARTESIAN_POINT ( 'NONE',  ( 19.30972751531945519, 5.994221256738944348, -19.84686166629000326 ) ) ;
#20879 = LINE ( 'NONE', #14157, #6752 ) ;
#20880 = CARTESIAN_POINT ( 'NONE',  ( 152.0152310637604955, -10.00000000000000178, -8.721423840594312082 ) ) ;
#20881 = CARTESIAN_POINT ( 'NONE',  ( 166.1922820468853104, -4.999999999999972466, -2.083034168790677043 ) ) ;
#20882 = ADVANCED_FACE ( 'NONE', ( #11885 ), #7575, .T. ) ;
#20883 = EDGE_CURVE ( 'NONE', #2624, #13296, #9997, .T. ) ;
#20884 = CARTESIAN_POINT ( 'NONE',  ( 23.60870351872479844, -7.222488552757559077, -14.83554404960226947 ) ) ;
#20885 = CARTESIAN_POINT ( 'NONE',  ( 7.738597516018001166, -5.000000000000015987, 23.81695417587389940 ) ) ;
#20886 = DIRECTION ( 'NONE',  ( -0.9510565162951536422, 0.000000000000000000, -0.3090169943749472292 ) ) ;
#20887 = VECTOR ( 'NONE', #3873, 1000.000000000000000 ) ;
#20888 =( NAMED_UNIT ( * ) SI_UNIT ( $, .STERADIAN. ) SOLID_ANGLE_UNIT ( ) );
#20889 = CARTESIAN_POINT ( 'NONE',  ( 161.1922820468853672, -9.999999999999998224, -19.40354224447947828 ) ) ;
#20890 = DIRECTION ( 'NONE',  ( -2.698458740408365879E-16, 1.000000000000000000, 0.000000000000000000 ) ) ;
#20891 = VECTOR ( 'NONE', #29484, 1000.000000000000000 ) ;
#20892 = CARTESIAN_POINT ( 'NONE',  ( 10.35864924400752862, 16.97212476034085782, -17.91519562840587199 ) ) ;
#20893 = CARTESIAN_POINT ( 'NONE',  ( 35.54859390953724585, -22.18451583373416014, -18.19919658220850778 ) ) ;
#20894 = CARTESIAN_POINT ( 'NONE',  ( 33.29928106196997817, -12.14339677642331772, -19.64090527578606427 ) ) ;
#20895 = ORIENTED_EDGE ( 'NONE', *, *, #8660, .F. ) ;
#20896 = CARTESIAN_POINT ( 'NONE',  ( 11.29844335826449964, 8.819016302236921234, -17.20546268888528374 ) ) ;
#20897 = ORIENTED_EDGE ( 'NONE', *, *, #10800, .F. ) ;
#20898 = CARTESIAN_POINT ( 'NONE',  ( 131.1922820468854241, -4.999999999999982236, -19.40354224447947473 ) ) ;
#20899 = CARTESIAN_POINT ( 'NONE',  ( 21.79935899731381710, -1.430375723040585356, -13.25318265510616733 ) ) ;
#20900 = CARTESIAN_POINT ( 'NONE',  ( 11.06643561541932463, 17.63888289548684796, -17.56974948598543662 ) ) ;
#20901 = CARTESIAN_POINT ( 'NONE',  ( 35.24964364652129234, -20.84149066036063047, -20.16262864730545346 ) ) ;
#20902 = ORIENTED_EDGE ( 'NONE', *, *, #2495, .F. ) ;
#20903 = ORIENTED_EDGE ( 'NONE', *, *, #8493, .T. ) ;
#20904 = CARTESIAN_POINT ( 'NONE',  ( 9.916637298967875935, 16.40639221407973380, -16.50447193873893781 ) ) ;
#20905 = DIRECTION ( 'NONE',  ( -1.110223024625156540E-16, 0.000000000000000000, -1.000000000000000000 ) ) ;
#20906 = CARTESIAN_POINT ( 'NONE',  ( 12.75441094417786658, 7.625102360211175601, -14.92740490885063309 ) ) ;
#20907 = LINE ( 'NONE', #19, #6396 ) ;
#20908 = DIRECTION ( 'NONE',  ( -2.698458740408365879E-16, 1.000000000000000000, 0.000000000000000000 ) ) ;
#20909 = ORIENTED_EDGE ( 'NONE', *, *, #22070, .T. ) ;
#20910 = CARTESIAN_POINT ( 'NONE',  ( -13.00000000000000178, 1.592040838891559293E-15, 18.00000000000000000 ) ) ;
#20911 = EDGE_LOOP ( 'NONE', ( #28051, #27008, #10157, #17130 ) ) ;
#20912 = CARTESIAN_POINT ( 'NONE',  ( 10.35953768210033665, 16.96805026999784616, -17.84385765891457254 ) ) ;
#20913 = AXIS2_PLACEMENT_3D ( 'NONE', #27550, #9173, #22787 ) ;
#20914 = CARTESIAN_POINT ( 'NONE',  ( 36.21530066971708095, -20.68720585756345187, -20.37220581101806971 ) ) ;
#20915 = CARTESIAN_POINT ( 'NONE',  ( 25.26806593431409453, -8.821542497490490575, -18.05414547114721557 ) ) ;
#20916 = ORIENTED_EDGE ( 'NONE', *, *, #8530, .F. ) ;
#20917 = DIRECTION ( 'NONE',  ( 2.908569913943825061E-16, -1.000000000000000000, -6.826925868028081731E-18 ) ) ;
#20918 = VERTEX_POINT ( 'NONE', #28120 ) ;
#20919 = CARTESIAN_POINT ( 'NONE',  ( 3.999999999999999112, 0.7862748000878193588, -0.03447227762756639030 ) ) ;
#20920 = SHAPE_DEFINITION_REPRESENTATION ( #24215, #6235 ) ;
#20921 = EDGE_CURVE ( 'NONE', #288, #1987, #16471, .T. ) ;
#20922 = EDGE_CURVE ( 'NONE', #2898, #24422, #16628, .T. ) ;
#20923 = CARTESIAN_POINT ( 'NONE',  ( 19.59003110916602708, 6.792398362604423312, -16.15450529561476500 ) ) ;
#20924 = EDGE_CURVE ( 'NONE', #10096, #10263, #21650, .T. ) ;
#20925 = CARTESIAN_POINT ( 'NONE',  ( 30.71753525214919378, -10.10955902127019179, -14.92479911117869484 ) ) ;
#20926 = EDGE_CURVE ( 'NONE', #21764, #9008, #30051, .T. ) ;
#20927 = ORIENTED_EDGE ( 'NONE', *, *, #20579, .F. ) ;
#20928 = CARTESIAN_POINT ( 'NONE',  ( 153.6922820468854241, -10.00000000000000000, -26.58683881228715862 ) ) ;
#20929 = VERTEX_POINT ( 'NONE', #14174 ) ;
#20930 = DIRECTION ( 'NONE',  ( -0.9510565162951536422, 0.000000000000000000, -0.3090169943749472292 ) ) ;
#20931 = VECTOR ( 'NONE', #27493, 1000.000000000000000 ) ;
#20932 = CARTESIAN_POINT ( 'NONE',  ( 131.1922820468854241, -4.999999999999982236, -22.25671179336495697 ) ) ;
#20933 = EDGE_LOOP ( 'NONE', ( #8596, #4525 ) ) ;
#20934 = CARTESIAN_POINT ( 'NONE',  ( 133.6922820468854241, -10.00000000000000711, -6.413161187712875133 ) ) ;
#20935 = AXIS2_PLACEMENT_3D ( 'NONE', #4248, #4683, #18118 ) ;
#20936 = CARTESIAN_POINT ( 'NONE',  ( 10.72284644870490489, 16.62177094183959980, -15.95334970537801134 ) ) ;
#20937 = DIRECTION ( 'NONE',  ( 0.3090169943749472292, 8.338696094057992503E-17, -0.9510565162951536422 ) ) ;
#20938 = DIRECTION ( 'NONE',  ( 0.5877852522924731371, 1.586114251531760728E-16, 0.8090169943749474513 ) ) ;
#20939 = ORIENTED_EDGE ( 'NONE', *, *, #27764, .F. ) ;
#20940 = CARTESIAN_POINT ( 'NONE',  ( 11.14863080475985591, 10.75631295387255548, -15.99499920034263489 ) ) ;
#20941 = ORIENTED_EDGE ( 'NONE', *, *, #13786, .F. ) ;
#20942 = CARTESIAN_POINT ( 'NONE',  ( 17.65840769916877662, 9.384080434346836697, -15.74689851229248738 ) ) ;
#20943 = CARTESIAN_POINT ( 'NONE',  ( 156.1922820468853956, -1.999999999999974465, -22.25671179336496053 ) ) ;
#20944 = LINE ( 'NONE', #208, #30132 ) ;
#20945 = EDGE_LOOP ( 'NONE', ( #5747, #23651, #25696, #4526 ) ) ;
#20947 = ORIENTED_EDGE ( 'NONE', *, *, #2861, .T. ) ;
#20946 = CARTESIAN_POINT ( 'NONE',  ( 28.75197783424699693, -9.407057218516385433, -18.70835418409691542 ) ) ;
#20948 = EDGE_LOOP ( 'NONE', ( #29998, #15086, #8199, #23059, #22191 ) ) ;
#20949 = LINE ( 'NONE', #26156, #29124 ) ;
#20950 = CARTESIAN_POINT ( 'NONE',  ( 11.27582353004791216, 16.67860322824865449, -16.78467813988110890 ) ) ;
#20951 = CARTESIAN_POINT ( 'NONE',  ( 32.73840480032550460, -11.71477781474665925, -16.63156947497440541 ) ) ;
#20952 = CARTESIAN_POINT ( 'NONE',  ( 13.77718166750866224, 8.859676595473322536, -15.39100258941132715 ) ) ;
#20953 = EDGE_LOOP ( 'NONE', ( #26184, #8259, #16146, #24424 ) ) ;
#20954 = CARTESIAN_POINT ( 'NONE',  ( 2.928571428571432378, 1.300546971703755312E-15, 1.700000000000000178 ) ) ;
#20955 = CARTESIAN_POINT ( 'NONE',  ( 25.21061150575720333, -3.342243121390650717, -18.67481654970342930 ) ) ;
#20956 = ORIENTED_EDGE ( 'NONE', *, *, #19686, .T. ) ;
#20957 = STYLED_ITEM ( 'NONE', ( #15741 ), #6562 ) ;
#20958 = DIRECTION ( 'NONE',  ( 0.9510565162951536422, 2.566386769018988816E-16, 0.3090169943749472292 ) ) ;
#20959 =( NAMED_UNIT ( * ) PLANE_ANGLE_UNIT ( ) SI_UNIT ( $, .RADIAN. ) );
#20960 = VECTOR ( 'NONE', #5534, 1000.000000000000000 ) ;
#20961 = CARTESIAN_POINT ( 'NONE',  ( 21.44014932938603835, 4.813297736510089742, -15.98289606589226075 ) ) ;
#20962 = CARTESIAN_POINT ( 'NONE',  ( 16.24840684054896656, 4.149509756678782857, -16.79736725456322688 ) ) ;
#20963 = EDGE_CURVE ( 'NONE', #30260, #14083, #7475, .T. ) ;
#20964 = ADVANCED_FACE ( 'NONE', ( #25797 ), #23500, .T. ) ;
#20965 = VERTEX_POINT ( 'NONE', #26102 ) ;
#20966 = ORIENTED_EDGE ( 'NONE', *, *, #8459, .F. ) ;
#20967 = FACE_OUTER_BOUND ( 'NONE', #7971, .T. ) ;
#20968 = DIRECTION ( 'NONE',  ( 2.698458740408365879E-16, -1.000000000000000000, 0.000000000000000000 ) ) ;
#20969 = AXIS2_PLACEMENT_3D ( 'NONE', #30243, #18879, #16281 ) ;
#20970 = DIRECTION ( 'NONE',  ( 0.000000000000000000, 0.000000000000000000, 1.000000000000000000 ) ) ;
#20971 = DIRECTION ( 'NONE',  ( -1.110223024625156540E-16, 0.000000000000000000, -1.000000000000000000 ) ) ;
#20972 = VECTOR ( 'NONE', #28012, 999.9999999999998863 ) ;
#20973 = PLANE ( 'NONE',  #21156 ) ;
#20974 = CARTESIAN_POINT ( 'NONE',  ( 9.915248083523094280, 16.41276333319327918, -16.50506225043874409 ) ) ;
#20975 = CARTESIAN_POINT ( 'NONE',  ( 22.27366892561238387, -0.4200048385588530664, -12.54648181008633934 ) ) ;
#20976 = CARTESIAN_POINT ( 'NONE',  ( 23.76385019584477831, -1.264968635605209446, -19.12809044524397351 ) ) ;
#20978 = ORIENTED_EDGE ( 'NONE', *, *, #16410, .T. ) ;
#20977 = CARTESIAN_POINT ( 'NONE',  ( 36.53927379715840829, -23.14264550581856739, -18.86160504153442830 ) ) ;
#20980 = PRESENTATION_STYLE_ASSIGNMENT (( #6959 ) ) ;
#20979 = STYLED_ITEM ( 'NONE', ( #21906 ), #29596 ) ;
#20981 = FACE_OUTER_BOUND ( 'NONE', #19032, .T. ) ;
#20982 = CARTESIAN_POINT ( 'NONE',  ( 168.6922820468853672, -1.999999999999970912, -26.58683881228715862 ) ) ;
#20983 = DIRECTION ( 'NONE',  ( -2.698458740408365879E-16, 1.000000000000000000, 0.000000000000000000 ) ) ;
#20985 = ORIENTED_EDGE ( 'NONE', *, *, #20036, .F. ) ;
#20984 = CARTESIAN_POINT ( 'NONE',  ( 15.78240017141095741, 4.038647184180326200, -18.77507866864583619 ) ) ;
#20986 = ORIENTED_EDGE ( 'NONE', *, *, #26433, .F. ) ;
#20987 = DIRECTION ( 'NONE',  ( 0.9510565162951535312, 2.566386769018988816E-16, -0.3090169943749475623 ) ) ;
#20988 = CARTESIAN_POINT ( 'NONE',  ( 10.71678736308702362, 16.64955868083699997, -15.95594379117117434 ) ) ;
#20989 = EDGE_LOOP ( 'NONE', ( #3687, #26896, #26021, #19376 ) ) ;
#20990 = FACE_OUTER_BOUND ( 'NONE', #7831, .T. ) ;
#20991 = LINE ( 'NONE', #23751, #2031 ) ;
#20992 = CARTESIAN_POINT ( 'NONE',  ( 16.53304876882650731, 8.555045913257369961, -19.77053526944897754 ) ) ;
#20993 = ORIENTED_EDGE ( 'NONE', *, *, #7399, .T. ) ;
#20994 = CARTESIAN_POINT ( 'NONE',  ( 24.94601217299843654, -12.81575267032737742, -15.97323768315044035 ) ) ;
#20995 = ORIENTED_EDGE ( 'NONE', *, *, #25040, .F. ) ;
#20997 = AXIS2_PLACEMENT_3D ( 'NONE', #9406, #4841, #14139 ) ;
#20996 = CARTESIAN_POINT ( 'NONE',  ( 34.99076264053043417, -20.67847543353016349, -21.19169145379677488 ) ) ;
#20998 = CARTESIAN_POINT ( 'NONE',  ( 20.43449928165676965, -1.849542096390112356, -17.64764676960594869 ) ) ;
#20999 = VECTOR ( 'NONE', #10846, 1000.000000000000000 ) ;
#21000 = EDGE_CURVE ( 'NONE', #952, #3702, #2258, .T. ) ;
#21001 = CARTESIAN_POINT ( 'NONE',  ( 18.18682981270212196, 6.389142113859191952, -14.72334701657588063 ) ) ;
#21002 = EDGE_CURVE ( 'NONE', #26592, #11825, #3061, .T. ) ;
#21003 = ADVANCED_FACE ( 'NONE', ( #18920 ), #28273, .F. ) ;
#21004 = EDGE_CURVE ( 'NONE', #2921, #12148, #9441, .T. ) ;
#21005 = CARTESIAN_POINT ( 'NONE',  ( 30.09709056228524204, -9.598102759715754217, -17.07777997130633807 ) ) ;
#21006 = ADVANCED_FACE ( 'NONE', ( #28565 ), #748, .T. ) ;
#21007 = ORIENTED_EDGE ( 'NONE', *, *, #11512, .T. ) ;
#21008 = CARTESIAN_POINT ( 'NONE',  ( 0.000000000000000000, 0.000000000000000000, 9.999999999999998224 ) ) ;
#21010 = EDGE_LOOP ( 'NONE', ( #1305, #24019, #28489, #9483 ) ) ;
#21009 = CARTESIAN_POINT ( 'NONE',  ( 134.7287565553230024, -1.999999999999980460, -33.82050807568879947 ) ) ;
#21011 = EDGE_LOOP ( 'NONE', ( #11688, #15835, #9976, #24714 ) ) ;
#21012 = CARTESIAN_POINT ( 'NONE',  ( 132.0152310637605524, -4.999999999999982236, -0.06116980274991495881 ) ) ;
#21013 = VECTOR ( 'NONE', #14853, 1000.000000000000000 ) ;
#21014 = DIRECTION ( 'NONE',  ( -0.9510565162951536422, -2.566386769018988323E-16, 0.3090169943749475623 ) ) ;
#21015 = CARTESIAN_POINT ( 'NONE',  ( 36.54859390953724585, -21.18451583373416014, -17.22552805718784441 ) ) ;
#21016 = VECTOR ( 'NONE', #26500, 1000.000000000000000 ) ;
#21017 = CARTESIAN_POINT ( 'NONE',  ( 9.641485839925177714, 17.66827187890266160, -17.87200850766020110 ) ) ;
#21018 = ORIENTED_EDGE ( 'NONE', *, *, #11568, .F. ) ;
#21019 = DIRECTION ( 'NONE',  ( 0.3090169943749475623, 8.338696094058001131E-17, 0.9510565162951536422 ) ) ;
#21020 = LINE ( 'NONE', #125, #27035 ) ;
#21021 = CARTESIAN_POINT ( 'NONE',  ( 10.46722255365007115, 16.47419372244215197, -17.33720764016775462 ) ) ;
#21022 = DIRECTION ( 'NONE',  ( -1.000000000000000000, 0.000000000000000000, 0.000000000000000000 ) ) ;
#21023 = ORIENTED_EDGE ( 'NONE', *, *, #15588, .F. ) ;
#21024 = LINE ( 'NONE', #15264, #25140 ) ;
#21025 = ADVANCED_FACE ( 'NONE', ( #1941 ), #24522, .F. ) ;
#21026 = ORIENTED_EDGE ( 'NONE', *, *, #22317, .F. ) ;
#21027 = DIRECTION ( 'NONE',  ( 1.110223024625156540E-16, 2.995891024602366092E-32, 1.000000000000000000 ) ) ;
#21028 = ORIENTED_EDGE ( 'NONE', *, *, #5784, .T. ) ;
#21029 = PLANE ( 'NONE',  #9282 ) ;
#21030 = ORIENTED_EDGE ( 'NONE', *, *, #2009, .F. ) ;
#21031 = DIRECTION ( 'NONE',  ( -0.9510565162951536422, 0.000000000000000000, -0.3090169943749472292 ) ) ;
#21032 = ORIENTED_EDGE ( 'NONE', *, *, #15969, .F. ) ;
#21033 = CARTESIAN_POINT ( 'NONE',  ( 10.57561133056755942, 12.06435231892607618, -17.50969232694400546 ) ) ;
#21034 = CARTESIAN_POINT ( 'NONE',  ( 25.51539342332723947, -8.447981945391376257, -12.99903862581394876 ) ) ;
#21035 = CARTESIAN_POINT ( 'NONE',  ( 23.43490106394649430, 0.5024168867186777909, -19.39616715318824802 ) ) ;
#21036 = ORIENTED_EDGE ( 'NONE', *, *, #4611, .F. ) ;
#21037 = CARTESIAN_POINT ( 'NONE',  ( 18.12654306171327079, 0.8625984663607378922, -18.09208126113620452 ) ) ;
#21038 = DIRECTION ( 'NONE',  ( 0.5877852522924731371, 1.586114251531760728E-16, 0.8090169943749474513 ) ) ;
#21039 = CARTESIAN_POINT ( 'NONE',  ( 148.6922820468853672, -4.999999999999978684, -0.6060766987539614181 ) ) ;
#21040 = DIRECTION ( 'NONE',  ( 0.9510565162951535312, 2.566386769018988816E-16, -0.3090169943749475623 ) ) ;
#21041 = EDGE_CURVE ( 'NONE', #18400, #21232, #29612, .T. ) ;
#21042 = VECTOR ( 'NONE', #4178, 1000.000000000000000 ) ;
#21043 = CARTESIAN_POINT ( 'NONE',  ( 21.57856661146780652, -4.666631351218505586, -18.28211233923166645 ) ) ;
#21044 = ORIENTED_EDGE ( 'NONE', *, *, #8281, .T. ) ;
#21045 = CARTESIAN_POINT ( 'NONE',  ( 3.345653888883660443, -2.687187980154745137, -0.1391502195351530802 ) ) ;
#21046 = CARTESIAN_POINT ( 'NONE',  ( 0.000000000000000000, 0.000000000000000000, 18.00000000000000000 ) ) ;
#21047 = VECTOR ( 'NONE', #17435, 1000.000000000000000 ) ;
#21048 = DIRECTION ( 'NONE',  ( 0.9510565162951536422, 2.566386769018988816E-16, 0.3090169943749472292 ) ) ;
#21049 = CARTESIAN_POINT ( 'NONE',  ( 133.7287565553229456, -1.999999999999980904, 6.499999999999978684 ) ) ;
#21050 = CARTESIAN_POINT ( 'NONE',  ( 10.43477690885096720, 16.62299358534909288, -17.37687480348504820 ) ) ;
#21051 = DIRECTION ( 'NONE',  ( 0.9510565162951535312, 2.566386769018988816E-16, -0.3090169943749475623 ) ) ;
#21052 = CARTESIAN_POINT ( 'NONE',  ( 33.27037009343090546, -12.05169513820189309, -19.60996450177851713 ) ) ;
#21053 = EDGE_LOOP ( 'NONE', ( #14552, #20552 ) ) ;
#21054 = CARTESIAN_POINT ( 'NONE',  ( 8.944584764616054784, 16.95159238827779546, -17.91493351301869552 ) ) ;
#21055 = ORIENTED_EDGE ( 'NONE', *, *, #28844, .F. ) ;
#21056 = DIRECTION ( 'NONE',  ( -2.698458740408365879E-16, 1.000000000000000000, 0.000000000000000000 ) ) ;
#21057 = VECTOR ( 'NONE', #21338, 999.9999999999998863 ) ;
#21058 = CARTESIAN_POINT ( 'NONE',  ( 16.89369580670022941, 0.5033910033923695293, -17.32063897790030893 ) ) ;
#21059 = CARTESIAN_POINT ( 'NONE',  ( 11.35716248442908061, 16.30557241515140277, -16.75104082405111683 ) ) ;
#21060 = LINE ( 'NONE', #28569, #18497 ) ;
#21061 = VERTEX_POINT ( 'NONE', #1330 ) ;
#21062 = ADVANCED_FACE ( 'NONE', ( #10777 ), #8775, .T. ) ;
#21063 = ORIENTED_EDGE ( 'NONE', *, *, #4908, .T. ) ;
#21064 = CARTESIAN_POINT ( 'NONE',  ( 9.918725397012197575, 16.39681593027784956, -16.50360835092378409 ) ) ;
#21065 = CARTESIAN_POINT ( 'NONE',  ( 172.0152310637604671, -1.999999999999969580, -26.04193191628311155 ) ) ;
#21066 = CARTESIAN_POINT ( 'NONE',  ( 10.56508425215480074, 13.43253182900300402, -16.23631622730588830 ) ) ;
#21067 = CARTESIAN_POINT ( 'NONE',  ( 157.0152310637605240, -1.999999999999973577, -26.04193191628311155 ) ) ;
#21068 = DIRECTION ( 'NONE',  ( -2.698458740408365879E-16, 1.000000000000000000, 0.000000000000000000 ) ) ;
#21069 = VERTEX_POINT ( 'NONE', #12907 ) ;
#21070 = PLANE ( 'NONE',  #27672 ) ;
#21071 = ORIENTED_EDGE ( 'NONE', *, *, #19136, .F. ) ;
#21072 = CARTESIAN_POINT ( 'NONE',  ( 10.55304143273637330, 16.08061740358965253, -17.30129946959702281 ) ) ;
#21073 = ORIENTED_EDGE ( 'NONE', *, *, #7733, .F. ) ;
#21074 = CARTESIAN_POINT ( 'NONE',  ( 32.63927297112797277, -9.624974391992262568, -18.12286679007055312 ) ) ;
#21075 = CARTESIAN_POINT ( 'NONE',  ( 27.78884322698630882, -6.380937659459246625, -17.89340433249687834 ) ) ;
#21076 = AXIS2_PLACEMENT_3D ( 'NONE', #3979, #22597, #20591 ) ;
#21077 = VERTEX_POINT ( 'NONE', #6504 ) ;
#21078 = CARTESIAN_POINT ( 'NONE',  ( 159.5152310637605240, -1.999999999999972689, -30.37205893520531319 ) ) ;
#21079 = ORIENTED_EDGE ( 'NONE', *, *, #2786, .F. ) ;
#21080 = CARTESIAN_POINT ( 'NONE',  ( 33.36027191889437660, -10.38700102556154903, -18.15738432823107473 ) ) ;
#21081 = DIRECTION ( 'NONE',  ( 1.000000000000000000, 0.000000000000000000, 0.000000000000000000 ) ) ;
#21082 = CARTESIAN_POINT ( 'NONE',  ( 19.63213555404020383, 6.204410169219986670, -18.27402551702938638 ) ) ;
#21083 = CARTESIAN_POINT ( 'NONE',  ( 27.16844481176636350, -11.11852963900163438, -17.34443814838110143 ) ) ;
#21084 = AXIS2_PLACEMENT_3D ( 'NONE', #10644, #19954, #26543 ) ;
#21085 = EDGE_LOOP ( 'NONE', ( #9205, #1279, #29207, #998, #17854 ) ) ;
#21086 = FACE_BOUND ( 'NONE', #16672, .T. ) ;
#21087 = LINE ( 'NONE', #2043, #1360 ) ;
#21088 = LINE ( 'NONE', #16353, #1927 ) ;
#21089 = VECTOR ( 'NONE', #1698, 1000.000000000000000 ) ;
#21090 = CARTESIAN_POINT ( 'NONE',  ( 146.1922820468853956, -4.999999999999978684, -2.083034168790677043 ) ) ;
#21091 = CARTESIAN_POINT ( 'NONE',  ( 10.61946839964472034, 17.09587585246520902, -16.05247762654136068 ) ) ;
#21092 = DIRECTION ( 'NONE',  ( -0.9510565162951536422, -2.566386769018988323E-16, 0.3090169943749475623 ) ) ;
#21093 = ADVANCED_FACE ( 'NONE', ( #22540 ), #283, .T. ) ;
#21094 = EDGE_CURVE ( 'NONE', #15830, #5025, #3918, .T. ) ;
#21095 = LINE ( 'NONE', #5221, #19325 ) ;
#21096 = ORIENTED_EDGE ( 'NONE', *, *, #11030, .T. ) ;
#21097 = CARTESIAN_POINT ( 'NONE',  ( 11.31072706937237982, 10.01291882189198112, -15.92796669285280764 ) ) ;
#21098 = EDGE_CURVE ( 'NONE', #952, #22117, #5083, .T. ) ;
#21099 = ORIENTED_EDGE ( 'NONE', *, *, #16699, .T. ) ;
#21100 = VECTOR ( 'NONE', #8804, 999.9999999999998863 ) ;
#21101 = CARTESIAN_POINT ( 'NONE',  ( 17.82019932507133930, 1.781282266713458240, -14.47200660618688417 ) ) ;
#21102 = LINE ( 'NONE', #18510, #17080 ) ;
#21103 = DIRECTION ( 'NONE',  ( -2.698458740408365879E-16, 1.000000000000000000, 0.000000000000000000 ) ) ;
#21104 = CARTESIAN_POINT ( 'NONE',  ( 25.97851742199650005, -11.98992670343847244, -16.97112261376066655 ) ) ;
#21105 = ORIENTED_EDGE ( 'NONE', *, *, #20166, .F. ) ;
#21106 = CARTESIAN_POINT ( 'NONE',  ( 0.000000000000000000, 0.000000000000000000, -23.00000000000000000 ) ) ;
#21107 = CARTESIAN_POINT ( 'NONE',  ( 11.27605965875426541, 16.67752031190189399, -16.78457976421582742 ) ) ;
#21108 = ORIENTED_EDGE ( 'NONE', *, *, #28303, .T. ) ;
#21109 = CARTESIAN_POINT ( 'NONE',  ( 33.64261581855389949, -12.62196589562294591, -18.73949555988700055 ) ) ;
#21110 = DIRECTION ( 'NONE',  ( -1.000000000000000000, -2.908569913943825554E-16, 0.000000000000000000 ) ) ;
#21111 = ORIENTED_EDGE ( 'NONE', *, *, #19893, .F. ) ;
#21112 = LINE ( 'NONE', #218, #13996 ) ;
#21113 = CARTESIAN_POINT ( 'NONE',  ( 24.25137658470242386, -8.936440734373054084, -19.04774169986686161 ) ) ;
#21114 = VERTEX_POINT ( 'NONE', #29462 ) ;
#21115 = DIRECTION ( 'NONE',  ( 0.3090169943749475623, 8.338696094058001131E-17, 0.9510565162951536422 ) ) ;
#21116 = CARTESIAN_POINT ( 'NONE',  ( 21.63689124574611711, 4.661388338709377521, -16.95871344450652174 ) ) ;
#21117 = CARTESIAN_POINT ( 'NONE',  ( 16.52347908691095668, 7.282719431485021211, -19.45954596032283845 ) ) ;
#21118 = ORIENTED_EDGE ( 'NONE', *, *, #1590, .T. ) ;
#21119 = ORIENTED_EDGE ( 'NONE', *, *, #4123, .F. ) ;
#21120 = CARTESIAN_POINT ( 'NONE',  ( -2.928571428571429713, -9.419004090963149730E-16, 2.549999999999998490 ) ) ;
#21121 = VECTOR ( 'NONE', #3458, 1000.000000000000000 ) ;
#21122 = CARTESIAN_POINT ( 'NONE',  ( 134.7287565553230024, -10.00000000000000711, -25.16025403784439973 ) ) ;
#21123 = CARTESIAN_POINT ( 'NONE',  ( 168.6922820468853388, -9.999999999999996447, -15.07341522555727664 ) ) ;
#21124 = CARTESIAN_POINT ( 'NONE',  ( 164.5152310637604955, -4.999999999999973355, -1.826485974285146869E-14 ) ) ;
#21125 = FACE_OUTER_BOUND ( 'NONE', #29598, .T. ) ;
#21126 = CARTESIAN_POINT ( 'NONE',  ( 9.918725397012197575, 16.39681593027784956, -16.50360835092378409 ) ) ;
#21127 = CARTESIAN_POINT ( 'NONE',  ( 21.03482577225312156, -5.582666113748667058, -14.36824825895596014 ) ) ;
#21128 = CARTESIAN_POINT ( 'NONE',  ( 20.97149233804390533, -0.06858483505933390956, -19.21322127741759189 ) ) ;
#21129 = ADVANCED_FACE ( 'NONE', ( #17781 ), #27141, .T. ) ;
#21131 = EDGE_LOOP ( 'NONE', ( #10538, #29071, #6964, #25427 ) ) ;
#21130 = CARTESIAN_POINT ( 'NONE',  ( 31.86596522828317291, -10.28264332119880820, -18.16914504201997360 ) ) ;
#21132 = LINE ( 'NONE', #11507, #29080 ) ;
#21133 = CARTESIAN_POINT ( 'NONE',  ( 12.50481220565295004, 8.572828783776230921, -15.12633959982445653 ) ) ;
#21134 = EDGE_CURVE ( 'NONE', #8261, #28996, #1638, .T. ) ;
#21135 = DIRECTION ( 'NONE',  ( -2.698458740408365879E-16, 1.000000000000000000, 0.000000000000000000 ) ) ;
#21136 = CARTESIAN_POINT ( 'NONE',  ( 111.4790881585512494, -4.999999999999986677, 80.99429853044631500 ) ) ;
#21137 = EDGE_CURVE ( 'NONE', #27103, #9856, #6359, .T. ) ;
#21138 = CARTESIAN_POINT ( 'NONE',  ( 19.20291185354690811, 8.143073066566493878, -16.32372945079811188 ) ) ;
#21139 = DIRECTION ( 'NONE',  ( 1.000000000000000000, 2.698458740408365879E-16, -1.110223024625156540E-16 ) ) ;
#21140 = CARTESIAN_POINT ( 'NONE',  ( 10.35008142444812052, 18.33131885956999696, -17.43324812465761653 ) ) ;
#21141 = VERTEX_POINT ( 'NONE', #15190 ) ;
#21142 = CARTESIAN_POINT ( 'NONE',  ( 169.5152310637604955, -4.999999999999971578, -1.881997125516404696E-14 ) ) ;
#21143 = DIRECTION ( 'NONE',  ( 1.000000000000000000, 0.000000000000000000, 0.000000000000000000 ) ) ;
#21144 = CARTESIAN_POINT ( 'NONE',  ( 21.66440995182641416, 5.535554982823286174, -17.57621636221614025 ) ) ;
#21145 = CARTESIAN_POINT ( 'NONE',  ( 14.69524703049083492, 10.61837011038446654, -14.15659040230468690 ) ) ;
#21146 = ORIENTED_EDGE ( 'NONE', *, *, #13786, .T. ) ;
#21147 = CARTESIAN_POINT ( 'NONE',  ( 35.54859661768235668, -23.18452799999607805, -18.25366188177437365 ) ) ;
#21148 = CARTESIAN_POINT ( 'NONE',  ( 21.08246358516588259, -1.232126404925322438, -18.58940169363586037 ) ) ;
#21149 = CARTESIAN_POINT ( 'NONE',  ( 17.81405000127377747, 1.596365152898254980, -17.08637312321770096 ) ) ;
#21150 = CARTESIAN_POINT ( 'NONE',  ( 28.29154804861901340, -7.753790107393749409, -19.00671289252072782 ) ) ;
#21151 = VERTEX_POINT ( 'NONE', #15339 ) ;
#21152 = CARTESIAN_POINT ( 'NONE',  ( 81.91613614387523512, -4.999999999999995559, 59.51555663840242261 ) ) ;
#21154 = ORIENTED_EDGE ( 'NONE', *, *, #13686, .F. ) ;
#21153 = DIRECTION ( 'NONE',  ( 0.3090169943749472292, 8.338696094057992503E-17, -0.9510565162951536422 ) ) ;
#21155 = FACE_OUTER_BOUND ( 'NONE', #69, .T. ) ;
#21156 = AXIS2_PLACEMENT_3D ( 'NONE', #6801, #9362, #2229 ) ;
#21157 = CARTESIAN_POINT ( 'NONE',  ( 157.0152310637605524, -1.999999999999973577, -24.27857615940569502 ) ) ;
#21158 = CARTESIAN_POINT ( 'NONE',  ( 33.19592593216645326, -10.35933293216661610, -17.69446280125821147 ) ) ;
#21159 = CARTESIAN_POINT ( 'NONE',  ( 13.19155076956097083, 7.818281081198240834, -14.57899684263624351 ) ) ;
#21160 = ORIENTED_EDGE ( 'NONE', *, *, #16064, .F. ) ;
#21161 = EDGE_CURVE ( 'NONE', #21674, #23858, #4067, .T. ) ;
#21162 = CARTESIAN_POINT ( 'NONE',  ( 157.0152310637604671, -10.00000000000000000, 1.702185954127501066 ) ) ;
#21163 = CARTESIAN_POINT ( 'NONE',  ( 172.7287565553229456, -9.999999999999971578, -36.50000000000000711 ) ) ;
#21164 = EDGE_CURVE ( 'NONE', #8863, #9240, #29298, .T. ) ;
#21165 = AXIS2_PLACEMENT_3D ( 'NONE', #28767, #27345, #12681 ) ;
#21166 = EDGE_CURVE ( 'NONE', #5527, #28746, #13510, .T. ) ;
#21167 = CARTESIAN_POINT ( 'NONE',  ( 10.53683180627515981, 16.15495681678771689, -17.30800272034635867 ) ) ;
#21168 = LINE ( 'NONE', #18585, #24396 ) ;
#21169 = EDGE_CURVE ( 'NONE', #3207, #968, #11225, .T. ) ;
#21170 = PLANE ( 'NONE',  #8133 ) ;
#21171 = EDGE_LOOP ( 'NONE', ( #18182, #24874, #6727, #9457 ) ) ;
#21172 = DIRECTION ( 'NONE',  ( 1.000000000000000000, 4.440892098500622217E-16, 0.000000000000000000 ) ) ;
#21173 = CARTESIAN_POINT ( 'NONE',  ( 134.5152310637605808, -1.999999999999980460, -2.627941064794695691 ) ) ;
#21174 = ORIENTED_EDGE ( 'NONE', *, *, #713, .T. ) ;
#21175 = FACE_OUTER_BOUND ( 'NONE', #1867, .T. ) ;
#21176 = VERTEX_POINT ( 'NONE', #29913 ) ;
#21177 = CARTESIAN_POINT ( 'NONE',  ( 9.667369220937283458, 16.22966640763102220, -17.88537093449073012 ) ) ;
#21178 = ORIENTED_EDGE ( 'NONE', *, *, #8690, .T. ) ;
#21179 = CARTESIAN_POINT ( 'NONE',  ( 26.12748305362656254, -5.066878407431925524, -14.17679521427828071 ) ) ;
#21180 = CARTESIAN_POINT ( 'NONE',  ( 21.81760893248375766, -3.923850722439390815, -13.93537712798182682 ) ) ;
#21181 = CARTESIAN_POINT ( 'NONE',  ( 146.1922820468854525, -1.999999999999976685, -28.06379628232387446 ) ) ;
#21182 = CARTESIAN_POINT ( 'NONE',  ( -3.660532965668823913, 7.124194613927632425, -2.285083133455287951E-15 ) ) ;
#21183 = AXIS2_PLACEMENT_3D ( 'NONE', #26951, #20330, #29717 ) ;
#21184 = DIRECTION ( 'NONE',  ( -0.8090169943749474513, -2.183098979609982436E-16, -0.5877852522924731371 ) ) ;
#21185 = CARTESIAN_POINT ( 'NONE',  ( 25.73595588610537277, -4.826321120321507507, -18.84379041344559269 ) ) ;
#21186 = ORIENTED_EDGE ( 'NONE', *, *, #28106, .F. ) ;
#21187 = CARTESIAN_POINT ( 'NONE',  ( 100.1455277581281536, -4.999999999999990230, -72.75998490582146871 ) ) ;
#21188 = DIRECTION ( 'NONE',  ( -2.698458740408365879E-16, 1.000000000000000000, 0.000000000000000000 ) ) ;
#21189 = DIRECTION ( 'NONE',  ( 0.000000000000000000, 0.000000000000000000, -1.000000000000000000 ) ) ;
#21190 = DIRECTION ( 'NONE',  ( 0.3090169943749472292, 8.338696094057992503E-17, -0.9510565162951536422 ) ) ;
#21191 = DIRECTION ( 'NONE',  ( 0.5877852522924731371, 0.000000000000000000, 0.8090169943749474513 ) ) ;
#21192 = CARTESIAN_POINT ( 'NONE',  ( 11.86602117609799301, 10.05912493454434120, -16.75833615892761586 ) ) ;
#21193 = FACE_BOUND ( 'NONE', #24930, .T. ) ;
#21194 = CARTESIAN_POINT ( 'NONE',  ( 32.57315965809380742, -11.03986597812349935, -18.16622079659612510 ) ) ;
#21195 = CARTESIAN_POINT ( 'NONE',  ( 13.37966566800644763, 7.625977406171305262, -15.70782985742499527 ) ) ;
#21196 = ORIENTED_EDGE ( 'NONE', *, *, #29954, .T. ) ;
#21197 = ADVANCED_FACE ( 'NONE', ( #1488 ), #10622, .T. ) ;
#21198 = DIRECTION ( 'NONE',  ( -2.698458740408365879E-16, 1.000000000000000000, 0.000000000000000000 ) ) ;
#21199 = AXIS2_PLACEMENT_3D ( 'NONE', #29375, #8248, #17848 ) ;
#21200 = CARTESIAN_POINT ( 'NONE',  ( 23.16390915794477223, 2.882539813099532555, -14.99485278278146438 ) ) ;
#21201 = EDGE_CURVE ( 'NONE', #16627, #20539, #28203, .T. ) ;
#21202 = CARTESIAN_POINT ( 'NONE',  ( 11.27643094638968613, 16.67581753947769130, -16.78442615493024803 ) ) ;
#21203 = FACE_BOUND ( 'NONE', #3879, .T. ) ;
#21204 = EDGE_CURVE ( 'NONE', #2119, #6518, #21132, .T. ) ;
#21205 = ORIENTED_EDGE ( 'NONE', *, *, #15479, .F. ) ;
#21206 = ORIENTED_EDGE ( 'NONE', *, *, #25417, .F. ) ;
#21207 = CARTESIAN_POINT ( 'NONE',  ( 9.641351654859628084, 17.66888726871794191, -17.91235298298990841 ) ) ;
#21208 = CARTESIAN_POINT ( 'NONE',  ( 139.5152310637605808, -10.00000000000000533, -13.05155085951651195 ) ) ;
#21209 = CARTESIAN_POINT ( 'NONE',  ( 9.916411867603999397, 16.40742607105030260, -16.50456570466356965 ) ) ;
#21210 = CARTESIAN_POINT ( 'NONE',  ( 0.2500000000000002220, 4.898587196589412829E-16, -4.000000000000000000 ) ) ;
#21211 = LINE ( 'NONE', #27980, #21325 ) ;
#21212 = ORIENTED_EDGE ( 'NONE', *, *, #23242, .F. ) ;
#21213 = ORIENTED_EDGE ( 'NONE', *, *, #25976, .T. ) ;
#21214 = CARTESIAN_POINT ( 'NONE',  ( 153.6922820468853104, -1.999999999999975797, 2.247092850131521491 ) ) ;
#21215 = ORIENTED_EDGE ( 'NONE', *, *, #2351, .F. ) ;
#21216 = CARTESIAN_POINT ( 'NONE',  ( 10.47249985125707106, 16.44999136291752251, -17.33460624675630513 ) ) ;
#21217 = ORIENTED_EDGE ( 'NONE', *, *, #25073, .F. ) ;
#21218 = CARTESIAN_POINT ( 'NONE',  ( 32.68023997084922883, -9.631188006280016367, -18.23865791264771730 ) ) ;
#21219 = CARTESIAN_POINT ( 'NONE',  ( 16.68567729567724456, 11.07888045854852876, -16.17353378320854418 ) ) ;
#21220 = CARTESIAN_POINT ( 'NONE',  ( 24.36497833745277930, -6.082191617938494055, -18.74521747929614435 ) ) ;
#21221 = ORIENTED_EDGE ( 'NONE', *, *, #29241, .T. ) ;
#21222 = CARTESIAN_POINT ( 'NONE',  ( -31.74999999999995737, 5.204748896376250699E-16, -4.250000000000000000 ) ) ;
#21223 = CARTESIAN_POINT ( 'NONE',  ( 34.49115424338278046, -12.94152926980570939, -19.96804914223585925 ) ) ;
#21224 = DIRECTION ( 'NONE',  ( 0.000000000000000000, 0.000000000000000000, 1.000000000000000000 ) ) ;
#21225 = CARTESIAN_POINT ( 'NONE',  ( 31.88113401528661939, -11.03952345999570639, -14.96145667752709585 ) ) ;
#21226 = CARTESIAN_POINT ( 'NONE',  ( 16.53342136567307108, 10.04554801986687629, -15.32032680638607047 ) ) ;
#21227 = STYLED_ITEM ( 'NONE', ( #23127 ), #21281 ) ;
#21228 = ORIENTED_EDGE ( 'NONE', *, *, #2179, .T. ) ;
#21229 = EDGE_CURVE ( 'NONE', #29062, #16025, #25422, .T. ) ;
#21230 = FACE_BOUND ( 'NONE', #28952, .T. ) ;
#21231 = MANIFOLD_SOLID_BREP ( 'Cut-Extrude1', #8718 ) ;
#21232 = VERTEX_POINT ( 'NONE', #16557 ) ;
#21233 = AXIS2_PLACEMENT_3D ( 'NONE', #15342, #10921, #10625 ) ;
#21234 = CARTESIAN_POINT ( 'NONE',  ( 167.0152310637604387, -9.999999999999998224, 1.702185954127501066 ) ) ;
#21235 = CARTESIAN_POINT ( 'NONE',  ( 157.0152310637605524, -1.999999999999973577, -24.27857615940569502 ) ) ;
#21236 = DIRECTION ( 'NONE',  ( -0.9510565162951536422, -2.566386769018988816E-16, -0.3090169943749472292 ) ) ;
#21237 = VECTOR ( 'NONE', #27351, 1000.000000000000000 ) ;
#21238 = CARTESIAN_POINT ( 'NONE',  ( 10.70471194873291410, 16.70493807032227451, -15.96226385378574264 ) ) ;
#21239 = LINE ( 'NONE', #201, #22920 ) ;
#21240 = ORIENTED_EDGE ( 'NONE', *, *, #1242, .T. ) ;
#21241 = DIRECTION ( 'NONE',  ( -0.000000000000000000, 0.000000000000000000, 1.000000000000000000 ) ) ;
#21242 = ORIENTED_EDGE ( 'NONE', *, *, #27363, .T. ) ;
#21243 = AXIS2_PLACEMENT_3D ( 'NONE', #5425, #24054, #11671 ) ;
#21244 = CARTESIAN_POINT ( 'NONE',  ( 9.916336358462064737, 16.40777236560037622, -16.50459729666445696 ) ) ;
#21245 = ORIENTED_EDGE ( 'NONE', *, *, #2895, .F. ) ;
#21246 = CARTESIAN_POINT ( 'NONE',  ( 9.667821753224751902, 16.22759103687616999, -17.88509611560606061 ) ) ;
#21247 = VECTOR ( 'NONE', #10378, 1000.000000000000000 ) ;
#21248 = CARTESIAN_POINT ( 'NONE',  ( 21.18694592818775746, 3.276320881159561438, -13.81383015674761339 ) ) ;
#21249 = FACE_OUTER_BOUND ( 'NONE', #4400, .T. ) ;
#21250 = DIRECTION ( 'NONE',  ( -1.000000000000000000, 0.000000000000000000, -0.000000000000000000 ) ) ;
#21251 = CARTESIAN_POINT ( 'NONE',  ( 29.46565128511723586, -7.689737916804423534, -14.82739468409561567 ) ) ;
#21252 = ORIENTED_EDGE ( 'NONE', *, *, #2594, .F. ) ;
#21253 = LINE ( 'NONE', #7075, #6664 ) ;
#21254 = CARTESIAN_POINT ( 'NONE',  ( 11.27378865171844602, 16.68793543965420767, -16.78556983912737621 ) ) ;
#21255 = VERTEX_POINT ( 'NONE', #25883 ) ;
#21256 = CARTESIAN_POINT ( 'NONE',  ( 35.54859390953724585, -21.18451583373416014, -17.22552805718784441 ) ) ;
#21257 = CARTESIAN_POINT ( 'NONE',  ( 17.54642605795894994, 9.676486402519270058, -18.74681543856335608 ) ) ;
#21258 = CARTESIAN_POINT ( 'NONE',  ( 172.7287565553229456, -9.999999999999971578, -33.50000000000000000 ) ) ;
#21259 = CARTESIAN_POINT ( 'NONE',  ( 22.23398510282979146, -6.138177547518383292, -17.55864386164050472 ) ) ;
#21260 = ORIENTED_EDGE ( 'NONE', *, *, #6342, .F. ) ;
#21261 = LINE ( 'NONE', #18822, #8602 ) ;
#21262 = CARTESIAN_POINT ( 'NONE',  ( 20.29352232415978463, 1.537418251635638944, -14.27211978419980021 ) ) ;
#21263 = CARTESIAN_POINT ( 'NONE',  ( 15.22094575638775282, 5.866722348926807662, -16.67377462076821715 ) ) ;
#21264 = AXIS2_PLACEMENT_3D ( 'NONE', #12579, #8600, #26810 ) ;
#21265 = ORIENTED_EDGE ( 'NONE', *, *, #17365, .T. ) ;
#21266 = ADVANCED_FACE ( 'NONE', ( #4961 ), #6614, .T. ) ;
#21267 = LINE ( 'NONE', #14541, #1490 ) ;
#21268 = AXIS2_PLACEMENT_3D ( 'NONE', #9001, #1877, #20306 ) ;
#21269 = EDGE_CURVE ( 'NONE', #19490, #10978, #12461, .T. ) ;
#21270 = VECTOR ( 'NONE', #4715, 1000.000000000000000 ) ;
#21271 = CARTESIAN_POINT ( 'NONE',  ( 164.5152310637604387, -9.999999999999998224, -4.391296821672111328 ) ) ;
#21272 = DIRECTION ( 'NONE',  ( -0.8090169943749474513, -2.183098979609982436E-16, 0.5877852522924731371 ) ) ;
#21273 = LINE ( 'NONE', #7251, #20392 ) ;
#21274 = LINE ( 'NONE', #384, #26087 ) ;
#21275 = CARTESIAN_POINT ( 'NONE',  ( 9.924804006935172396, 16.36893865032855899, -16.50109463189289016 ) ) ;
#21276 = CARTESIAN_POINT ( 'NONE',  ( 20.97462796522363959, -1.010871063906457534, -12.65628865346789134 ) ) ;
#21277 = CARTESIAN_POINT ( 'NONE',  ( 22.98323032518889519, 2.094654362561221284, -17.51695658672324640 ) ) ;
#21278 = ADVANCED_FACE ( 'NONE', ( #23582 ), #24664, .T. ) ;
#21280 = ORIENTED_EDGE ( 'NONE', *, *, #24076, .T. ) ;
#21279 = CARTESIAN_POINT ( 'NONE',  ( 31.96909791962396596, -10.29830001063286460, -18.46063605759182735 ) ) ;
#21281 = MANIFOLD_SOLID_BREP ( 'Cut-Extrude1', #22883 ) ;
#21282 = CARTESIAN_POINT ( 'NONE',  ( 154.5152310637605524, -4.999999999999976019, -19.94844914048349693 ) ) ;
#21283 = CIRCLE ( 'NONE', #28629, 8.000000000000005329 ) ;
#21284 = LINE ( 'NONE', #28361, #7866 ) ;
#21285 = LINE ( 'NONE', #14709, #20727 ) ;
#21286 = CARTESIAN_POINT ( 'NONE',  ( 16.01392728624657025, 9.853228751548474662, -15.03783782146776105 ) ) ;
#21287 = ORIENTED_EDGE ( 'NONE', *, *, #9758, .T. ) ;
#21288 = PLANE ( 'NONE',  #25626 ) ;
#21289 = CARTESIAN_POINT ( 'NONE',  ( 10.71920666609040573, 16.63846344887410922, -15.95486870256106648 ) ) ;
#21290 = ORIENTED_EDGE ( 'NONE', *, *, #1109, .F. ) ;
#21291 = AXIS2_PLACEMENT_3D ( 'NONE', #4850, #6860, #9722 ) ;
#21292 = DIRECTION ( 'NONE',  ( 1.000000000000000000, 2.698458740408365879E-16, -1.110223024625156540E-16 ) ) ;
#21293 = DIRECTION ( 'NONE',  ( -0.9510565162951536422, -2.566386769018988323E-16, 0.3090169943749475623 ) ) ;
#21294 = ORIENTED_EDGE ( 'NONE', *, *, #8271, .F. ) ;
#21295 = VECTOR ( 'NONE', #23782, 1000.000000000000000 ) ;
#21296 = CARTESIAN_POINT ( 'NONE',  ( 21.48529164538665981, 5.106035544247377267, -18.65531623833433628 ) ) ;
#21297 = ORIENTED_EDGE ( 'NONE', *, *, #17622, .T. ) ;
#21298 = CARTESIAN_POINT ( 'NONE',  ( 15.41439956623108642, 10.93483300904300215, -14.25553973300288568 ) ) ;
#21299 = ORIENTED_EDGE ( 'NONE', *, *, #5086, .T. ) ;
#21300 = CARTESIAN_POINT ( 'NONE',  ( 32.57315965809380742, -11.03986597812349935, -18.16622079659612510 ) ) ;
#21301 = CARTESIAN_POINT ( 'NONE',  ( 21.34664435287406903, -1.670712410592182895, -14.88600020661825063 ) ) ;
#21302 = CARTESIAN_POINT ( 'NONE',  ( 18.08386662754633534, 1.890959213400748684, -17.98613275626550134 ) ) ;
#21303 = CARTESIAN_POINT ( 'NONE',  ( 27.67597367917761630, -6.185689562215541670, -12.94745500973225383 ) ) ;
#21304 = EDGE_CURVE ( 'NONE', #11783, #27678, #19001, .T. ) ;
#21305 = ADVANCED_FACE ( 'NONE', ( #13800 ), #2090, .T. ) ;
#21306 = EDGE_CURVE ( 'NONE', #16265, #10263, #7700, .T. ) ;
#21307 = ORIENTED_EDGE ( 'NONE', *, *, #21448, .T. ) ;
#21308 = EDGE_CURVE ( 'NONE', #28060, #25015, #16857, .T. ) ;
#21309 = CARTESIAN_POINT ( 'NONE',  ( 175.7287565553229172, -4.999999999999970690, -30.76635726929469783 ) ) ;
#21310 = LINE ( 'NONE', #26060, #27788 ) ;
#21311 = LINE ( 'NONE', #28231, #2666 ) ;
#21312 = PLANE ( 'NONE',  #20460 ) ;
#21313 = CARTESIAN_POINT ( 'NONE',  ( 35.14511844984765787, -14.87944403499761670, -19.12340528518704730 ) ) ;
#21314 = CARTESIAN_POINT ( 'NONE',  ( 9.641351654859628084, 17.66888726871794191, -17.91235298298990841 ) ) ;
#21315 = ORIENTED_EDGE ( 'NONE', *, *, #17481, .T. ) ;
#21316 = LINE ( 'NONE', #21162, #5915 ) ;
#21317 = DIRECTION ( 'NONE',  ( -0.5877852522924731371, -1.586114251531760235E-16, 0.8090169943749474513 ) ) ;
#21318 = CARTESIAN_POINT ( 'NONE',  ( 12.02786405831828986, 9.316892843345049968, -16.69140843421181231 ) ) ;
#21319 = CARTESIAN_POINT ( 'NONE',  ( 175.7287565553229456, -4.999999999999970690, -30.76635726929468362 ) ) ;
#21320 = VERTEX_POINT ( 'NONE', #21591 ) ;
#21321 = DIRECTION ( 'NONE',  ( -0.9510565162951536422, 0.000000000000000000, -0.3090169943749472292 ) ) ;
#21322 = EDGE_LOOP ( 'NONE', ( #2808, #12916, #3338, #21023 ) ) ;
#21323 = VERTEX_POINT ( 'NONE', #12125 ) ;
#21324 = CARTESIAN_POINT ( 'NONE',  ( 151.1922820468854241, -10.00000000000000178, -19.40354224447947828 ) ) ;
#21325 = VECTOR ( 'NONE', #23360, 1000.000000000000000 ) ;
#21326 = PLANE ( 'NONE',  #15610 ) ;
#21327 = ORIENTED_EDGE ( 'NONE', *, *, #2615, .T. ) ;
#21328 = DIRECTION ( 'NONE',  ( -0.5877852522924731371, -1.586114251531760235E-16, 0.8090169943749474513 ) ) ;
#21329 = ORIENTED_EDGE ( 'NONE', *, *, #1458, .F. ) ;
#21330 = CARTESIAN_POINT ( 'NONE',  ( 9.667746079407143256, 16.22793808664985704, -17.88513208046981617 ) ) ;
#21331 = EDGE_CURVE ( 'NONE', #25891, #30082, #24165, .T. ) ;
#21332 = EDGE_LOOP ( 'NONE', ( #7650, #20468, #7792, #3636 ) ) ;
#21333 = VECTOR ( 'NONE', #28935, 1000.000000000000000 ) ;
#21334 = CARTESIAN_POINT ( 'NONE',  ( 26.63310354640557520, -6.268104337495945977, -18.78393408973622769 ) ) ;
#21335 = CARTESIAN_POINT ( 'NONE',  ( 19.55718041265476970, -1.390565517676688900, -17.79492730709450754 ) ) ;
#21336 = CARTESIAN_POINT ( 'NONE',  ( 143.6922820468854525, -1.999999999999978018, -35.24709285013155835 ) ) ;
#21337 = LINE ( 'NONE', #28407, #16500 ) ;
#21338 = DIRECTION ( 'NONE',  ( -0.9510565162951536422, -2.566386769018988323E-16, 0.3090169943749475623 ) ) ;
#21339 = CARTESIAN_POINT ( 'NONE',  ( 26.47492910780048447, -3.130564378024159211, -15.09640780237150892 ) ) ;
#21340 = EDGE_CURVE ( 'NONE', #13044, #25090, #26035, .T. ) ;
#21341 = EDGE_CURVE ( 'NONE', #27148, #28119, #23900, .T. ) ;
#21342 = ADVANCED_FACE ( 'NONE', ( #21887 ), #17345, .T. ) ;
#21343 = DIRECTION ( 'NONE',  ( 6.938893903907227392E-16, -0.000000000000000000, 1.000000000000000000 ) ) ;
#21344 = EDGE_CURVE ( 'NONE', #27863, #15139, #18793, .T. ) ;
#21345 = FACE_OUTER_BOUND ( 'NONE', #21752, .T. ) ;
#21346 = CARTESIAN_POINT ( 'NONE',  ( 172.0152310637604671, -4.999999999999970690, -15.61832212156129707 ) ) ;
#21347 = VECTOR ( 'NONE', #9608, 1000.000000000000000 ) ;
#21348 = DIRECTION ( 'NONE',  ( 1.000000000000000000, 0.000000000000000000, 0.000000000000000000 ) ) ;
#21349 = FACE_BOUND ( 'NONE', #20933, .T. ) ;
#21350 = CARTESIAN_POINT ( 'NONE',  ( 10.47187086816178159, 16.45287595956923354, -17.33486661187913214 ) ) ;
#21351 = LINE ( 'NONE', #9895, #16989 ) ;
#21352 = CARTESIAN_POINT ( 'NONE',  ( 34.82539348385352440, -18.93555941106099993, -20.13934242161363741 ) ) ;
#21353 = AXIS2_PLACEMENT_3D ( 'NONE', #25181, #27648, #2147 ) ;
#21354 = EDGE_LOOP ( 'NONE', ( #20400, #14349, #28188, #10513 ) ) ;
#21355 = CARTESIAN_POINT ( 'NONE',  ( 13.37103985619203783, 7.622196798368539028, -15.71470239503888422 ) ) ;
#21356 = ORIENTED_EDGE ( 'NONE', *, *, #155, .T. ) ;
#21357 = DIRECTION ( 'NONE',  ( 0.000000000000000000, 0.000000000000000000, 1.000000000000000000 ) ) ;
#21358 = CARTESIAN_POINT ( 'NONE',  ( 19.02541433733466647, 1.263421280649871248, -13.57496312174407826 ) ) ;
#21359 = CARTESIAN_POINT ( 'NONE',  ( 12.83227841057820484, 9.540504573332061256, -16.14102835882348330 ) ) ;
#21360 = CARTESIAN_POINT ( 'NONE',  ( 159.5152310637604671, -1.999999999999973577, -13.05155085951651195 ) ) ;
#21361 = ORIENTED_EDGE ( 'NONE', *, *, #1376, .F. ) ;
#21362 = CARTESIAN_POINT ( 'NONE',  ( 11.47250673971808688, 9.270976631574885829, -15.86106510822916249 ) ) ;
#21363 = DIRECTION ( 'NONE',  ( -2.698458740408365879E-16, 1.000000000000000000, 0.000000000000000000 ) ) ;
#21364 = CARTESIAN_POINT ( 'NONE',  ( 10.17605321708455257, 15.21667774575863419, -16.39719424528293246 ) ) ;
#21365 = DIRECTION ( 'NONE',  ( -0.5877852522924731371, -1.586114251531760235E-16, 0.8090169943749474513 ) ) ;
#21366 = VERTEX_POINT ( 'NONE', #17301 ) ;
#21367 = CARTESIAN_POINT ( 'NONE',  ( 5.690023276062400548, 5.952467836904161480, -0.1306530452038157097 ) ) ;
#21368 = ORIENTED_EDGE ( 'NONE', *, *, #21201, .T. ) ;
#21369 = CARTESIAN_POINT ( 'NONE',  ( 10.35873811938078504, 16.97171716655003593, -17.89325570535168453 ) ) ;
#21370 = EDGE_LOOP ( 'NONE', ( #11901, #71, #18626, #11145 ) ) ;
#21371 = CARTESIAN_POINT ( 'NONE',  ( 34.01601630636088913, -11.85276864474937852, -20.84012540857256823 ) ) ;
#21372 = CARTESIAN_POINT ( 'NONE',  ( 27.11191462667604313, -11.78482644060662743, -13.28705938033944989 ) ) ;
#21373 = CARTESIAN_POINT ( 'NONE',  ( 31.59793210864275537, -10.01186915388335485, -14.42687813506083039 ) ) ;
#21374 = VERTEX_POINT ( 'NONE', #21439 ) ;
#21375 = EDGE_LOOP ( 'NONE', ( #2220, #15828, #6536, #6093, #23907 ) ) ;
#21376 = FACE_OUTER_BOUND ( 'NONE', #7453, .T. ) ;
#21377 = ORIENTED_EDGE ( 'NONE', *, *, #26644, .T. ) ;
#21378 = CARTESIAN_POINT ( 'NONE',  ( 177.2287565553228887, -9.999999999999994671, -20.83012701892220520 ) ) ;
#21379 = DIRECTION ( 'NONE',  ( 1.000000000000000000, 0.000000000000000000, 0.000000000000000000 ) ) ;
#21380 = CARTESIAN_POINT ( 'NONE',  ( 28.35369828010231785, -12.30166555976806464, -13.00196782638265169 ) ) ;
#21381 = VECTOR ( 'NONE', #20395, 1000.000000000000000 ) ;
#21382 = CARTESIAN_POINT ( 'NONE',  ( 15.73644607668725826, 9.740111719757674535, -14.94734896276200153 ) ) ;
#21383 = ADVANCED_FACE ( 'NONE', ( #22042 ), #24191, .T. ) ;
#21384 = EDGE_CURVE ( 'NONE', #16793, #30188, #23219, .T. ) ;
#21385 = EDGE_CURVE ( 'NONE', #16231, #486, #19588, .T. ) ;
#21386 = AXIS2_PLACEMENT_3D ( 'NONE', #11011, #19642, #3047 ) ;
#21388 = ORIENTED_EDGE ( 'NONE', *, *, #25451, .F. ) ;
#21387 = EDGE_CURVE ( 'NONE', #13253, #3275, #3144, .T. ) ;
#21389 = FACE_BOUND ( 'NONE', #14516, .T. ) ;
#21390 = AXIS2_PLACEMENT_3D ( 'NONE', #9370, #89, #7259 ) ;
#21391 = ORIENTED_EDGE ( 'NONE', *, *, #9165, .T. ) ;
#21392 = DIRECTION ( 'NONE',  ( 0.9510565162951536422, 2.566386769018988816E-16, 0.3090169943749472292 ) ) ;
#21393 = CARTESIAN_POINT ( 'NONE',  ( 167.0152310637604387, -4.999999999999972466, -1.854241549900775151E-14 ) ) ;
#21394 = LINE ( 'NONE', #14052, #25309 ) ;
#21395 = LINE ( 'NONE', #21688, #12902 ) ;
#21396 = CARTESIAN_POINT ( 'NONE',  ( 10.72145343393089512, 16.62815948516130504, -15.95392576598924350 ) ) ;
#21397 = CARTESIAN_POINT ( 'NONE',  ( 169.5152310637605240, -9.999999999999994671, -28.60870317832789667 ) ) ;
#21398 = ORIENTED_EDGE ( 'NONE', *, *, #6022, .T. ) ;
#21399 = VECTOR ( 'NONE', #14658, 1000.000000000000000 ) ;
#21400 = CARTESIAN_POINT ( 'NONE',  ( 147.0152310637606092, -1.999999999999976241, -24.27857615940569502 ) ) ;
#21401 = ORIENTED_EDGE ( 'NONE', *, *, #10659, .F. ) ;
#21402 = CARTESIAN_POINT ( 'NONE',  ( 9.924804006935172396, 16.36893865032855899, -16.50109463189289016 ) ) ;
#21403 = ORIENTED_EDGE ( 'NONE', *, *, #10939, .T. ) ;
#21404 = CARTESIAN_POINT ( 'NONE',  ( 18.10326352236751646, 1.905885860032081158, -14.21403189877281825 ) ) ;
#21405 = LINE ( 'NONE', #28925, #14127 ) ;
#21406 = DIRECTION ( 'NONE',  ( 1.000000000000000000, 0.000000000000000000, 0.000000000000000000 ) ) ;
#21407 = CARTESIAN_POINT ( 'NONE',  ( 26.08768104250457753, -11.87935956797728210, -17.28510650846989805 ) ) ;
#21408 = VECTOR ( 'NONE', #21189, 1000.000000000000000 ) ;
#21409 = CARTESIAN_POINT ( 'NONE',  ( 15.00000000000000000, 0.000000000000000000, 0.000000000000000000 ) ) ;
#21410 = CARTESIAN_POINT ( 'NONE',  ( 11.27814055543051630, 16.66797705449195988, -16.78371917145281955 ) ) ;
#21411 = ORIENTED_EDGE ( 'NONE', *, *, #24702, .F. ) ;
#21412 = CARTESIAN_POINT ( 'NONE',  ( 35.19403856461168090, -19.59168648217519504, -19.20845343762490032 ) ) ;
#21413 = CARTESIAN_POINT ( 'NONE',  ( 17.96884874826282186, 1.586046385177752871, -19.67104016136476119 ) ) ;
#21414 = EDGE_LOOP ( 'NONE', ( #21327, #19130 ) ) ;
#21415 = DIRECTION ( 'NONE',  ( -2.698458740408365879E-16, 1.000000000000000000, 0.000000000000000000 ) ) ;
#21416 = CARTESIAN_POINT ( 'NONE',  ( 9.068088202150136112, 16.38518988071972871, -17.09785080524718381 ) ) ;
#21417 = CARTESIAN_POINT ( 'NONE',  ( 25.72734949418555317, -2.696321649843969936, -17.76569039084671786 ) ) ;
#21418 = ORIENTED_EDGE ( 'NONE', *, *, #20768, .F. ) ;
#21419 = CARTESIAN_POINT ( 'NONE',  ( 131.1922820468854241, -10.00000000000000888, -30.91696583120935671 ) ) ;
#21420 = CARTESIAN_POINT ( 'NONE',  ( 19.23896461120675383, 4.098237937441782996, -14.15247350351863886 ) ) ;
#21421 = CARTESIAN_POINT ( 'NONE',  ( 18.03247465133560468, 8.846858265128714649, -18.47062581007826410 ) ) ;
#21422 = VERTEX_POINT ( 'NONE', #12419 ) ;
#21423 = LINE ( 'NONE', #12108, #14245 ) ;
#21424 = ADVANCED_FACE ( 'NONE', ( #28358 ), #1289, .T. ) ;
#21426 = ORIENTED_EDGE ( 'NONE', *, *, #8919, .F. ) ;
#21425 = EDGE_CURVE ( 'NONE', #21526, #10703, #24335, .T. ) ;
#21427 = LINE ( 'NONE', #9962, #17647 ) ;
#21428 = AXIS2_PLACEMENT_3D ( 'NONE', #14322, #16631, #9902 ) ;
#21429 = LINE ( 'NONE', #16846, #10394 ) ;
#21430 = AXIS2_PLACEMENT_3D ( 'NONE', #24252, #5780, #5629 ) ;
#21431 = LINE ( 'NONE', #3284, #11061 ) ;
#21432 = DIRECTION ( 'NONE',  ( -2.698458740408365879E-16, 1.000000000000000000, 0.000000000000000000 ) ) ;
#21433 = PLANE ( 'NONE',  #8023 ) ;
#21434 = CARTESIAN_POINT ( 'NONE',  ( 9.641890818133653340, 17.66641459721583374, -17.82828029666912073 ) ) ;
#21435 = CARTESIAN_POINT ( 'NONE',  ( 26.86129341093661793, -9.458291044957649163, -14.14057404834478682 ) ) ;
#21436 = CARTESIAN_POINT ( 'NONE',  ( 21.34960977245966873, -3.524359730468174412, -18.69795900347392248 ) ) ;
#21438 = VERTEX_POINT ( 'NONE', #19292 ) ;
#21437 = CARTESIAN_POINT ( 'NONE',  ( 34.86302720852563652, -20.10462780087231138, -21.19305451400748552 ) ) ;
#21439 = CARTESIAN_POINT ( 'NONE',  ( 137.2287565553230309, -4.999999999999980460, -29.49038105676659427 ) ) ;
#21440 = DIRECTION ( 'NONE',  ( -1.000000000000000000, -2.698458740408365879E-16, -0.000000000000000000 ) ) ;
#21441 = CARTESIAN_POINT ( 'NONE',  ( 154.7287565553229172, -10.00000000000000178, -16.50000000000000000 ) ) ;
#21442 = DIRECTION ( 'NONE',  ( -2.698458740408365879E-16, 1.000000000000000000, 0.000000000000000000 ) ) ;
#21443 = CARTESIAN_POINT ( 'NONE',  ( 18.69974902744413470, 8.051839821468062652, -15.50866580261103955 ) ) ;
#21445 = ORIENTED_EDGE ( 'NONE', *, *, #7320, .F. ) ;
#21444 = PRODUCT_DEFINITION_FORMATION_WITH_SPECIFIED_SOURCE ( 'ANY', '', #8864, .NOT_KNOWN. ) ;
#21446 = DIRECTION ( 'NONE',  ( -2.698458740408365879E-16, 1.000000000000000000, 0.000000000000000000 ) ) ;
#21447 = CARTESIAN_POINT ( 'NONE',  ( 10.33816386007038268, 18.38597432894226458, -17.88535571907410571 ) ) ;
#21448 = EDGE_CURVE ( 'NONE', #22950, #16768, #28111, .T. ) ;
#21449 = CIRCLE ( 'NONE', #27825, 6.999999999999999112 ) ;
#21450 = CARTESIAN_POINT ( 'NONE',  ( 133.7287565553229456, -84.33034373659253902, -33.50000000000000000 ) ) ;
#21451 = DIRECTION ( 'NONE',  ( -1.110223024625156540E-16, 0.000000000000000000, -1.000000000000000000 ) ) ;
#21452 = VECTOR ( 'NONE', #20516, 1000.000000000000000 ) ;
#21453 = CARTESIAN_POINT ( 'NONE',  ( 17.66155849027303049, 7.702290371990539342, -14.74052880078125760 ) ) ;
#21454 = CARTESIAN_POINT ( 'NONE',  ( 18.07402036735202699, 11.65617268414930940, -17.08825885362000108 ) ) ;
#21455 = VERTEX_POINT ( 'NONE', #1146 ) ;
#21456 = CARTESIAN_POINT ( 'NONE',  ( 33.29928106196997817, -12.14339677642331772, -19.64090527578606427 ) ) ;
#21457 = CARTESIAN_POINT ( 'NONE',  ( 21.70429774405079115, -3.429840324723197664, -17.59459576866303365 ) ) ;
#21458 = CARTESIAN_POINT ( 'NONE',  ( 18.78845540754137744, 2.550960650414936914, -18.75190108346638951 ) ) ;
#21459 = CARTESIAN_POINT ( 'NONE',  ( 25.78329585330208218, -10.67969159757694086, -14.14496057932236361 ) ) ;
#21460 = VECTOR ( 'NONE', #15155, 1000.000000000000000 ) ;
#21461 = AXIS2_PLACEMENT_3D ( 'NONE', #24950, #10588, #29426 ) ;
#21462 = ORIENTED_EDGE ( 'NONE', *, *, #26053, .T. ) ;
#21463 = ORIENTED_EDGE ( 'NONE', *, *, #10520, .T. ) ;
#21464 = DIRECTION ( 'NONE',  ( -1.000000000000000000, -2.891205793294689173E-16, 0.000000000000000000 ) ) ;
#21465 =( GEOMETRIC_REPRESENTATION_CONTEXT ( 3 ) GLOBAL_UNCERTAINTY_ASSIGNED_CONTEXT ( ( #29719 ) ) GLOBAL_UNIT_ASSIGNED_CONTEXT ( ( #12587, #857, #4046 ) ) REPRESENTATION_CONTEXT ( 'NONE', 'WORKASPACE' ) );
#21466 = DIRECTION ( 'NONE',  ( 1.000000000000000000, 0.000000000000000000, 0.000000000000000000 ) ) ;
#21467 = DIRECTION ( 'NONE',  ( -1.000000000000000000, -4.440892098500622217E-16, 0.000000000000000000 ) ) ;
#21468 = DIRECTION ( 'NONE',  ( 0.000000000000000000, 0.000000000000000000, 1.000000000000000000 ) ) ;
#21469 = CARTESIAN_POINT ( 'NONE',  ( 36.54859390953723874, -21.18451583373416014, -14.99999999999999822 ) ) ;
#21470 = CARTESIAN_POINT ( 'NONE',  ( 13.30044262271030142, 7.866402339252101861, -14.49220811360527605 ) ) ;
#21471 = LINE ( 'NONE', #11851, #15638 ) ;
#21472 = CARTESIAN_POINT ( 'NONE',  ( 146.1922820468854525, -1.999999999999976685, -19.40354224447947828 ) ) ;
#21473 = CARTESIAN_POINT ( 'NONE',  ( 13.06976498004312326, 8.549601185932660385, -15.95463209657921055 ) ) ;
#21474 = CARTESIAN_POINT ( 'NONE',  ( 171.1922820468853104, -4.999999999999971578, -13.59645775552055902 ) ) ;
#21475 = DIRECTION ( 'NONE',  ( 1.000000000000000000, 2.698458740408365879E-16, -1.110223024625156540E-16 ) ) ;
#21476 = VECTOR ( 'NONE', #7746, 1000.000000000000000 ) ;
#21477 = ADVANCED_FACE ( 'NONE', ( #551 ), #19782, .T. ) ;
#21478 = ADVANCED_FACE ( 'NONE', ( #3429 ), #19148, .T. ) ;
#21479 = ORIENTED_EDGE ( 'NONE', *, *, #6778, .T. ) ;
#21480 = CIRCLE ( 'NONE', #13682, 2.700000000000001066 ) ;
#21481 = DIRECTION ( 'NONE',  ( 0.3090169943749475623, 8.338696094058001131E-17, 0.9510565162951536422 ) ) ;
#21482 = EDGE_CURVE ( 'NONE', #29149, #28465, #29724, .T. ) ;
#21483 = CARTESIAN_POINT ( 'NONE',  ( 162.0152310637604671, -4.999999999999974243, -1.798730398669517640E-14 ) ) ;
#21484 = ORIENTED_EDGE ( 'NONE', *, *, #25576, .T. ) ;
#21485 = EDGE_CURVE ( 'NONE', #13389, #8350, #29260, .T. ) ;
#21486 = LINE ( 'NONE', #27118, #6711 ) ;
#21487 = EDGE_LOOP ( 'NONE', ( #29623, #16598, #12996, #28861 ) ) ;
#21488 = CARTESIAN_POINT ( 'NONE',  ( 11.22782251818125232, 9.073501160497098539, -17.23995927586370769 ) ) ;
#21489 = STYLED_ITEM ( 'NONE', ( #13199 ), #13457 ) ;
#21490 = CARTESIAN_POINT ( 'NONE',  ( 26.37829838608531219, -4.974601419860719353, -14.31557877768424092 ) ) ;
#21491 = CARTESIAN_POINT ( 'NONE',  ( 25.47985489653468605, -2.350970512090694520, -13.88367939857760014 ) ) ;
#21492 = DIRECTION ( 'NONE',  ( 0.5877852522924731371, 1.586114251531760728E-16, -0.8090169943749474513 ) ) ;
#21493 = DIRECTION ( 'NONE',  ( 0.9510565162951535312, 2.566386769018988816E-16, -0.3090169943749475623 ) ) ;
#21494 = CARTESIAN_POINT ( 'NONE',  ( 149.5152310637605808, -1.999999999999975797, -19.94844914048349693 ) ) ;
#21495 = CARTESIAN_POINT ( 'NONE',  ( 171.1922820468852819, -1.999999999999970912, -2.083034168790677043 ) ) ;
#21496 = CIRCLE ( 'NONE', #565, 4.000000000000003553 ) ;
#21497 = CARTESIAN_POINT ( 'NONE',  ( 136.1922820468854241, -10.00000000000000533, -28.06379628232387446 ) ) ;
#21498 = CONICAL_SURFACE ( 'NONE', #8361, 8.000000000000007105, 1.047197551196596077 ) ;
#21499 = PLANE ( 'NONE',  #29756 ) ;
#21500 = VECTOR ( 'NONE', #22195, 999.9999999999998863 ) ;
#21501 = LINE ( 'NONE', #9286, #1995 ) ;
#21502 = CARTESIAN_POINT ( 'NONE',  ( 147.0152310637605524, -4.999999999999977796, -1.632196944975745105E-14 ) ) ;
#21503 = CARTESIAN_POINT ( 'NONE',  ( 12.02761088988360783, 9.318053909225662679, -16.69151312802368636 ) ) ;
#21504 = FACE_OUTER_BOUND ( 'NONE', #30104, .T. ) ;
#21505 = FACE_OUTER_BOUND ( 'NONE', #516, .T. ) ;
#21506 = ORIENTED_EDGE ( 'NONE', *, *, #10827, .T. ) ;
#21507 = CARTESIAN_POINT ( 'NONE',  ( 8.944584683310379702, 16.95159276115599667, -19.66666666666843000 ) ) ;
#21508 = DIRECTION ( 'NONE',  ( -2.698458740408365879E-16, 1.000000000000000000, 0.000000000000000000 ) ) ;
#21509 = CARTESIAN_POINT ( 'NONE',  ( 23.76365953361780470, 2.837943588559999508, -16.54419024451982168 ) ) ;
#21510 = CARTESIAN_POINT ( 'NONE',  ( 12.81197645932666163, 9.633610080622574401, -16.14942406932820163 ) ) ;
#21511 = LINE ( 'NONE', #5184, #17044 ) ;
#21512 = ADVANCED_FACE ( 'NONE', ( #29103 ), #4026, .T. ) ;
#21513 = ORIENTED_EDGE ( 'NONE', *, *, #16619, .T. ) ;
#21514 = CARTESIAN_POINT ( 'NONE',  ( 11.39177520167864266, 9.641221755901229429, -15.89445043910815336 ) ) ;
#21515 = CARTESIAN_POINT ( 'NONE',  ( 0.000000000000000000, 0.000000000000000000, -2.424599999999998978 ) ) ;
#21516 = EDGE_CURVE ( 'NONE', #21824, #4884, #27155, .T. ) ;
#21517 = ADVANCED_FACE ( 'NONE', ( #19889 ), #5871, .F. ) ;
#21518 = CARTESIAN_POINT ( 'NONE',  ( 10.95411528722473626, 11.64838591225006859, -16.07543820933196699 ) ) ;
#21519 = DIRECTION ( 'NONE',  ( 0.5877852522924731371, 0.000000000000000000, 0.8090169943749474513 ) ) ;
#21520 = EDGE_CURVE ( 'NONE', #2375, #12138, #15612, .T. ) ;
#21521 = ORIENTED_EDGE ( 'NONE', *, *, #17996, .F. ) ;
#21522 = EDGE_LOOP ( 'NONE', ( #29345, #25383, #22018, #6782 ) ) ;
#21523 = DIRECTION ( 'NONE',  ( -0.000000000000000000, -0.000000000000000000, -1.000000000000000000 ) ) ;
#21524 = ORIENTED_EDGE ( 'NONE', *, *, #26191, .F. ) ;
#21525 = CARTESIAN_POINT ( 'NONE',  ( 13.11043623405165448, 8.565188957795726310, -15.92239833454181230 ) ) ;
#21526 = VERTEX_POINT ( 'NONE', #13321 ) ;
#21528 = VECTOR ( 'NONE', #15727, 1000.000000000000000 ) ;
#21527 = CARTESIAN_POINT ( 'NONE',  ( 36.54779501103016770, -22.18092680593016652, -18.48200341583098449 ) ) ;
#21529 = CARTESIAN_POINT ( 'NONE',  ( 28.67486520862709654, -7.888541471525570614, -13.83454100519475105 ) ) ;
#21530 = CARTESIAN_POINT ( 'NONE',  ( 26.32595758385100382, -12.12905223104374386, -14.21117607008287642 ) ) ;
#21531 = DIRECTION ( 'NONE',  ( 0.9510565162951536422, 2.566386769018988816E-16, 0.3090169943749472292 ) ) ;
#21532 = EDGE_LOOP ( 'NONE', ( #2262, #28471, #15580, #12613 ) ) ;
#21533 = CARTESIAN_POINT ( 'NONE',  ( 93.00224314937874226, -4.999999999999992006, 67.57008484791889202 ) ) ;
#21534 = ORIENTED_EDGE ( 'NONE', *, *, #25697, .F. ) ;
#21535 = CARTESIAN_POINT ( 'NONE',  ( 16.83868323617221208, 3.350830693655540315, -16.91447790370928672 ) ) ;
#21536 = CARTESIAN_POINT ( 'NONE',  ( 27.97039215263694345, -10.38370070276099710, -17.82092013489567606 ) ) ;
#21537 = SURFACE_SIDE_STYLE ('',( #3096 ) ) ;
#21538 = LINE ( 'NONE', #28596, #27931 ) ;
#21539 = VECTOR ( 'NONE', #24132, 1000.000000000000000 ) ;
#21540 = EDGE_LOOP ( 'NONE', ( #12581, #29930, #16839, #8419 ) ) ;
#21541 = LINE ( 'NONE', #17256, #18432 ) ;
#21542 = CARTESIAN_POINT ( 'NONE',  ( 20.00000000000001066, 60.00000000000000711, 24.99999999999998579 ) ) ;
#21543 = CARTESIAN_POINT ( 'NONE',  ( 172.2287565553229172, -9.999999999999996447, -20.83012701892220520 ) ) ;
#21544 = DIRECTION ( 'NONE',  ( -2.698458740408365879E-16, 1.000000000000000000, 0.000000000000000000 ) ) ;
#21545 = CARTESIAN_POINT ( 'NONE',  ( 12.25668235260104844, 9.587403967970216101, -15.31905460325341117 ) ) ;
#21546 = FACE_OUTER_BOUND ( 'NONE', #27533, .T. ) ;
#21547 = ORIENTED_EDGE ( 'NONE', *, *, #13011, .T. ) ;
#21548 = FACE_OUTER_BOUND ( 'NONE', #19111, .T. ) ;
#21549 = ORIENTED_EDGE ( 'NONE', *, *, #303, .T. ) ;
#21550 = CARTESIAN_POINT ( 'NONE',  ( 11.47395765415086188, 9.264374527449886543, -15.86046114005151075 ) ) ;
#21551 = ORIENTED_EDGE ( 'NONE', *, *, #7569, .T. ) ;
#21552 = ADVANCED_FACE ( 'NONE', ( #22645 ), #13175, .T. ) ;
#21553 = AXIS2_PLACEMENT_3D ( 'NONE', #8431, #3715, #3868 ) ;
#21554 = ADVANCED_FACE ( 'NONE', ( #20049 ), #8142, .T. ) ;
#21555 = CARTESIAN_POINT ( 'NONE',  ( 19.10622122644073428, 3.678778577015775042, -19.67015202264490625 ) ) ;
#21556 = DIRECTION ( 'NONE',  ( 0.3331260486002958765, -0.05059491534325381845, -0.9415238660200613285 ) ) ;
#21557 = CARTESIAN_POINT ( 'NONE',  ( 147.2287565553230309, -10.00000000000000178, -20.83012701892220520 ) ) ;
#21558 = EDGE_CURVE ( 'NONE', #22270, #26851, #15459, .T. ) ;
#21559 = PLANE ( 'NONE',  #26346 ) ;
#21560 = DIRECTION ( 'NONE',  ( -0.000000000000000000, -0.000000000000000000, 1.000000000000000000 ) ) ;
#21561 = EDGE_CURVE ( 'NONE', #15878, #23534, #1601, .T. ) ;
#21562 = CARTESIAN_POINT ( 'NONE',  ( 11.27239417409149880, 16.69433069180593776, -16.78622300611779750 ) ) ;
#21563 = ORIENTED_EDGE ( 'NONE', *, *, #11995, .F. ) ;
#21564 = CARTESIAN_POINT ( 'NONE',  ( 33.20927704557755789, -11.78629111679139996, -17.96241082601573424 ) ) ;
#21565 = CARTESIAN_POINT ( 'NONE',  ( 14.17177033308128031, 6.273687421093853800, -17.36430109743762173 ) ) ;
#21566 = DIRECTION ( 'NONE',  ( 0.9510565162951536422, 0.000000000000000000, -0.3090169943749475623 ) ) ;
#21567 = VECTOR ( 'NONE', #17065, 1000.000000000000000 ) ;
#21568 = CARTESIAN_POINT ( 'NONE',  ( 23.14387462191455214, -5.292040767005758539, -18.71731562455695297 ) ) ;
#21569 = EDGE_LOOP ( 'NONE', ( #5380, #30110, #21260, #20627 ) ) ;
#21570 = DIRECTION ( 'NONE',  ( 0.9510565162951535312, 2.566386769018988816E-16, -0.3090169943749475623 ) ) ;
#21571 =( NAMED_UNIT ( * ) SI_UNIT ( $, .STERADIAN. ) SOLID_ANGLE_UNIT ( ) );
#21572 = CARTESIAN_POINT ( 'NONE',  ( 19.50876870223950377, -1.661710298099399630, -15.95382585723518432 ) ) ;
#21573 = CARTESIAN_POINT ( 'NONE',  ( 15.15242361522499692, 5.855521407460130057, -16.92275779674541170 ) ) ;
#21574 = ORIENTED_EDGE ( 'NONE', *, *, #14358, .T. ) ;
#21575 = LINE ( 'NONE', #18568, #19615 ) ;
#21576 = ORIENTED_EDGE ( 'NONE', *, *, #10309, .T. ) ;
#21577 = ORIENTED_EDGE ( 'NONE', *, *, #5468, .T. ) ;
#21578 = DIRECTION ( 'NONE',  ( -0.9510565162951536422, -2.566386769018988816E-16, -0.3090169943749472292 ) ) ;
#21579 = CIRCLE ( 'NONE', #23523, 2.041999999999999815 ) ;
#21580 = DIRECTION ( 'NONE',  ( -0.9510565162951536422, -2.566386769018988816E-16, -0.3090169943749472292 ) ) ;
#21581 = EDGE_CURVE ( 'NONE', #11833, #14866, #24789, .T. ) ;
#21582 = CARTESIAN_POINT ( 'NONE',  ( 107.7837191567167565, -4.999999999999987566, 78.30945579394082756 ) ) ;
#21583 = CARTESIAN_POINT ( 'NONE',  ( 0.000000000000000000, -1.178949249685215417, 2.042000000000002036 ) ) ;
#21584 = LINE ( 'NONE', #543, #12401 ) ;
#21585 = AXIS2_PLACEMENT_3D ( 'NONE', #19957, #29329, #15821 ) ;
#21586 = CARTESIAN_POINT ( 'NONE',  ( 11.47181023233108021, 9.274170903235749108, -15.86135313853478657 ) ) ;
#21587 = CARTESIAN_POINT ( 'NONE',  ( 27.11308663627701776, -11.54974243744149653, -14.54931088138702933 ) ) ;
#21588 = CARTESIAN_POINT ( 'NONE',  ( 21.19231167106929803, 0.1271100694386541607, -19.24388053421374778 ) ) ;
#21590 = VERTEX_POINT ( 'NONE', #24632 ) ;
#21589 = CARTESIAN_POINT ( 'NONE',  ( 32.77977724007769211, -11.13765286058784554, -18.71157503069099448 ) ) ;
#21591 = CARTESIAN_POINT ( 'NONE',  ( 130.7287565553228887, -4.999999999999982236, -10.89389676854976585 ) ) ;
#21592 = CARTESIAN_POINT ( 'NONE',  ( -1.660531772554310725, 3.660093687634845772, -2.450000000000005507 ) ) ;
#21593 = CARTESIAN_POINT ( 'NONE',  ( -0.6543461111163949573, -4.241015250120828028, -0.1391502195351573268 ) ) ;
#21594 = ADVANCED_FACE ( 'NONE', ( #1744 ), #24485, .T. ) ;
#21595 = DIRECTION ( 'NONE',  ( -2.698458740408365879E-16, 1.000000000000000000, 0.000000000000000000 ) ) ;
#21596 = CARTESIAN_POINT ( 'NONE',  ( 4.000000000000003553, 2.309401076758525573, -2.092734410091829034 ) ) ;
#21597 = CARTESIAN_POINT ( 'NONE',  ( 21.66440995182641416, 5.535554982823286174, -17.57621636221614025 ) ) ;
#21598 = ORIENTED_EDGE ( 'NONE', *, *, #467, .T. ) ;
#21599 = LINE ( 'NONE', #4966, #8562 ) ;
#21600 = ADVANCED_FACE ( 'NONE', ( #17886 ), #12870, .F. ) ;
#21601 = CARTESIAN_POINT ( 'NONE',  ( 10.71436926824426550, 16.66064837202128501, -15.95707641581892133 ) ) ;
#21602 = DIRECTION ( 'NONE',  ( 1.110223024625156540E-16, 2.995891024602366092E-32, 1.000000000000000000 ) ) ;
#21603 = CARTESIAN_POINT ( 'NONE',  ( 171.1922820468853388, -9.999999999999996447, -22.25671179336496053 ) ) ;
#21604 = AXIS2_PLACEMENT_3D ( 'NONE', #7909, #899, #17068 ) ;
#21605 = CARTESIAN_POINT ( 'NONE',  ( 24.66978787416869068, -0.3063955544261361963, -14.42797892638687784 ) ) ;
#21606 = CARTESIAN_POINT ( 'NONE',  ( 14.42366234001531922, 7.375548675892134476, -20.85295579936483179 ) ) ;
#21607 = EDGE_LOOP ( 'NONE', ( #11945, #15171, #30143, #3866, #4434 ) ) ;
#21608 = CARTESIAN_POINT ( 'NONE',  ( 33.33926371295168423, -12.28475995124076903, -19.67523791759492013 ) ) ;
#21609 = CARTESIAN_POINT ( 'NONE',  ( 21.79248024726475563, -3.676524810334697246, -15.28166220873658077 ) ) ;
#21610 = CARTESIAN_POINT ( 'NONE',  ( 20.37262416712335167, 4.106476634890254829, -18.27772908839511246 ) ) ;
#21611 = AXIS2_PLACEMENT_3D ( 'NONE', #20217, #22371, #26983 ) ;
#21612 = DIRECTION ( 'NONE',  ( -2.698458740408365879E-16, 1.000000000000000000, 0.000000000000000000 ) ) ;
#21613 = ADVANCED_FACE ( 'NONE', ( #3729 ), #5366, .T. ) ;
#21615 = ORIENTED_EDGE ( 'NONE', *, *, #23847, .T. ) ;
#21614 = CARTESIAN_POINT ( 'NONE',  ( 0.000000000000000000, 0.000000000000000000, -15.00000000000000000 ) ) ;
#21616 = CARTESIAN_POINT ( 'NONE',  ( 159.5152310637605240, -1.999999999999972689, -30.37205893520531319 ) ) ;
#21617 = DIRECTION ( 'NONE',  ( 0.9510565162951536422, 0.000000000000000000, -0.3090169943749475623 ) ) ;
#21618 = CARTESIAN_POINT ( 'NONE',  ( 34.21937970685856101, -11.80343312934236089, -19.83772509046166732 ) ) ;
#21619 = CARTESIAN_POINT ( 'NONE',  ( 9.641350810849047548, 17.66889113945805789, -17.92454625180715766 ) ) ;
#21620 = AXIS2_PLACEMENT_3D ( 'NONE', #8363, #29941, #10804 ) ;
#21621 = FACE_OUTER_BOUND ( 'NONE', #21894, .T. ) ;
#21622 = LINE ( 'NONE', #17048, #15348 ) ;
#21623 = CARTESIAN_POINT ( 'NONE',  ( 13.11965390131543430, 8.569119222385459977, -15.91506261175275760 ) ) ;
#21624 = CARTESIAN_POINT ( 'NONE',  ( 149.5152310637605240, -1.999999999999976685, -2.627941064794695691 ) ) ;
#21625 = LINE ( 'NONE', #10168, #19757 ) ;
#21626 = VERTEX_POINT ( 'NONE', #17254 ) ;
#21627 = LINE ( 'NONE', #24234, #26125 ) ;
#21628 = DIRECTION ( 'NONE',  ( -0.8090169943749474513, -2.183098979609982436E-16, -0.5877852522924731371 ) ) ;
#21629 = EDGE_LOOP ( 'NONE', ( #23977, #4725, #21814, #7130, #626 ) ) ;
#21630 = ORIENTED_EDGE ( 'NONE', *, *, #2218, .F. ) ;
#21631 = CARTESIAN_POINT ( 'NONE',  ( 12.16405474897817207, 7.700086518927777846, -16.63006945039463247 ) ) ;
#21632 = CARTESIAN_POINT ( 'NONE',  ( 25.82086518536678454, -3.233603117969178875, -16.21460360555060021 ) ) ;
#21633 = CARTESIAN_POINT ( 'NONE',  ( 21.30888034401541731, -0.8953576338359930942, -14.03585182699830369 ) ) ;
#21634 = DIRECTION ( 'NONE',  ( 0.3090169943749475623, 8.338696094058001131E-17, 0.9510565162951536422 ) ) ;
#21635 = CARTESIAN_POINT ( 'NONE',  ( 1.214306433183764966E-14, 4.618802153517016507, -2.092734410091829034 ) ) ;
#21636 = DIRECTION ( 'NONE',  ( -2.698458740408365879E-16, 1.000000000000000000, 0.000000000000000000 ) ) ;
#21637 = AXIS2_PLACEMENT_3D ( 'NONE', #11809, #29907, #25268 ) ;
#21638 = CARTESIAN_POINT ( 'NONE',  ( 132.2287565553230024, -1.999999999999981348, -12.16987298107780013 ) ) ;
#21639 = EDGE_CURVE ( 'NONE', #29239, #1679, #12481, .T. ) ;
#21640 = DIRECTION ( 'NONE',  ( -0.000000000000000000, -0.000000000000000000, -1.000000000000000000 ) ) ;
#21641 = CARTESIAN_POINT ( 'NONE',  ( 0.000000000000000000, 0.000000000000000000, -2.450000000000000178 ) ) ;
#21642 = EDGE_CURVE ( 'NONE', #7383, #22052, #24136, .T. ) ;
#21643 = CARTESIAN_POINT ( 'NONE',  ( 129.5152310637605808, -1.999999999999982236, -2.627941064794695691 ) ) ;
#21644 = DIRECTION ( 'NONE',  ( -2.698458740408365879E-16, 1.000000000000000000, 0.000000000000000000 ) ) ;
#21645 = CARTESIAN_POINT ( 'NONE',  ( 10.48820292689142519, 16.37797505638186735, -17.32811247259324716 ) ) ;
#21646 = DIRECTION ( 'NONE',  ( 1.000000000000000000, 0.000000000000000000, -0.000000000000000000 ) ) ;
#21647 = CARTESIAN_POINT ( 'NONE',  ( 33.69611315462438483, -12.86230108826256924, -18.75566652118837752 ) ) ;
#21648 = ORIENTED_EDGE ( 'NONE', *, *, #9838, .F. ) ;
#21649 = CARTESIAN_POINT ( 'NONE',  ( 13.38606102883407445, 7.628803627606831839, -15.70273264218319120 ) ) ;
#21650 = LINE ( 'NONE', #28422, #9012 ) ;
#21651 = CARTESIAN_POINT ( 'NONE',  ( 25.45462155318426767, -0.2439708902934435431, -15.99927030562601438 ) ) ;
#21652 = CARTESIAN_POINT ( 'NONE',  ( 12.79171442625009547, 9.726534347120292523, -16.15780313276466273 ) ) ;
#21653 = DIRECTION ( 'NONE',  ( -0.5877852522924731371, -1.586114251531760235E-16, 0.8090169943749474513 ) ) ;
#21654 = EDGE_LOOP ( 'NONE', ( #3482, #27817, #17745, #29709 ) ) ;
#21655 = ORIENTED_EDGE ( 'NONE', *, *, #14443, .F. ) ;
#21656 = CARTESIAN_POINT ( 'NONE',  ( 9.919231947839115549, 16.39449282361540483, -16.50339887433786501 ) ) ;
#21657 = DIRECTION ( 'NONE',  ( 0.000000000000000000, 0.000000000000000000, -1.000000000000000000 ) ) ;
#21658 = CONICAL_SURFACE ( 'NONE', #22635, 5.000000000000006217, 0.9599310885968819207 ) ;
#21659 = CARTESIAN_POINT ( 'NONE',  ( 9.919231947839115549, 16.39449282361540483, -16.50339887433786501 ) ) ;
#21660 = FACE_OUTER_BOUND ( 'NONE', #27376, .T. ) ;
#21661 = ORIENTED_EDGE ( 'NONE', *, *, #10034, .T. ) ;
#21662 = LINE ( 'NONE', #625, #10081 ) ;
#21663 = ORIENTED_EDGE ( 'NONE', *, *, #8168, .T. ) ;
#21664 = CARTESIAN_POINT ( 'NONE',  ( 12.26413032053702779, 8.815164712426300397, -16.54932944099246228 ) ) ;
#21665 = ORIENTED_EDGE ( 'NONE', *, *, #27011, .T. ) ;
#21666 = CARTESIAN_POINT ( 'NONE',  ( 35.12112610261377910, -16.77165912796762726, -21.20079607051596327 ) ) ;
#21667 = CARTESIAN_POINT ( 'NONE',  ( 29.30346499805017757, -7.722527705200430859, -14.56292402596598556 ) ) ;
#21668 = CARTESIAN_POINT ( 'NONE',  ( 28.75197783424699693, -9.407057218516385433, -18.70835418409691542 ) ) ;
#21669 = VERTEX_POINT ( 'NONE', #14653 ) ;
#21670 = CARTESIAN_POINT ( 'NONE',  ( 132.0152310637605524, -1.999999999999981348, -0.06116980274991495881 ) ) ;
#21671 = ORIENTED_EDGE ( 'NONE', *, *, #11615, .F. ) ;
#21672 = CARTESIAN_POINT ( 'NONE',  ( 34.28781561389841670, -12.04879923890588422, -19.89451123369701691 ) ) ;
#21673 = ITEM_DEFINED_TRANSFORMATION ( 'NONE', 'NONE', #5369,  #13190 ) ;
#21674 = VERTEX_POINT ( 'NONE', #12223 ) ;
#21675 = CARTESIAN_POINT ( 'NONE',  ( 20.54317392443767076, 4.330699614500605144, -17.92201748610454715 ) ) ;
#21676 = CARTESIAN_POINT ( 'NONE',  ( 14.33367420948735393, 6.252843122977492563, -16.41390433006782956 ) ) ;
#21677 = EDGE_LOOP ( 'NONE', ( #933, #27432, #25348, #19675 ) ) ;
#21678 = DIRECTION ( 'NONE',  ( -2.698458740408365879E-16, 1.000000000000000000, 0.000000000000000000 ) ) ;
#21679 = FACE_BOUND ( 'NONE', #2588, .T. ) ;
#21680 = EDGE_CURVE ( 'NONE', #7265, #436, #2941, .T. ) ;
#21681 = ADVANCED_FACE ( 'NONE', ( #19687 ), #24435, .T. ) ;
#21682 = AXIS2_PLACEMENT_3D ( 'NONE', #13020, #15605, #6311 ) ;
#21683 = EDGE_CURVE ( 'NONE', #19068, #12130, #26435, .T. ) ;
#21684 = ORIENTED_EDGE ( 'NONE', *, *, #29502, .T. ) ;
#21685 = DIRECTION ( 'NONE',  ( -0.8090169943749474513, -2.183098979609982436E-16, -0.5877852522924731371 ) ) ;
#21686 = DIRECTION ( 'NONE',  ( -0.8090169943749474513, -2.183098979609982436E-16, 0.5877852522924731371 ) ) ;
#21687 = LINE ( 'NONE', #24005, #29775 ) ;
#21688 = CARTESIAN_POINT ( 'NONE',  ( 176.1922820468853104, -9.999999999999994671, -22.25671179336496053 ) ) ;
#21689 = CARTESIAN_POINT ( 'NONE',  ( 12.26747700539757346, 9.511763647452495363, -15.31658389161178668 ) ) ;
#21690 = PLANE ( 'NONE',  #27997 ) ;
#21691 = VERTEX_POINT ( 'NONE', #10074 ) ;
#21692 = CARTESIAN_POINT ( 'NONE',  ( 11.07703429628124958, -5.000000000000015099, 34.09160609439044975 ) ) ;
#21693 = VERTEX_POINT ( 'NONE', #8087 ) ;
#21694 = CARTESIAN_POINT ( 'NONE',  ( 11.47310491742633687, 9.268236560789974376, -15.86081749295074594 ) ) ;
#21695 = ORIENTED_EDGE ( 'NONE', *, *, #4499, .T. ) ;
#21696 = CARTESIAN_POINT ( 'NONE',  ( 19.61234978942155038, 5.539603999143367652, -15.30853080630118512 ) ) ;
#21697 = LINE ( 'NONE', #23702, #1002 ) ;
#21698 =( NAMED_UNIT ( * ) SI_UNIT ( $, .STERADIAN. ) SOLID_ANGLE_UNIT ( ) );
#21699 = CARTESIAN_POINT ( 'NONE',  ( 169.7287565553229456, -1.999999999999970024, -25.16025403784440329 ) ) ;
#21700 = EDGE_LOOP ( 'NONE', ( #25649, #21915, #4028, #1912, #19981, #8090 ) ) ;
#21701 = CARTESIAN_POINT ( 'NONE',  ( 74.18800000000001660, 0.000000000000000000, 0.000000000000000000 ) ) ;
#21702 = CARTESIAN_POINT ( 'NONE',  ( 12.83231907764629476, 9.540323555994485005, -16.14101112307237074 ) ) ;
#21703 = ORIENTED_EDGE ( 'NONE', *, *, #11376, .T. ) ;
#21704 = CARTESIAN_POINT ( 'NONE',  ( 35.46586886002400263, -20.81287600694606610, -19.09165458252410374 ) ) ;
#21705 = CARTESIAN_POINT ( 'NONE',  ( 19.05868480923028940, 8.129737193291200370, -16.02886444249750042 ) ) ;
#21706 = VECTOR ( 'NONE', #20148, 1000.000000000000000 ) ;
#21707 = CARTESIAN_POINT ( 'NONE',  ( -5.000000000000005329, -1.608122649676636157E-15, 0.000000000000000000 ) ) ;
#21708 = CARTESIAN_POINT ( 'NONE',  ( 18.35279563442798079, 9.979516425631709708, -19.26739628155305439 ) ) ;
#21709 = EDGE_LOOP ( 'NONE', ( #22809, #10635, #16475, #22864 ) ) ;
#21710 = DIRECTION ( 'NONE',  ( -0.5877852522924731371, 0.000000000000000000, 0.8090169943749474513 ) ) ;
#21711 = EDGE_CURVE ( 'NONE', #21764, #17928, #26283, .T. ) ;
#21712 = CARTESIAN_POINT ( 'NONE',  ( 24.68325608809179528, -0.07379305852225118145, -17.41420097001153167 ) ) ;
#21713 = CARTESIAN_POINT ( 'NONE',  ( 18.15277384750198308, 2.816914934748806054, -19.48283598520044180 ) ) ;
#21714 = LINE ( 'NONE', #26318, #6953 ) ;
#21715 = ORIENTED_EDGE ( 'NONE', *, *, #4408, .T. ) ;
#21716 = VECTOR ( 'NONE', #11820, 1000.000000000000000 ) ;
#21717 = PLANE ( 'NONE',  #2078 ) ;
#21718 = EDGE_CURVE ( 'NONE', #12491, #24756, #10527, .T. ) ;
#21719 = EDGE_LOOP ( 'NONE', ( #13672, #15508, #3511, #12391 ) ) ;
#21720 = AXIS2_PLACEMENT_3D ( 'NONE', #21324, #10018, #587 ) ;
#21721 = EDGE_CURVE ( 'NONE', #12612, #1753, #12365, .T. ) ;
#21722 = EDGE_CURVE ( 'NONE', #117, #17394, #29050, .T. ) ;
#21723 = CARTESIAN_POINT ( 'NONE',  ( 86.03433166160688472, -4.999999999999993783, 62.50760082067552048 ) ) ;
#21724 = EDGE_CURVE ( 'NONE', #13408, #13174, #7801, .T. ) ;
#21725 = CARTESIAN_POINT ( 'NONE',  ( 132.0152310637605524, -10.00000000000000711, -8.721423840594310306 ) ) ;
#21726 = CARTESIAN_POINT ( 'NONE',  ( 159.5152310637604387, -10.00000000000000000, -4.391296821672111328 ) ) ;
#21727 = VECTOR ( 'NONE', #4812, 1000.000000000000000 ) ;
#21728 = LINE ( 'NONE', #10122, #25582 ) ;
#21729 = VECTOR ( 'NONE', #14474, 1000.000000000000000 ) ;
#21730 = CARTESIAN_POINT ( 'NONE',  ( 11.47338783222600789, 9.266948822715743717, -15.86069975447064806 ) ) ;
#21731 = CARTESIAN_POINT ( 'NONE',  ( 26.77273401934504093, -11.50074486517209138, -16.59227217106661101 ) ) ;
#21732 = CARTESIAN_POINT ( 'NONE',  ( 26.55721583451634160, -2.971036115494387175, -18.36415422809029607 ) ) ;
#21734 = ORIENTED_EDGE ( 'NONE', *, *, #3283, .F. ) ;
#21733 = CARTESIAN_POINT ( 'NONE',  ( 33.40713826534622655, -12.56408340279653757, -19.71064172033093698 ) ) ;
#21735 = DIRECTION ( 'NONE',  ( 0.9510565162951535312, 2.566386769018988816E-16, -0.3090169943749475623 ) ) ;
#21736 = AXIS2_PLACEMENT_3D ( 'NONE', #21725, #14544, #3136 ) ;
#21737 = MANIFOLD_SOLID_BREP ( 'Extrude-Thin1', #28269 ) ;
#21738 = FACE_BOUND ( 'NONE', #18307, .T. ) ;
#21739 = CARTESIAN_POINT ( 'NONE',  ( 5.200000000000002842, 0.000000000000000000, 0.000000000000000000 ) ) ;
#21740 = DIRECTION ( 'NONE',  ( -0.5877852522924731371, -1.586114251531760235E-16, 0.8090169943749474513 ) ) ;
#21741 = DIRECTION ( 'NONE',  ( 1.000000000000000000, 2.891205793294675861E-16, 0.000000000000000000 ) ) ;
#21742 = DIRECTION ( 'NONE',  ( -2.698458740408365879E-16, 1.000000000000000000, 0.000000000000000000 ) ) ;
#21743 = CARTESIAN_POINT ( 'NONE',  ( 18.98200677837107264, -2.562081333921657933, -16.63161468174866187 ) ) ;
#21744 = ORIENTED_EDGE ( 'NONE', *, *, #28241, .F. ) ;
#21745 = CARTESIAN_POINT ( 'NONE',  ( 171.1922820468852819, -9.999999999999996447, -2.083034168790677043 ) ) ;
#21746 = CARTESIAN_POINT ( 'NONE',  ( 12.11484812106508713, 10.23787383345373136, -15.37770804730690166 ) ) ;
#21747 = PLANE ( 'NONE',  #12964 ) ;
#21748 = DIRECTION ( 'NONE',  ( -2.698458740408365879E-16, 1.000000000000000000, 0.000000000000000000 ) ) ;
#21749 = CIRCLE ( 'NONE', #16383, 5.999999999999977796 ) ;
#21750 = CARTESIAN_POINT ( 'NONE',  ( 21.10023079691774228, -0.4353598523292347422, -20.14113737667230097 ) ) ;
#21751 = CARTESIAN_POINT ( 'NONE',  ( 19.35412429307980986, 8.340480409601783052, -14.20924892776020343 ) ) ;
#21752 = EDGE_LOOP ( 'NONE', ( #2730, #22849, #13562, #9042 ) ) ;
#21753 = CARTESIAN_POINT ( 'NONE',  ( 34.82539348385352440, -18.93555941106099993, -20.13934242161363741 ) ) ;
#21754 = EDGE_CURVE ( 'NONE', #1397, #12383, #21989, .T. ) ;
#21755 = ORIENTED_EDGE ( 'NONE', *, *, #22840, .T. ) ;
#21756 =( NAMED_UNIT ( * ) SI_UNIT ( $, .STERADIAN. ) SOLID_ANGLE_UNIT ( ) );
#21757 = CARTESIAN_POINT ( 'NONE',  ( 28.21504805113574221, -4.147720155524260655, -15.34900075604336500 ) ) ;
#21758 = AXIS2_PLACEMENT_3D ( 'NONE', #7821, #17129, #15121 ) ;
#21759 = CARTESIAN_POINT ( 'NONE',  ( 18.31666763169264911, 2.112308299563359970, -18.35152529819803746 ) ) ;
#21760 = AXIS2_PLACEMENT_3D ( 'NONE', #27104, #26799, #17601 ) ;
#21761 = EDGE_LOOP ( 'NONE', ( #4442, #4972, #15248, #10085, #15122 ) ) ;
#21762 = EDGE_LOOP ( 'NONE', ( #14748, #1816, #211, #16235 ) ) ;
#21763 = EDGE_CURVE ( 'NONE', #1338, #20421, #24183, .T. ) ;
#21764 = VERTEX_POINT ( 'NONE', #27368 ) ;
#21765 = EDGE_CURVE ( 'NONE', #12978, #25256, #19994, .T. ) ;
#21766 = CARTESIAN_POINT ( 'NONE',  ( 94.33602617680786295, -4.999999999999992006, -68.53913494047789357 ) ) ;
#21767 = EDGE_CURVE ( 'NONE', #7222, #17091, #22747, .T. ) ;
#21768 = SURFACE_STYLE_FILL_AREA ( #14579 ) ;
#21769 = CARTESIAN_POINT ( 'NONE',  ( 142.0152310637605808, -1.999999999999978018, -17.38167787843871182 ) ) ;
#21770 = CARTESIAN_POINT ( 'NONE',  ( 0.000000000000000000, 0.000000000000000000, -4.974599999999998801 ) ) ;
#21771 = AXIS2_PLACEMENT_3D ( 'NONE', #14684, #9660, #7529 ) ;
#21772 = CARTESIAN_POINT ( 'NONE',  ( 120.0000000000000000, -19.99999999999999645, -186.4312945166758482 ) ) ;
#21773 = CARTESIAN_POINT ( 'NONE',  ( 36.54859390953724585, -22.18451583373416014, -17.64281456791166036 ) ) ;
#21774 = VECTOR ( 'NONE', #2623, 1000.000000000000000 ) ;
#21775 = CARTESIAN_POINT ( 'NONE',  ( 9.655099948573186097, 17.60583584124798051, -17.48406748397995614 ) ) ;
#21776 = VECTOR ( 'NONE', #4863, 1000.000000000000000 ) ;
#21777 = DIRECTION ( 'NONE',  ( -0.8090169943749474513, -2.183098979609982436E-16, 0.5877852522924731371 ) ) ;
#21778 = CARTESIAN_POINT ( 'NONE',  ( 154.5152310637604955, -4.999999999999975131, -2.627941064794695691 ) ) ;
#21779 = CARTESIAN_POINT ( 'NONE',  ( 13.09695832212169364, 8.559710067821024282, -15.93310406974445392 ) ) ;
#21780 = LINE ( 'NONE', #19936, #15088 ) ;
#21781 = CARTESIAN_POINT ( 'NONE',  ( 169.5152310637604103, -4.999999999999971578, -1.881997125516403749E-14 ) ) ;
#21782 = ORIENTED_EDGE ( 'NONE', *, *, #21448, .F. ) ;
#21783 = PLANE ( 'NONE',  #25621 ) ;
#21784 = CARTESIAN_POINT ( 'NONE',  ( 152.0152310637606092, -4.999999999999976019, -32.93883019725009120 ) ) ;
#21785 = CARTESIAN_POINT ( 'NONE',  ( 131.1922820468854241, -10.00000000000000888, -28.06379628232387446 ) ) ;
#21786 = ORIENTED_EDGE ( 'NONE', *, *, #16125, .F. ) ;
#21787 = ORIENTED_EDGE ( 'NONE', *, *, #22835, .T. ) ;
#21788 = VERTEX_POINT ( 'NONE', #29521 ) ;
#21789 = CARTESIAN_POINT ( 'NONE',  ( 11.68823183152383471, 8.106166304734948369, -16.96230016324342671 ) ) ;
#21790 = EDGE_CURVE ( 'NONE', #19672, #14318, #5666, .T. ) ;
#21791 = EDGE_CURVE ( 'NONE', #436, #6429, #1394, .T. ) ;
#21792 = CARTESIAN_POINT ( 'NONE',  ( 30.07451494818246474, -7.670792865742884992, -18.22619146169064663 ) ) ;
#21793 = CARTESIAN_POINT ( 'NONE',  ( 24.77705064808911217, -2.604154092221317551, -13.46095375842554098 ) ) ;
#21794 = VECTOR ( 'NONE', #26152, 1000.000000000000000 ) ;
#21795 = CARTESIAN_POINT ( 'NONE',  ( 166.1922820468853672, -4.999999999999973355, -22.25671179336496053 ) ) ;
#21796 = DIRECTION ( 'NONE',  ( 0.3090169943749472292, 8.338696094057992503E-17, -0.9510565162951536422 ) ) ;
#21797 = DIRECTION ( 'NONE',  ( -0.5877852522924731371, -1.586114251531760728E-16, -0.8090169943749474513 ) ) ;
#21798 = AXIS2_PLACEMENT_3D ( 'NONE', #3742, #27722, #20507 ) ;
#21799 = ORIENTED_EDGE ( 'NONE', *, *, #7021, .F. ) ;
#21800 = CARTESIAN_POINT ( 'NONE',  ( 147.0152310637606092, -10.00000000000000178, -24.27857615940569502 ) ) ;
#21801 = ADVANCED_FACE ( 'NONE', ( #13277 ), #22596, .T. ) ;
#21802 = LINE ( 'NONE', #12324, #5504 ) ;
#21803 = CARTESIAN_POINT ( 'NONE',  ( 159.7287565553228887, -1.999999999999974021, 0.8205080756887930260 ) ) ;
#21804 = ORIENTED_EDGE ( 'NONE', *, *, #6086, .F. ) ;
#21805 = DIRECTION ( 'NONE',  ( -0.9510565162951536422, 0.000000000000000000, -0.3090169943749472292 ) ) ;
#21806 = DIRECTION ( 'NONE',  ( 1.110223024625156540E-16, 2.995891024602366092E-32, 1.000000000000000000 ) ) ;
#21807 = CARTESIAN_POINT ( 'NONE',  ( 10.47249985125707106, 16.44999136291752251, -17.33460624675630513 ) ) ;
#21808 = CARTESIAN_POINT ( 'NONE',  ( 33.09970432537804896, -11.76965169494800989, -17.65272085910585886 ) ) ;
#21809 = ORIENTED_EDGE ( 'NONE', *, *, #3857, .T. ) ;
#21810 = CARTESIAN_POINT ( 'NONE',  ( 9.242255153701981030, 15.58643803978083753, -17.00107889682120899 ) ) ;
#21811 = CARTESIAN_POINT ( 'NONE',  ( 23.63863231746517712, -2.790269051896475450, -19.68844555248840678 ) ) ;
#21812 = CARTESIAN_POINT ( 'NONE',  ( 12.85347977544317111, 9.515020184875311315, -16.12678873937763413 ) ) ;
#21813 = FACE_BOUND ( 'NONE', #26080, .T. ) ;
#21814 = ORIENTED_EDGE ( 'NONE', *, *, #12933, .T. ) ;
#21815 = AXIS2_PLACEMENT_3D ( 'NONE', #23676, #4900, #14197 ) ;
#21816 = DIRECTION ( 'NONE',  ( -1.000000000000000000, -4.440892098500622217E-16, 0.000000000000000000 ) ) ;
#21817 = CARTESIAN_POINT ( 'NONE',  ( 11.46775782571576130, 9.292755756535285627, -15.86302895122203616 ) ) ;
#21818 = DIRECTION ( 'NONE',  ( -0.5877852522924731371, -1.586114251531760728E-16, -0.8090169943749474513 ) ) ;
#21819 = ORIENTED_EDGE ( 'NONE', *, *, #3645, .F. ) ;
#21820 = CARTESIAN_POINT ( 'NONE',  ( 176.1922820468853388, -1.999999999999968914, -30.91696583120936026 ) ) ;
#21821 = ORIENTED_EDGE ( 'NONE', *, *, #25339, .T. ) ;
#21822 = CARTESIAN_POINT ( 'NONE',  ( 12.02908293258818517, 9.311337566433326884, -16.69090174519279657 ) ) ;
#21823 = ADVANCED_FACE ( 'NONE', ( #8538 ), #22903, .T. ) ;
#21824 = VERTEX_POINT ( 'NONE', #29832 ) ;
#21825 = CARTESIAN_POINT ( 'NONE',  ( 35.54910479118309041, -18.69434066908399217, -21.33016376092627553 ) ) ;
#21826 = CARTESIAN_POINT ( 'NONE',  ( 28.47856004806874353, -11.16640101040803401, -12.66155532224275149 ) ) ;
#21827 = CARTESIAN_POINT ( 'NONE',  ( 13.97862894411929879, 7.467096638697104716, -19.56757695884047621 ) ) ;
#21828 = ADVANCED_FACE ( 'NONE', ( #27055 ), #20286, .T. ) ;
#21829 = CARTESIAN_POINT ( 'NONE',  ( 159.7287565553229740, -1.999999999999972689, -25.16025403784440329 ) ) ;
#21830 = ORIENTED_EDGE ( 'NONE', *, *, #12892, .F. ) ;
#21831 = ORIENTED_EDGE ( 'NONE', *, *, #8240, .T. ) ;
#21832 = CARTESIAN_POINT ( 'NONE',  ( 35.34711162051457478, -16.78689235204268115, -20.22678452305727603 ) ) ;
#21833 = CARTESIAN_POINT ( 'NONE',  ( 20.64697163712990857, 4.580154932681155699, -17.29389188279686707 ) ) ;
#21834 = CARTESIAN_POINT ( 'NONE',  ( 16.34386185847872142, 4.569898679961749366, -19.52586945278800812 ) ) ;
#21835 = CIRCLE ( 'NONE', #24285, 5.000000000000000888 ) ;
#21836 =( NAMED_UNIT ( * ) PLANE_ANGLE_UNIT ( ) SI_UNIT ( $, .RADIAN. ) );
#21837 = FACE_BOUND ( 'NONE', #6035, .T. ) ;
#21838 = VECTOR ( 'NONE', #3973, 1000.000000000000000 ) ;
#21839 = FACE_OUTER_BOUND ( 'NONE', #14974, .T. ) ;
#21840 = LINE ( 'NONE', #9930, #17929 ) ;
#21841 = LINE ( 'NONE', #28308, #3676 ) ;
#21842 = CARTESIAN_POINT ( 'NONE',  ( 12.25826188308600351, 9.517053581970603915, -15.32321445922237224 ) ) ;
#21843 = CARTESIAN_POINT ( 'NONE',  ( 167.0152310637604955, -4.999999999999972466, -1.854241549900775782E-14 ) ) ;
#21844 = DIRECTION ( 'NONE',  ( 1.000000000000000000, -0.000000000000000000, 0.000000000000000000 ) ) ;
#21845 = EDGE_LOOP ( 'NONE', ( #8019, #4974 ) ) ;
#21846 = CARTESIAN_POINT ( 'NONE',  ( 12.48484057295006977, 8.564241722236854315, -15.14223913367768759 ) ) ;
#21847 = ORIENTED_EDGE ( 'NONE', *, *, #680, .T. ) ;
#21848 = AXIS2_PLACEMENT_3D ( 'NONE', #8673, #3657, #29349 ) ;
#21849 = CARTESIAN_POINT ( 'NONE',  ( 10.53902527060216343, 9.639284983934057749, -16.46481883690060144 ) ) ;
#21850 = CARTESIAN_POINT ( 'NONE',  ( 159.7287565553229172, -1.999999999999973577, -7.839745962155603820 ) ) ;
#21851 = DIRECTION ( 'NONE',  ( 0.5877852522924731371, 0.000000000000000000, 0.8090169943749474513 ) ) ;
#21852 = CARTESIAN_POINT ( 'NONE',  ( -31.74999999999995737, 0.000000000000000000, 0.000000000000000000 ) ) ;
#21853 = CARTESIAN_POINT ( 'NONE',  ( 166.1922820468853104, -9.999999999999998224, -2.083034168790677043 ) ) ;
#21854 = EDGE_LOOP ( 'NONE', ( #1882, #5124, #3943 ) ) ;
#21855 = CARTESIAN_POINT ( 'NONE',  ( 12.83225835781710344, 9.540595166069421040, -16.14103675596956933 ) ) ;
#21856 = EDGE_CURVE ( 'NONE', #19510, #29002, #4128, .T. ) ;
#21857 = EDGE_CURVE ( 'NONE', #23142, #10211, #13122, .T. ) ;
#21858 = VECTOR ( 'NONE', #28867, 1000.000000000000000 ) ;
#21859 = CARTESIAN_POINT ( 'NONE',  ( 34.16485483951214519, -11.28898102658429536, -18.35413676833350038 ) ) ;
#21860 = CARTESIAN_POINT ( 'NONE',  ( 17.08157517049449581, 7.460725202527481947, -14.57009041681831896 ) ) ;
#21861 = ORIENTED_EDGE ( 'NONE', *, *, #6468, .T. ) ;
#21862 = EDGE_CURVE ( 'NONE', #4141, #13418, #12975, .T. ) ;
#21863 = CARTESIAN_POINT ( 'NONE',  ( 175.7287565553229456, -9.999999999999971578, 3.500000000000003109 ) ) ;
#21864 = EDGE_CURVE ( 'NONE', #2741, #21885, #8686, .T. ) ;
#21865 = CARTESIAN_POINT ( 'NONE',  ( 18.16551323082808267, 7.152368624112494189, -14.07085781252208712 ) ) ;
#21866 = LINE ( 'NONE', #20025, #26259 ) ;
#21867 = AXIS2_PLACEMENT_3D ( 'NONE', #6225, #29322, #1510 ) ;
#21868 = LINE ( 'NONE', #22480, #344 ) ;
#21869 = CIRCLE ( 'NONE', #9193, 2.100000000000002753 ) ;
#21870 = CARTESIAN_POINT ( 'NONE',  ( 19.95076809599375878, -1.008983920988137495, -18.52968236344498720 ) ) ;
#21871 = CARTESIAN_POINT ( 'NONE',  ( 21.92347772697934261, 3.537472258236324052, -14.28107661384214211 ) ) ;
#21872 = ORIENTED_EDGE ( 'NONE', *, *, #17787, .F. ) ;
#21873 = CARTESIAN_POINT ( 'NONE',  ( 171.1922820468852819, -1.999999999999970912, -2.083034168790677043 ) ) ;
#21874 = LINE ( 'NONE', #17293, #13791 ) ;
#21875 = CARTESIAN_POINT ( 'NONE',  ( 164.5152310637604955, -4.999999999999973355, -30.37205893520531319 ) ) ;
#21876 = VECTOR ( 'NONE', #22706, 1000.000000000000000 ) ;
#21877 = CARTESIAN_POINT ( 'NONE',  ( 154.5152310637605808, -10.00000000000000000, -28.60870317832789667 ) ) ;
#21878 = CARTESIAN_POINT ( 'NONE',  ( 169.7287565553228887, -1.999999999999970912, -7.839745962155603820 ) ) ;
#21879 = ORIENTED_EDGE ( 'NONE', *, *, #1971, .F. ) ;
#21880 = CARTESIAN_POINT ( 'NONE',  ( 10.04637620539468124, 15.81139305134258599, -16.45082025127570091 ) ) ;
#21881 = VECTOR ( 'NONE', #30123, 1000.000000000000000 ) ;
#21882 = CARTESIAN_POINT ( 'NONE',  ( 25.52642221012979462, -9.988304178644780151, -15.98026830291908773 ) ) ;
#21883 = CARTESIAN_POINT ( 'NONE',  ( 24.79209089726652948, -9.725099617967893906, -18.44766554224525734 ) ) ;
#21885 = VERTEX_POINT ( 'NONE', #27213 ) ;
#21884 = CARTESIAN_POINT ( 'NONE',  ( 32.63711423693117553, -11.05166607373017484, -18.34576405707344549 ) ) ;
#21886 = CLOSED_SHELL ( 'NONE', ( #13508, #28939, #7409, #28879, #26214, #28032, #23048, #9022, #14609, #21994, #6193, #7155, #8418, #21478, #22239, #5585, #14650, #3154, #27693, #11653, #7644, #28360, #18297, #15328, #16006, #28666, #29083, #19683, #1765, #7462, #12686, #8793, #29446, #28496, #25286, #8796, #15243, #15889, #26360, #4290, #14095, #29010, #14125, #17954, #22525, #20549, #12474, #10690, #9332, #19062, #6012, #25042, #11760, #19236, #27553, #4782, #5946, #14675, #15631, #4501, #2761, #21828, #17659, #29975, #30198, #16344, #6681, #13278, #21383, #19514, #25607, #5673, #1077, #9928, #29994, #576, #17371, #3610, #30162, #9125, #27523, #5925, #27397, #1134, #15126, #12960, #12593, #9927, #17038, #10941, #10177, #29471, #28103, #17407, #25738, #15752, #29004, #25911, #19102, #29833, #19684, #1718, #27770, #6984, #16204, #3107, #4571, #4569, #28528, #12412, #18486, #24935, #2858, #22791, #6190, #13283, #2148, #23418, #16055, #17109, #13928, #19644, #524, #22107, #13694, #4952, #607, #22281, #25010, #23994, #12971, #21613, #27433, #23995, #860, #4866, #14011, #2564, #19143, #13142, #26778, #17282, #1800, #30160, #15169, #13977, #346, #12176, #16866, #3898, #4232, #23560, #21681, #13822, #5566, #28557, #28699, #29042, #24873, #28187, #17712, #6230, #3199, #13726, #18242, #29754, #20547, #11859, #22498, #10694, #11715, #21801, #25663, #1626, #24356, #12030, #9584, #1342, #12104, #23770, #25798, #1171, #237, #8033, #8381, #13849, #18103, #29481, #27867, #25661, #13581, #23460, #17284, #10180, #8146, #17035, #24028, #25108, #24323, #24320, #3240, #13695, #25796, #8495, #21823, #16617, #4694, #21594, #27904, #27328, #606, #26434, #28494, #21006, #29325, #24483, #5161, #14341, #8724, #19103, #4441, #2758, #20964, #2940, #99, #19445, #3708, #934, #28585, #28091, #29363, #6912, #6859, #20780, #18725, #14745, #7330, #17318, #14815, #26243, #26395, #23286, #22710, #21512, #526, #19234, #11989, #25612, #22877, #5640, #9371, #18998, #1551, #29865, #28663, #9161, #25452, #1862, #1007, #3859, #21902, #3531, #27901, #10209, #16140, #7288, #29407, #30230, #4663, #195, #26967, #7059, #10267, #2720, #26823, #16306, #1844, #24660, #3823, #17110, #6570, #21552, #23803, #14992, #8655, #17824, #5642, #29208, #12375, #29789, #7940, #17547, #14713, #408, #6443, #6436, #24877, #2213, #8870, #24073, #20586, #5080, #25109, #2531, #10735, #20111, #27181, #28979, #12728, #27859, #15027, #862, #22131, #25288, #13387, #9996, #17399, #27168, #18796, #4610, #18861, #10729, #22843, #10173, #19100, #10272, #23010, #10901, #11409, #6268, #8414, #17957, #4772, #8455, #15514, #9543, #25722, #8241, #3318, #19137, #27184, #25251, #20846, #25700, #17509, #14741, #7153, #3316, #7285, #23735, #8659, #7981, #21197, #7080, #4472, #26260, #17995, #6092, #734, #13980, #8278, #18865, #615, #6367, #18898, #27095, #17956, #4405, #28693, #8109, #19549, #7661, #15515, #12248, #26394, #2141, #7238, #18301, #29791, #19347, #25578, #17679, #24566, #27805, #22135, #24916, #3280, #20409, #30120, #4365, #14654, #15371, #8658, #22668, #24620, #65, #9546, #22940, #20131, #12972, #14504, #10562, #15967, #1173, #10889, #8953, #20001, #22418, #1517, #25791, #20408, #3517, #12034, #26127, #6228, #23282, #1204, #13281, #16441, #30019, #2183, #9018, #17661, #14388, #16702, #18130, #7500, #11315, #11172, #24739, #2492, #29288, #11248, #17625, #4236, #24482, #17249, #13311, #14989, #22708, #16060, #22626, #10374, #1930, #6368, #9440, #7257, #4195, #5195, #23920, #29788, #7740, #27004, #29618, #5253, #25873, #5252, #20583, #19512, #4732 ) ) ;
#21887 = FACE_OUTER_BOUND ( 'NONE', #17132, .T. ) ;
#21888 = DIRECTION ( 'NONE',  ( -2.698458740408365879E-16, 1.000000000000000000, 0.000000000000000000 ) ) ;
#21889 = DIRECTION ( 'NONE',  ( 1.000000000000000000, 0.000000000000000000, 0.000000000000000000 ) ) ;
#21890 = LINE ( 'NONE', #26643, #8291 ) ;
#21891 = CARTESIAN_POINT ( 'NONE',  ( 138.6922820468854241, -10.00000000000000533, 2.247092850131519715 ) ) ;
#21892 = CARTESIAN_POINT ( 'NONE',  ( 129.5152310637605808, -10.00000000000000888, -11.28819510263909187 ) ) ;
#21894 = EDGE_LOOP ( 'NONE', ( #15425, #26694, #7955, #26380 ) ) ;
#21893 = CARTESIAN_POINT ( 'NONE',  ( 15.41431293496917121, 3.575304669039410133, -17.09800041271234150 ) ) ;
#21895 = ORIENTED_EDGE ( 'NONE', *, *, #26018, .T. ) ;
#21896 = DIRECTION ( 'NONE',  ( 1.000000000000000000, 0.000000000000000000, 0.000000000000000000 ) ) ;
#21897 = CARTESIAN_POINT ( 'NONE',  ( 11.95275185645256322, 10.98126796543430572, -15.44474055479659569 ) ) ;
#21898 = CARTESIAN_POINT ( 'NONE',  ( 33.29928106196997817, -12.14339677642331772, -19.64090527578606427 ) ) ;
#21899 = CARTESIAN_POINT ( 'NONE',  ( -2.100000000000000977, -6.754115128641868940E-16, -2.450000000000000178 ) ) ;
#21900 = EDGE_CURVE ( 'NONE', #15422, #29696, #29673, .T. ) ;
#21901 = CARTESIAN_POINT ( 'NONE',  ( 24.79644250101478065, -1.608028467720058918, -19.02763285027648976 ) ) ;
#21902 = ADVANCED_FACE ( 'NONE', ( #17999 ), #25187, .T. ) ;
#21903 = CARTESIAN_POINT ( 'NONE',  ( 17.99875044999096119, -0.3805832805143671838, -17.40611996466761369 ) ) ;
#21904 = ORIENTED_EDGE ( 'NONE', *, *, #7771, .T. ) ;
#21905 = CARTESIAN_POINT ( 'NONE',  ( 35.13870703111577143, -20.34311121210408757, -20.23074448643712486 ) ) ;
#21906 = PRESENTATION_STYLE_ASSIGNMENT (( #17618 ) ) ;
#21907 = VECTOR ( 'NONE', #25985, 1000.000000000000000 ) ;
#21908 = CARTESIAN_POINT ( 'NONE',  ( 29.43474752111978177, -7.508961153211615169, -12.65842848261850229 ) ) ;
#21909 = CARTESIAN_POINT ( 'NONE',  ( 21.04533358917985808, -3.575919577149618167, -19.74844908412899969 ) ) ;
#21910 = VECTOR ( 'NONE', #18114, 1000.000000000000000 ) ;
#21911 = CARTESIAN_POINT ( 'NONE',  ( 26.32595758385100382, -12.12905223104374386, -14.21117607008287642 ) ) ;
#21912 = ORIENTED_EDGE ( 'NONE', *, *, #1004, .F. ) ;
#21913 = CARTESIAN_POINT ( 'NONE',  ( 16.08363025263714263, -5.000000000000013323, -49.50032404655522811 ) ) ;
#21914 = ORIENTED_EDGE ( 'NONE', *, *, #11992, .T. ) ;
#21915 = ORIENTED_EDGE ( 'NONE', *, *, #20270, .F. ) ;
#21916 = CARTESIAN_POINT ( 'NONE',  ( 130.7287565553229172, -4.999999999999983125, -19.55415080639416203 ) ) ;
#21917 = DIRECTION ( 'NONE',  ( -2.698458740408365879E-16, 1.000000000000000000, 0.000000000000000000 ) ) ;
#21918 = CARTESIAN_POINT ( 'NONE',  ( 27.31974442496251143, -5.660127319198639206, -14.41990313654811651 ) ) ;
#21919 = DIRECTION ( 'NONE',  ( 0.000000000000000000, 0.000000000000000000, 1.000000000000000000 ) ) ;
#21920 = CARTESIAN_POINT ( 'NONE',  ( 36.02474454408307736, -19.83113812547715682, -20.43161669954002591 ) ) ;
#21921 = AXIS2_PLACEMENT_3D ( 'NONE', #25951, #7622, #19212 ) ;
#21922 = CARTESIAN_POINT ( 'NONE',  ( 10.95411528722473626, 11.64838591225006859, -16.07543820933196699 ) ) ;
#21923 = DIRECTION ( 'NONE',  ( -0.9510565162951536422, -2.566386769018988323E-16, 0.3090169943749475623 ) ) ;
#21924 = CARTESIAN_POINT ( 'NONE',  ( 158.6922820468853672, -10.00000000000000000, -17.92658477444275889 ) ) ;
#21925 = CARTESIAN_POINT ( 'NONE',  ( 12.35422140817580683, 8.720385185214494683, -16.48779044034850116 ) ) ;
#21926 = DIRECTION ( 'NONE',  ( 0.000000000000000000, 0.000000000000000000, 1.000000000000000000 ) ) ;
#21927 =( GEOMETRIC_REPRESENTATION_CONTEXT ( 3 ) GLOBAL_UNCERTAINTY_ASSIGNED_CONTEXT ( ( #1596 ) ) GLOBAL_UNIT_ASSIGNED_CONTEXT ( ( #3021, #10003, #12600 ) ) REPRESENTATION_CONTEXT ( 'NONE', 'WORKASPACE' ) );
#21928 = FACE_OUTER_BOUND ( 'NONE', #18857, .T. ) ;
#21929 = ORIENTED_EDGE ( 'NONE', *, *, #27009, .F. ) ;
#21930 = CARTESIAN_POINT ( 'NONE',  ( 144.5152310637605808, -4.999999999999978684, -1.604441369360116507E-14 ) ) ;
#21931 = DIRECTION ( 'NONE',  ( -0.9510565162951536422, -2.566386769018988323E-16, 0.3090169943749475623 ) ) ;
#21932 = ADVANCED_FACE ( 'NONE', ( #8391 ), #17857, .T. ) ;
#21933 = EDGE_CURVE ( 'NONE', #12771, #30193, #20140, .T. ) ;
#21934 = CARTESIAN_POINT ( 'NONE',  ( 147.0152310637605524, -4.999999999999977796, -17.38167787843871182 ) ) ;
#21935 = ORIENTED_EDGE ( 'NONE', *, *, #2042, .F. ) ;
#21936 = ADVANCED_FACE ( 'NONE', ( #26904 ), #3673, .T. ) ;
#21937 = VERTEX_POINT ( 'NONE', #2152 ) ;
#21938 = EDGE_CURVE ( 'NONE', #619, #9664, #23051, .T. ) ;
#21939 = CARTESIAN_POINT ( 'NONE',  ( 12.82830918206423121, 7.509569466653498004, -16.13756579491948173 ) ) ;
#21940 = ORIENTED_EDGE ( 'NONE', *, *, #16736, .T. ) ;
#21941 = CARTESIAN_POINT ( 'NONE',  ( 14.35528768574272895, 10.45889919667044410, -14.17515447063821910 ) ) ;
#21942 = VECTOR ( 'NONE', #8298, 1000.000000000000000 ) ;
#21943 = CARTESIAN_POINT ( 'NONE',  ( 26.64416741123070054, -12.70369174447049332, -17.39020166599120643 ) ) ;
#21944 = CARTESIAN_POINT ( 'NONE',  ( 164.5152310637604671, -1.999999999999972244, -11.28819510263909542 ) ) ;
#21945 = LINE ( 'NONE', #29157, #8216 ) ;
#21946 =( BOUNDED_SURFACE ( )  B_SPLINE_SURFACE ( 3, 3, ( 
 ( #20540, #17795, #4226, #29929, #30070, #13675, #23001, #9082, #13075, #22396, #1500, #20835, #19012, #23753, #9846, #9533, #9688, #2250, #20992, #14262, #28219, #2850, #18556, #12136, #5120, #100, #2558, #30218, #28369, #9228, #7424, #403, #16724, #16868, #26044, #4971, #27912, #21453, #16417, #13961, #6971, #19159, #255, #18856, #28515, #7564, #23594, #14413, #4818, #4524, #561, #7268, #9385, #16258, #18711, #13811, #28059, #7112, #16572, #11676, #25571, #25894, #25736, #23141, #11523, #2402, #14114, #4669, #23291, #2693, #23445, #11829, #21144, #11976, #21296, #12431, #15167, #8308, #17172, #8007, #10293, #9988, #3591, #3008, #1159, #14716, #5429, #12583, #3446, #26199, #29117, #24058, #853, #17463, #26812, #5887, #5277, #3158, #24503, #10439, #12882, #22057, #5734, #19601, #22197, #26350, #702, #8158, #21750, #15017, #12736, #19304, #1309, #24347, #28664, #10142, #19455, #10597, #7715, #1016, #17024, #19908, #28825, #29272, #12285, #19748, #14564, #23913, #28971, #21605, #7862, #26501, #5581, #17314, #14864, #24204, #3307, #21901, #26655, #15627, #13041, #11195, #22357, #20506, #13484, #22813, #182, #1917, #18067, #1462, #6627, #29585, #27117, #10753, #2065, #13337, #1763, #11345, #20648, #6483, #29891, #17903, #17613, #8899, #22659, #13193, #20060, #3894, #22964, #22515, #20205, #29742, #24807, #29435, #11050, #8603, #18216, #25252, #15474, #27282, #27571, #6179, #20352, #8457, #26972, #1615, #6030, #10893, #6332, #15920, #15314, #24961, #8748, #27428, #17761, #4337, #24647, #13635, #4041, #15772, #25097, #4188, #3741, #12354, #18937, #14337, #769, #10066, #19378, #18785, #7347, #28742, #3085, #16795, #21529, #21667, #23673, #14787, #7788, #16490, #24127, #12059, #5502, #334, #19087, #26122, #28293, #17097, #16648, #9769, #14641, #25965, #23831, #14193, #3225, #2777, #12503, #5046, #21372, #26422, #21826, #480, #630, #2929, #23519, #9461 ),
 ( #28139, #28438, #7490, #7196, #25816, #4897, #2628, #5200, #11903, #21219, #14494, #9915, #9619, #12209, #19226, #28583, #7637, #16944, #26273, #5355, #23988, #10514, #8228, #19673, #15397, #1539, #27048, #10677, #24578, #22439, #1091, #5657, #13113, #8078, #19986, #8383, #14939, #20133, #29357, #24274, #10368, #17387, #29511, #3373, #5958, #12660, #10822, #21978, #8532, #17242, #24731, #17833, #6256, #15246, #6103, #28900, #26732, #17689, #3666, #27205, #29038, #15551, #24886, #5804, #29191, #26573, #3819, #15089, #3971, #13270, #926, #10218, #19529, #1386, #24425, #7931, #12813, #3520, #22126, #1230, #26894, #12962, #19828, #17538, #22277, #27798, #22894, #16295, #16152, #27644, #18143, #15703, #8830, #27949, #27505, #25177, #4420, #29822, #25032, #6712, #4268, #13850, #2142, #20580, #18598, #25608, #27358, #4118, #6414, #23040, #13568, #25470, #20430, #16000, #13413, #22738, #4704, #29965, #30258, #6556, #1996, #11559, #7006, #11416, #4561, #20721, #20876, #9270, #8972, #23176, #15847, #1851, #11275, #22587, #17986, #11129, #1688, #18287, #25329, #10969, #13714, #2288, #30108, #9118, #20278, #29665, #8680, #6865, #18449, #19191, #23792, #11717, #9879, #14155, #19048, #23634, #19339, #5011, #23483, #13997, #21632, #4854, #14453, #28403, #14300, #2889, #441, #9573, #28704, #12171, #7752, #7457, #28547, #2590, #18896, #28253, #16453, #25776, #7598, #729, #7303, #11866, #23326, #21179, #21490, #290, #12016, #2733, #16760, #16904, #26082, #594, #16608, #25929, #9420, #18745, #21334, #26235, #5315, #14599, #23953, #3044, #17061, #9726, #12316, #5163, #10026, #26389, #2439, #21034, #140, #28093, #7154, #12622, #10640, #19950, #24240, #8351, #5772, #12923, #27015, #3784, #21792, #28865, #15053, #12776, #3341, #3488, #29318, #17653, #26539, #14753, #24091, #3192, #6070, #13080, #15356, #15210, #12469, #1351, #5619, #10479, #24387, #10795, #26697, #14899 ),
 ( #20102, #8043, #1506, #21941, #22093, #1198, #1055, #24695, #22402, #29480, #24543, #29153, #8500, #10331, #10183, #17799, #19639, #3630, #22241, #19494, #5467, #891, #7900, #29005, #17352, #17210, #19788, #8194, #17504, #26857, #5924, #16118, #13238, #11385, #25438, #2255, #1959, #2110, #24849, #13378, #6674, #20546, #4529, #10934, #13819, #27763, #22702, #25139, #22558, #20690, #1657, #30075, #23006, #9088, #9233, #18412, #27611, #20245, #23145, #8794, #6379, #29632, #11528, #22857, #11240, #20841, #30224, #15964, #6829, #27470, #27162, #6221, #29933, #1810, #8644, #11091, #15517, #20393, #29783, #8940, #4085, #17948, #18256, #18108, #3935, #27324, #25002, #6524, #15669, #15814, #25294, #4231, #13531, #4382, #13681, #28064, #4825, #7568, #707, #9537, #410, #2698, #2408, #26203, #23602, #14121, #11683, #23451, #23919, #2562, #21148, #9694, #25741, #20998, #11981, #259, #9850, #5281, #16422, #18864, #23757, #7119, #21301, #23295, #3013, #11836, #12289, #28223, #7274, #16874, #18564, #16576, #19019, #28374, #108, #14569, #25577, #2854, #25900, #4976, #14267, #26049, #27916, #21457, #7428, #16729, #19163, #28520, #21609, #6975, #5128, #16263, #12142, #14417, #566, #4673, #13965, #9390, #18716, #17029, #15322, #12588, #6037, #858, #19607, #17321, #28829, #24508, #10604, #5892, #19754, #3452, #1314, #10148, #14720, #22204, #17178, #29123, #17469, #24063, #29278, #8163, #3164, #19461, #26506, #8314, #12435, #15022, #21757, #19915, #7867, #17619, #26355, #3596, #26978, #24654, #24354, #15173, #7719, #5588, #26819, #12743, #3748, #14869, #13046, #22365, #24209, #8013, #5436, #12889, #3311, #9993, #19308, #28671, #21908, #1022, #10447, #10300, #28978, #26661, #5739, #22062, #1164, #27435, #15778, #25404, #4496, #20512, #6632, #1770, #13787, #25258, #17909, #20656, #1468, #22666, #13491, #25103, #15482, #9047, #8466, #15925, #20212, #10899, #18073, #8906 ),
 ( #6790, #11055, #1620, #10758, #18371, #22523, #1923, #6488, #20357, #11202, #4193, #27288, #16079, #29897, #20066, #22820, #4343, #29593, #6338, #15635, #3901, #13200, #13642, #27728, #24969, #8609, #29442, #4047, #18223, #13342, #29748, #8757, #27577, #22970, #2073, #11350, #30041, #17768, #27124, #6185, #24812, #5093, #9662, #18985, #28341, #7394, #7532, #4641, #23566, #2373, #9354, #18825, #7242, #16692, #23263, #16539, #25863, #73, #26016, #14381, #11646, #23718, #23412, #375, #2820, #21420, #9200, #16233, #2528, #223, #20961, #21116, #12106, #530, #2664, #9501, #19127, #26167, #27884, #25547, #6941, #11943, #14081, #9815, #18680, #4941, #13932, #28028, #5242, #28184, #28484, #7086, #11799, #16837, #23113, #21262, #2222, #11492, #20805, #30191, #14233, #18530, #16381, #25706, #4791, #29237, #9955, #23880, #12399, #3563, #8126, #21870, #26622, #17430, #19423, #19871, #12854, #21572, #8272, #17142, #10567, #5400, #24170, #978, #3126, #29088, #15137, #10412, #24319, #7977, #5849, #14686, #19271, #26780, #21712, #3413, #22025, #28627, #22168, #12704, #7682, #24030, #816, #1275, #16990, #19574, #26315, #24467, #10111, #17584, #670, #26940, #14535, #2979, #28941, #19717, #12255, #28789, #1131, #17287, #7833, #26470, #5554, #14832, #3272, #12548, #10261, #5700, #14982, #29862, #1887, #11168, #18332, #20474, #6451, #20028, #25222, #17869, #15443, #29402, #20625, #1730, #20317, #30004, #9010, #25067, #8872, #6297, #5996, #18186, #11013, #1582, #8426, #22482, #11313, #10862, #8570, #18032, #13158, #17727, #29706, #27248, #27543, #13606, #3864, #15595, #6596, #24772, #8719, #10717, #15284, #20172, #24615, #29553, #24928, #4307, #3710, #4008, #27401, #15742, #27086, #22936, #13006, #15890, #13306, #22627, #4155, #13452, #22325, #2038, #22780, #1429, #6146, #18946, #7354, #20765, #12065, #23373, #11765, #21380, #492, #16497, #2633, #27993, #9777, #21225 ),
 ( #5054, #25516, #7053, #16654, #2783, #7205, #9624, #25823, #25975, #14343, #14044, #28299, #4607, #30154, #23223, #27692, #23082, #9163, #23679, #18492, #13898, #6751, #18791, #16042, #16342, #27846, #25368, #4461, #13752, #11908, #2186, #340, #4903, #11454, #23528, #6908, #2493, #25666, #16199, #18647, #2337, #11607, #20923, #37, #28147, #21082, #4754, #14202, #189, #9322, #9469, #17252, #13243, #3233, #3378, #19235, #23998, #3093, #21535, #636, #12668, #6227, #12363, #7647, #28445, #16951, #19538, #26279, #17104, #28753, #12512, #24282, #21833, #7938, #21675, #9923, #14500, #23838, #7798, #1098, #5664, #14945, #21986, #10375, #3941, #28592, #28907, #5364, #14647, #14795, #938, #19681, #777, #10225, #26581, #10071, #29048, #8084, #19385, #17805, #26430, #27167, #15525, #24854, #5208, #12220, #5515, #24134, #22565, #1663, #19092, #7499, #16800, #26130, #2935, #8801, #11244, #16122, #20398, #25298, #15673, #16266, #25144, #25581, #29787, #27474, #30228, #23298, #1962, #23009, #4386, #25007, #18569, #17953, #25441, #18111, #6527, #27616, #18416, #10942, #13825, #15817, #4237, #2260, #11531, #20845, #20249, #13535, #9239, #4533, #18259, #2116, #23148, #22860, #4676, #27918, #27330, #13967, #20551, #6978, #1814, #29937, #6677, #8943, #29636, #8649, #6832, #20693, #13685, #6384, #11096, #4089, #13382, #15972, #30080, #27771, #22711, #11388, #9091, #28066, #14124, #11839, #28523, #16425, #21303, #25745, #569, #7124, #7574, #9393, #2857, #16878, #5285, #11985, #23760, #111, #21150, #7431, #414, #26205, #4828, #14572, #9854, #262, #14274, #18718, #12147, #23455, #21459, #19167, #23923, #12293, #3016, #16732, #2567, #2412, #16579, #9542, #18867, #11685, #9697, #19021, #21005, #28226, #7277, #25903, #4979, #23605, #2701, #28378, #26055, #5131, #14422, #4774, #25238, #2053, #11473, #28011, #16061, #56, #6615, #1905, #4324, #14066, #25086, #11185 ),
 ( #4623, #18202, #8888, #25388, #6924, #11780, #2358, #27562, #13622, #20942, #9338, #18666, #8738, #15908, #7070, #23244, #6768, #20790, #11629, #22953, #23396, #16365, #6471, #2513, #11333, #25686, #20494, #9031, #4479, #20638, #13915, #29730, #25531, #9183, #23098, #18055, #29880, #4176, #27418, #30021, #18509, #16217, #13470, #15762, #27868, #22800, #18354, #27711, #13770, #2201, #30175, #23548, #3110, #25847, #10090, #7224, #5382, #19404, #26450, #26150, #26298, #18810, #7379, #656, #14518, #28773, #4926, #7816, #21696, #16674, #19112, #16520, #14668, #14218, #24014, #16973, #12384, #3257, #801, #21555, #2651, #17124, #2805, #360, #11926, #5531, #16816, #5225, #14812, #24153, #9940, #21101, #21404, #206, #9486, #23861, #25997, #21248, #5073, #28167, #14366, #23701, #2959, #28320, #9645, #12238, #12086, #18964, #508, #9797, #28467, #7515, #19252, #28609, #7666, #30053, #14247, #25419, #23123, #23578, #18388, #4508, #28199, #21276, #30204, #20975, #23273, #22983, #16554, #15943, #14096, #27743, #6803, #25556, #16397, #8917, #11812, #16092, #13797, #239, #9516, #18838, #18233, #2232, #7255, #2542, #16244, #84, #21127, #11504, #2674, #25878, #25270, #11960, #20820, #4957, #9063, #18540, #4651, #9213, #23429, #27591, #4803, #18696, #2388, #6649, #27894, #13659, #4356, #6956, #28041, #25720, #2086, #11362, #7097, #20666, #13943, #11661, #9365, #2834, #5414, #12120, #12563, #5105, #19585, #16710, #14844, #28954, #5719, #14699, #5564, #28354, #16853, #10125, #24041, #7990, #14395, #17298, #993, #26180, #28644, #26031, #24187, #23737, #3288, #26484, #21882, #12717, #10276, #834, #21435, #26637, #12268, #9828, #546, #14999, #26331, #3140, #24333, #3426, #19435, #388, #686, #9674, #18996, #12415, #5261, #19144, #14549, #7410, #23896, #2993, #21731, #7549, #28501, #28808, #21587, #9973, #19288, #7695, #17008, #7846, #17155, #18010, #25051, #4287 ),
 ( #11434, #6431, #4138, #11147, #22180, #24480, #27379, #6887, #17447, #3578, #20744, #12867, #29684, #16176, #13589, #2160, #22757, #1705, #1143, #10423, #19732, #27666, #30133, #6729, #2016, #29100, #18310, #10988, #27524, #1869, #27820, #13430, #20296, #22039, #9140, #8699, #22913, #6579, #20450, #11295, #8848, #15723, #25497, #20599, #4586, #15867, #16020, #29843, #18163, #25197, #29982, #8992, #25345, #18468, #4437, #13734, #8139, #23061, #26796, #5867, #15149, #23502, #28274, #19071, #7331, #2757, #16472, #4728, #9297, #18622, #2611, #26104, #463, #9750, #28424, #7476, #28567, #25638, #14320, #23351, #163, #9600, #16629, #16779, #14022, #25949, #5029, #21058, #5182, #14476, #2465, #23815, #14175, #21358, #2913, #12193, #10, #7030, #11886, #21200, #11740, #316, #21509, #616, #23656, #18921, #9900, #16925, #27969, #16321, #9442, #12044, #4879, #19210, #18768, #7620, #28121, #26255, #13876, #7180, #23198, #2315, #25799, #11585, #20899, #24562, #7770, #10355, #17083, #17524, #10047, #3652, #21651, #19811, #12948, #10662, #19659, #10499, #3063, #21811, #15072, #29024, #22261, #19361, #1370, #5943, #909, #3358, #750, #29177, #28722, #8213, #1216, #26879, #17676, #15228, #5790, #26406, #19971, #17229, #14768, #5486, #29342, #1076, #8062, #8369, #5340, #24411, #14625, #5643, #23973, #12339, #17373, #10200, #24111, #19513, #3210, #28887, #7919, #26718, #12488, #26556, #3506, #14921, #24261, #12644, #21963, #12798, #22114, #8519, #17820, #2129, #13257, #10955, #11399, #6244, #22576, #15985, #9104, #17972, #8816, #11112, #10811, #4403, #3805, #1981, #15539, #24870, #13398, #4253, #27032, #29948, #3959, #1676, #18273, #27631, #6696, #6088, #20265, #25312, #20565, #4104, #18124, #8957, #29651, #20707, #13702, #13096, #30095, #8667, #23027, #27191, #6399, #22726, #27344, #11262, #15385, #22875, #6542, #20416, #24718, #15690, #25019, #22425, #1830, #29807 ) ),
 .UNSPECIFIED., .T., .F., .F. ) 
 B_SPLINE_SURFACE_WITH_KNOTS ( ( 4, 3, 4 ),
 ( 4, 2, 2, 2, 2, 2, 2, 2, 2, 2, 2, 2, 2, 2, 2, 2, 2, 2, 2, 2, 2, 2, 2, 2, 2, 2, 2, 2, 2, 2, 2, 2, 2, 2, 2, 2, 2, 2, 2, 2, 2, 2, 2, 2, 2, 2, 2, 2, 2, 2, 2, 2, 2, 2, 2, 2, 2, 2, 2, 2, 2, 2, 2, 2, 2, 2, 2, 2, 2, 2, 2, 2, 2, 2, 2, 2, 2, 2, 2, 2, 2, 2, 2, 2, 2, 2, 2, 2, 2, 2, 2, 2, 2, 2, 2, 2, 2, 2, 2, 2, 2, 2, 2, 2, 2, 2, 2, 2, 2, 2, 2, 2, 2, 2, 2, 2, 2, 2, 2, 2, 2, 2, 4 ),
 ( 0.000000000000000000, 0.5000000000000000000, 1.000000000000000000 ),
 ( 0.000000000000000000, 0.007812500000000000000, 0.01464843750000000000, 0.02148437500000000000, 0.02832031250000000000, 0.03515625000000000000, 0.04882812500000000000, 0.05566406250000000000, 0.06250000000000000000, 0.06933593750000000000, 0.07617187500000000000, 0.08984375000000000000, 0.09667968750000000000, 0.1035156250000000000, 0.1103515625000000000, 0.1171875000000000000, 0.1240234375000000000, 0.1308593750000000000, 0.1376953125000000000, 0.1445312500000000000, 0.1513671875000000000, 0.1582031250000000000, 0.1718750000000000000, 0.1787109375000000000, 0.1855468750000000000, 0.1992187500000000000, 0.2060546875000000000, 0.2128906250000000000, 0.2197265625000000000, 0.2265625000000000000, 0.2402343750000000000, 0.2470703125000000000, 0.2539062500000000000, 0.2607421875000000000, 0.2675781250000000000, 0.2812500000000000000, 0.2880859375000000000, 0.2949218750000000000, 0.3017578125000000000, 0.3085937500000000000, 0.3154296875000000000, 0.3222656250000000000, 0.3291015625000000000, 0.3359375000000000000, 0.3496093750000000000, 0.3564453125000000000, 0.3632812500000000000, 0.3701171875000000000, 0.3769531250000000000, 0.3906250000000000000, 0.3974609375000000000, 0.4042968750000000000, 0.4179687500000000000, 0.4316406250000000000, 0.4384765625000000000, 0.4453125000000000000, 0.4521484375000000000, 0.4589843750000000000, 0.4658203125000000000, 0.4726562500000000000, 0.4794921875000000000, 0.4863281250000000000, 0.4931640625000000000, 0.5000000000000000000, 0.5078125000000000000, 0.5156250000000000000, 0.5234375000000000000, 0.5312500000000000000, 0.5390625000000000000, 0.5468750000000000000, 0.5625000000000000000, 0.5693359375000000000, 0.5761718750000000000, 0.5898437500000000000, 0.5966796875000000000, 0.6035156250000000000, 0.6103515625000000000, 0.6171875000000000000, 0.6308593750000000000, 0.6376953125000000000, 0.6445312500000000000, 0.6513671875000000000, 0.6582031250000000000, 0.6718750000000000000, 0.6787109375000000000, 0.6855468750000000000, 0.6992187500000000000, 0.7128906250000000000, 0.7197265625000000000, 0.7265625000000000000, 0.7333984375000000000, 0.7402343750000000000, 0.7470703125000000000, 0.7539062500000000000, 0.7607421875000000000, 0.7675781250000000000, 0.7744140625000000000, 0.7812500000000000000, 0.7890625000000000000, 0.7968750000000000000, 0.8046875000000000000, 0.8125000000000000000, 0.8203125000000000000, 0.8281250000000000000, 0.8437500000000000000, 0.8505859375000000000, 0.8574218750000000000, 0.8710937500000000000, 0.8779296875000000000, 0.8847656250000000000, 0.8916015625000000000, 0.8984375000000000000, 0.9121093750000000000, 0.9189453125000000000, 0.9257812500000000000, 0.9326171875000000000, 0.9394531250000000000, 0.9531250000000000000, 0.9589843750000000000, 0.9648437500000000000, 0.9765625000000000000, 0.9882812500000000000, 1.000000000000000000 ),
 .UNSPECIFIED. ) 
 GEOMETRIC_REPRESENTATION_ITEM ( )  RATIONAL_B_SPLINE_SURFACE ( (
 ( 1.000000000000000000, 1.000000000000000000, 1.000000000000000000, 1.000000000000000000, 1.000000000000000000, 1.000000000000000000, 1.000000000000000000, 1.000000000000000000, 1.000000000000000000, 1.000000000000000000, 1.000000000000000000, 1.000000000000000000, 1.000000000000000000, 1.000000000000000000, 1.000000000000000000, 1.000000000000000000, 1.000000000000000000, 1.000000000000000000, 1.000000000000000000, 1.000000000000000000, 1.000000000000000000, 1.000000000000000000, 1.000000000000000000, 1.000000000000000000, 1.000000000000000000, 1.000000000000000000, 1.000000000000000000, 1.000000000000000000, 1.000000000000000000, 1.000000000000000000, 1.000000000000000000, 1.000000000000000000, 1.000000000000000000, 1.000000000000000000, 1.000000000000000000, 1.000000000000000000, 1.000000000000000000, 1.000000000000000000, 1.000000000000000000, 1.000000000000000000, 1.000000000000000000, 1.000000000000000000, 1.000000000000000000, 1.000000000000000000, 1.000000000000000000, 1.000000000000000000, 1.000000000000000000, 1.000000000000000000, 1.000000000000000000, 1.000000000000000000, 1.000000000000000000, 1.000000000000000000, 1.000000000000000000, 1.000000000000000000, 1.000000000000000000, 1.000000000000000000, 1.000000000000000000, 1.000000000000000000, 1.000000000000000000, 1.000000000000000000, 1.000000000000000000, 1.000000000000000000, 1.000000000000000000, 1.000000000000000000, 1.000000000000000000, 1.000000000000000000, 1.000000000000000000, 1.000000000000000000, 1.000000000000000000, 1.000000000000000000, 1.000000000000000000, 1.000000000000000000, 1.000000000000000000, 1.000000000000000000, 1.000000000000000000, 1.000000000000000000, 1.000000000000000000, 1.000000000000000000, 1.000000000000000000, 1.000000000000000000, 1.000000000000000000, 1.000000000000000000, 1.000000000000000000, 1.000000000000000000, 1.000000000000000000, 1.000000000000000000, 1.000000000000000000, 1.000000000000000000, 1.000000000000000000, 1.000000000000000000, 1.000000000000000000, 1.000000000000000000, 1.000000000000000000, 1.000000000000000000, 1.000000000000000000, 1.000000000000000000, 1.000000000000000000, 1.000000000000000000, 1.000000000000000000, 1.000000000000000000, 1.000000000000000000, 1.000000000000000000, 1.000000000000000000, 1.000000000000000000, 1.000000000000000000, 1.000000000000000000, 1.000000000000000000, 1.000000000000000000, 1.000000000000000000, 1.000000000000000000, 1.000000000000000000, 1.000000000000000000, 1.000000000000000000, 1.000000000000000000, 1.000000000000000000, 1.000000000000000000, 1.000000000000000000, 1.000000000000000000, 1.000000000000000000, 1.000000000000000000, 1.000000000000000000, 1.000000000000000000, 1.000000000000000000, 1.000000000000000000, 1.000000000000000000, 1.000000000000000000, 1.000000000000000000, 1.000000000000000000, 1.000000000000000000, 1.000000000000000000, 1.000000000000000000, 1.000000000000000000, 1.000000000000000000, 1.000000000000000000, 1.000000000000000000, 1.000000000000000000, 1.000000000000000000, 1.000000000000000000, 1.000000000000000000, 1.000000000000000000, 1.000000000000000000, 1.000000000000000000, 1.000000000000000000, 1.000000000000000000, 1.000000000000000000, 1.000000000000000000, 1.000000000000000000, 1.000000000000000000, 1.000000000000000000, 1.000000000000000000, 1.000000000000000000, 1.000000000000000000, 1.000000000000000000, 1.000000000000000000, 1.000000000000000000, 1.000000000000000000, 1.000000000000000000, 1.000000000000000000, 1.000000000000000000, 1.000000000000000000, 1.000000000000000000, 1.000000000000000000, 1.000000000000000000, 1.000000000000000000, 1.000000000000000000, 1.000000000000000000, 1.000000000000000000, 1.000000000000000000, 1.000000000000000000, 1.000000000000000000, 1.000000000000000000, 1.000000000000000000, 1.000000000000000000, 1.000000000000000000, 1.000000000000000000, 1.000000000000000000, 1.000000000000000000, 1.000000000000000000, 1.000000000000000000, 1.000000000000000000, 1.000000000000000000, 1.000000000000000000, 1.000000000000000000, 1.000000000000000000, 1.000000000000000000, 1.000000000000000000, 1.000000000000000000, 1.000000000000000000, 1.000000000000000000, 1.000000000000000000, 1.000000000000000000, 1.000000000000000000, 1.000000000000000000, 1.000000000000000000, 1.000000000000000000, 1.000000000000000000, 1.000000000000000000, 1.000000000000000000, 1.000000000000000000, 1.000000000000000000, 1.000000000000000000, 1.000000000000000000, 1.000000000000000000, 1.000000000000000000, 1.000000000000000000, 1.000000000000000000, 1.000000000000000000, 1.000000000000000000, 1.000000000000000000, 1.000000000000000000, 1.000000000000000000, 1.000000000000000000, 1.000000000000000000, 1.000000000000000000, 1.000000000000000000, 1.000000000000000000, 1.000000000000000000, 1.000000000000000000, 1.000000000000000000, 1.000000000000000000, 1.000000000000000000, 1.000000000000000000, 1.000000000000000000, 1.000000000000000000, 1.000000000000000000, 1.000000000000000000, 1.000000000000000000, 1.000000000000000000, 1.000000000000000000, 1.000000000000000000, 1.000000000000000000, 1.000000000000000000, 1.000000000000000000, 1.000000000000000000, 1.000000000000000000, 1.000000000000000000, 1.000000000000000000, 1.000000000000000000, 1.000000000000000000, 1.000000000000000000, 1.000000000000000000, 1.000000000000000000, 1.000000000000000000, 1.000000000000000000, 1.000000000000000000, 1.000000000000000000),
 ( 0.3333333333333333703, 0.3333333333333333703, 0.3333333333333333703, 0.3333333333333333703, 0.3333333333333333703, 0.3333333333333333703, 0.3333333333333333703, 0.3333333333333333703, 0.3333333333333333703, 0.3333333333333333703, 0.3333333333333333703, 0.3333333333333333703, 0.3333333333333333703, 0.3333333333333333703, 0.3333333333333333703, 0.3333333333333333703, 0.3333333333333333703, 0.3333333333333333703, 0.3333333333333333703, 0.3333333333333333703, 0.3333333333333333703, 0.3333333333333333703, 0.3333333333333333703, 0.3333333333333333703, 0.3333333333333333703, 0.3333333333333333703, 0.3333333333333333703, 0.3333333333333333703, 0.3333333333333333703, 0.3333333333333333703, 0.3333333333333333703, 0.3333333333333333703, 0.3333333333333333703, 0.3333333333333333703, 0.3333333333333333703, 0.3333333333333333703, 0.3333333333333333703, 0.3333333333333333703, 0.3333333333333333703, 0.3333333333333333703, 0.3333333333333333703, 0.3333333333333333703, 0.3333333333333333703, 0.3333333333333333703, 0.3333333333333333703, 0.3333333333333333703, 0.3333333333333333703, 0.3333333333333333703, 0.3333333333333333703, 0.3333333333333333703, 0.3333333333333333703, 0.3333333333333333703, 0.3333333333333333703, 0.3333333333333333703, 0.3333333333333333703, 0.3333333333333333703, 0.3333333333333333703, 0.3333333333333333703, 0.3333333333333333703, 0.3333333333333333703, 0.3333333333333333703, 0.3333333333333333703, 0.3333333333333333703, 0.3333333333333333703, 0.3333333333333333703, 0.3333333333333333703, 0.3333333333333333703, 0.3333333333333333703, 0.3333333333333333703, 0.3333333333333333703, 0.3333333333333333703, 0.3333333333333333703, 0.3333333333333333703, 0.3333333333333333703, 0.3333333333333333703, 0.3333333333333333703, 0.3333333333333333703, 0.3333333333333333703, 0.3333333333333333703, 0.3333333333333333703, 0.3333333333333333703, 0.3333333333333333703, 0.3333333333333333703, 0.3333333333333333703, 0.3333333333333333703, 0.3333333333333333703, 0.3333333333333333703, 0.3333333333333333703, 0.3333333333333333703, 0.3333333333333333703, 0.3333333333333333703, 0.3333333333333333703, 0.3333333333333333703, 0.3333333333333333703, 0.3333333333333333703, 0.3333333333333333703, 0.3333333333333333703, 0.3333333333333333703, 0.3333333333333333703, 0.3333333333333333703, 0.3333333333333333703, 0.3333333333333333703, 0.3333333333333333703, 0.3333333333333333703, 0.3333333333333333703, 0.3333333333333333703, 0.3333333333333333703, 0.3333333333333333703, 0.3333333333333333703, 0.3333333333333333703, 0.3333333333333333703, 0.3333333333333333703, 0.3333333333333333703, 0.3333333333333333703, 0.3333333333333333703, 0.3333333333333333703, 0.3333333333333333703, 0.3333333333333333703, 0.3333333333333333703, 0.3333333333333333703, 0.3333333333333333703, 0.3333333333333333703, 0.3333333333333333703, 0.3333333333333333703, 0.3333333333333333703, 0.3333333333333333703, 0.3333333333333333703, 0.3333333333333333703, 0.3333333333333333703, 0.3333333333333333703, 0.3333333333333333703, 0.3333333333333333703, 0.3333333333333333703, 0.3333333333333333703, 0.3333333333333333703, 0.3333333333333333703, 0.3333333333333333703, 0.3333333333333333703, 0.3333333333333333703, 0.3333333333333333703, 0.3333333333333333703, 0.3333333333333333703, 0.3333333333333333703, 0.3333333333333333703, 0.3333333333333333703, 0.3333333333333333703, 0.3333333333333333703, 0.3333333333333333703, 0.3333333333333333703, 0.3333333333333333703, 0.3333333333333333703, 0.3333333333333333703, 0.3333333333333333703, 0.3333333333333333703, 0.3333333333333333703, 0.3333333333333333703, 0.3333333333333333703, 0.3333333333333333703, 0.3333333333333333703, 0.3333333333333333703, 0.3333333333333333703, 0.3333333333333333703, 0.3333333333333333703, 0.3333333333333333703, 0.3333333333333333703, 0.3333333333333333703, 0.3333333333333333703, 0.3333333333333333703, 0.3333333333333333703, 0.3333333333333333703, 0.3333333333333333703, 0.3333333333333333703, 0.3333333333333333703, 0.3333333333333333703, 0.3333333333333333703, 0.3333333333333333703, 0.3333333333333333703, 0.3333333333333333703, 0.3333333333333333703, 0.3333333333333333703, 0.3333333333333333703, 0.3333333333333333703, 0.3333333333333333703, 0.3333333333333333703, 0.3333333333333333703, 0.3333333333333333703, 0.3333333333333333703, 0.3333333333333333703, 0.3333333333333333703, 0.3333333333333333703, 0.3333333333333333703, 0.3333333333333333703, 0.3333333333333333703, 0.3333333333333333703, 0.3333333333333333703, 0.3333333333333333703, 0.3333333333333333703, 0.3333333333333333703, 0.3333333333333333703, 0.3333333333333333703, 0.3333333333333333703, 0.3333333333333333703, 0.3333333333333333703, 0.3333333333333333703, 0.3333333333333333703, 0.3333333333333333703, 0.3333333333333333703, 0.3333333333333333703, 0.3333333333333333703, 0.3333333333333333703, 0.3333333333333333703, 0.3333333333333333703, 0.3333333333333333703, 0.3333333333333333703, 0.3333333333333333703, 0.3333333333333333703, 0.3333333333333333703, 0.3333333333333333703, 0.3333333333333333703, 0.3333333333333333703, 0.3333333333333333703, 0.3333333333333333703, 0.3333333333333333703, 0.3333333333333333703, 0.3333333333333333703, 0.3333333333333333703, 0.3333333333333333703, 0.3333333333333333703, 0.3333333333333333703, 0.3333333333333333703, 0.3333333333333333703, 0.3333333333333333703, 0.3333333333333333703, 0.3333333333333333703, 0.3333333333333333703, 0.3333333333333333703, 0.3333333333333333703, 0.3333333333333333703, 0.3333333333333333703, 0.3333333333333333703, 0.3333333333333333703, 0.3333333333333333703, 0.3333333333333333703, 0.3333333333333333703, 0.3333333333333333703, 0.3333333333333333703),
 ( 0.3333333333333333703, 0.3333333333333333703, 0.3333333333333333703, 0.3333333333333333703, 0.3333333333333333703, 0.3333333333333333703, 0.3333333333333333703, 0.3333333333333333703, 0.3333333333333333703, 0.3333333333333333703, 0.3333333333333333703, 0.3333333333333333703, 0.3333333333333333703, 0.3333333333333333703, 0.3333333333333333703, 0.3333333333333333703, 0.3333333333333333703, 0.3333333333333333703, 0.3333333333333333703, 0.3333333333333333703, 0.3333333333333333703, 0.3333333333333333703, 0.3333333333333333703, 0.3333333333333333703, 0.3333333333333333703, 0.3333333333333333703, 0.3333333333333333703, 0.3333333333333333703, 0.3333333333333333703, 0.3333333333333333703, 0.3333333333333333703, 0.3333333333333333703, 0.3333333333333333703, 0.3333333333333333703, 0.3333333333333333703, 0.3333333333333333703, 0.3333333333333333703, 0.3333333333333333703, 0.3333333333333333703, 0.3333333333333333703, 0.3333333333333333703, 0.3333333333333333703, 0.3333333333333333703, 0.3333333333333333703, 0.3333333333333333703, 0.3333333333333333703, 0.3333333333333333703, 0.3333333333333333703, 0.3333333333333333703, 0.3333333333333333703, 0.3333333333333333703, 0.3333333333333333703, 0.3333333333333333703, 0.3333333333333333703, 0.3333333333333333703, 0.3333333333333333703, 0.3333333333333333703, 0.3333333333333333703, 0.3333333333333333703, 0.3333333333333333703, 0.3333333333333333703, 0.3333333333333333703, 0.3333333333333333703, 0.3333333333333333703, 0.3333333333333333703, 0.3333333333333333703, 0.3333333333333333703, 0.3333333333333333703, 0.3333333333333333703, 0.3333333333333333703, 0.3333333333333333703, 0.3333333333333333703, 0.3333333333333333703, 0.3333333333333333703, 0.3333333333333333703, 0.3333333333333333703, 0.3333333333333333703, 0.3333333333333333703, 0.3333333333333333703, 0.3333333333333333703, 0.3333333333333333703, 0.3333333333333333703, 0.3333333333333333703, 0.3333333333333333703, 0.3333333333333333703, 0.3333333333333333703, 0.3333333333333333703, 0.3333333333333333703, 0.3333333333333333703, 0.3333333333333333703, 0.3333333333333333703, 0.3333333333333333703, 0.3333333333333333703, 0.3333333333333333703, 0.3333333333333333703, 0.3333333333333333703, 0.3333333333333333703, 0.3333333333333333703, 0.3333333333333333703, 0.3333333333333333703, 0.3333333333333333703, 0.3333333333333333703, 0.3333333333333333703, 0.3333333333333333703, 0.3333333333333333703, 0.3333333333333333703, 0.3333333333333333703, 0.3333333333333333703, 0.3333333333333333703, 0.3333333333333333703, 0.3333333333333333703, 0.3333333333333333703, 0.3333333333333333703, 0.3333333333333333703, 0.3333333333333333703, 0.3333333333333333703, 0.3333333333333333703, 0.3333333333333333703, 0.3333333333333333703, 0.3333333333333333703, 0.3333333333333333703, 0.3333333333333333703, 0.3333333333333333703, 0.3333333333333333703, 0.3333333333333333703, 0.3333333333333333703, 0.3333333333333333703, 0.3333333333333333703, 0.3333333333333333703, 0.3333333333333333703, 0.3333333333333333703, 0.3333333333333333703, 0.3333333333333333703, 0.3333333333333333703, 0.3333333333333333703, 0.3333333333333333703, 0.3333333333333333703, 0.3333333333333333703, 0.3333333333333333703, 0.3333333333333333703, 0.3333333333333333703, 0.3333333333333333703, 0.3333333333333333703, 0.3333333333333333703, 0.3333333333333333703, 0.3333333333333333703, 0.3333333333333333703, 0.3333333333333333703, 0.3333333333333333703, 0.3333333333333333703, 0.3333333333333333703, 0.3333333333333333703, 0.3333333333333333703, 0.3333333333333333703, 0.3333333333333333703, 0.3333333333333333703, 0.3333333333333333703, 0.3333333333333333703, 0.3333333333333333703, 0.3333333333333333703, 0.3333333333333333703, 0.3333333333333333703, 0.3333333333333333703, 0.3333333333333333703, 0.3333333333333333703, 0.3333333333333333703, 0.3333333333333333703, 0.3333333333333333703, 0.3333333333333333703, 0.3333333333333333703, 0.3333333333333333703, 0.3333333333333333703, 0.3333333333333333703, 0.3333333333333333703, 0.3333333333333333703, 0.3333333333333333703, 0.3333333333333333703, 0.3333333333333333703, 0.3333333333333333703, 0.3333333333333333703, 0.3333333333333333703, 0.3333333333333333703, 0.3333333333333333703, 0.3333333333333333703, 0.3333333333333333703, 0.3333333333333333703, 0.3333333333333333703, 0.3333333333333333703, 0.3333333333333333703, 0.3333333333333333703, 0.3333333333333333703, 0.3333333333333333703, 0.3333333333333333703, 0.3333333333333333703, 0.3333333333333333703, 0.3333333333333333703, 0.3333333333333333703, 0.3333333333333333703, 0.3333333333333333703, 0.3333333333333333703, 0.3333333333333333703, 0.3333333333333333703, 0.3333333333333333703, 0.3333333333333333703, 0.3333333333333333703, 0.3333333333333333703, 0.3333333333333333703, 0.3333333333333333703, 0.3333333333333333703, 0.3333333333333333703, 0.3333333333333333703, 0.3333333333333333703, 0.3333333333333333703, 0.3333333333333333703, 0.3333333333333333703, 0.3333333333333333703, 0.3333333333333333703, 0.3333333333333333703, 0.3333333333333333703, 0.3333333333333333703, 0.3333333333333333703, 0.3333333333333333703, 0.3333333333333333703, 0.3333333333333333703, 0.3333333333333333703, 0.3333333333333333703, 0.3333333333333333703, 0.3333333333333333703, 0.3333333333333333703, 0.3333333333333333703, 0.3333333333333333703, 0.3333333333333333703, 0.3333333333333333703, 0.3333333333333333703, 0.3333333333333333703, 0.3333333333333333703, 0.3333333333333333703, 0.3333333333333333703, 0.3333333333333333703, 0.3333333333333333703, 0.3333333333333333703, 0.3333333333333333703, 0.3333333333333333703, 0.3333333333333333703, 0.3333333333333333703, 0.3333333333333333703),
 ( 1.000000000000000000, 1.000000000000000000, 1.000000000000000000, 1.000000000000000000, 1.000000000000000000, 1.000000000000000000, 1.000000000000000000, 1.000000000000000000, 1.000000000000000000, 1.000000000000000000, 1.000000000000000000, 1.000000000000000000, 1.000000000000000000, 1.000000000000000000, 1.000000000000000000, 1.000000000000000000, 1.000000000000000000, 1.000000000000000000, 1.000000000000000000, 1.000000000000000000, 1.000000000000000000, 1.000000000000000000, 1.000000000000000000, 1.000000000000000000, 1.000000000000000000, 1.000000000000000000, 1.000000000000000000, 1.000000000000000000, 1.000000000000000000, 1.000000000000000000, 1.000000000000000000, 1.000000000000000000, 1.000000000000000000, 1.000000000000000000, 1.000000000000000000, 1.000000000000000000, 1.000000000000000000, 1.000000000000000000, 1.000000000000000000, 1.000000000000000000, 1.000000000000000000, 1.000000000000000000, 1.000000000000000000, 1.000000000000000000, 1.000000000000000000, 1.000000000000000000, 1.000000000000000000, 1.000000000000000000, 1.000000000000000000, 1.000000000000000000, 1.000000000000000000, 1.000000000000000000, 1.000000000000000000, 1.000000000000000000, 1.000000000000000000, 1.000000000000000000, 1.000000000000000000, 1.000000000000000000, 1.000000000000000000, 1.000000000000000000, 1.000000000000000000, 1.000000000000000000, 1.000000000000000000, 1.000000000000000000, 1.000000000000000000, 1.000000000000000000, 1.000000000000000000, 1.000000000000000000, 1.000000000000000000, 1.000000000000000000, 1.000000000000000000, 1.000000000000000000, 1.000000000000000000, 1.000000000000000000, 1.000000000000000000, 1.000000000000000000, 1.000000000000000000, 1.000000000000000000, 1.000000000000000000, 1.000000000000000000, 1.000000000000000000, 1.000000000000000000, 1.000000000000000000, 1.000000000000000000, 1.000000000000000000, 1.000000000000000000, 1.000000000000000000, 1.000000000000000000, 1.000000000000000000, 1.000000000000000000, 1.000000000000000000, 1.000000000000000000, 1.000000000000000000, 1.000000000000000000, 1.000000000000000000, 1.000000000000000000, 1.000000000000000000, 1.000000000000000000, 1.000000000000000000, 1.000000000000000000, 1.000000000000000000, 1.000000000000000000, 1.000000000000000000, 1.000000000000000000, 1.000000000000000000, 1.000000000000000000, 1.000000000000000000, 1.000000000000000000, 1.000000000000000000, 1.000000000000000000, 1.000000000000000000, 1.000000000000000000, 1.000000000000000000, 1.000000000000000000, 1.000000000000000000, 1.000000000000000000, 1.000000000000000000, 1.000000000000000000, 1.000000000000000000, 1.000000000000000000, 1.000000000000000000, 1.000000000000000000, 1.000000000000000000, 1.000000000000000000, 1.000000000000000000, 1.000000000000000000, 1.000000000000000000, 1.000000000000000000, 1.000000000000000000, 1.000000000000000000, 1.000000000000000000, 1.000000000000000000, 1.000000000000000000, 1.000000000000000000, 1.000000000000000000, 1.000000000000000000, 1.000000000000000000, 1.000000000000000000, 1.000000000000000000, 1.000000000000000000, 1.000000000000000000, 1.000000000000000000, 1.000000000000000000, 1.000000000000000000, 1.000000000000000000, 1.000000000000000000, 1.000000000000000000, 1.000000000000000000, 1.000000000000000000, 1.000000000000000000, 1.000000000000000000, 1.000000000000000000, 1.000000000000000000, 1.000000000000000000, 1.000000000000000000, 1.000000000000000000, 1.000000000000000000, 1.000000000000000000, 1.000000000000000000, 1.000000000000000000, 1.000000000000000000, 1.000000000000000000, 1.000000000000000000, 1.000000000000000000, 1.000000000000000000, 1.000000000000000000, 1.000000000000000000, 1.000000000000000000, 1.000000000000000000, 1.000000000000000000, 1.000000000000000000, 1.000000000000000000, 1.000000000000000000, 1.000000000000000000, 1.000000000000000000, 1.000000000000000000, 1.000000000000000000, 1.000000000000000000, 1.000000000000000000, 1.000000000000000000, 1.000000000000000000, 1.000000000000000000, 1.000000000000000000, 1.000000000000000000, 1.000000000000000000, 1.000000000000000000, 1.000000000000000000, 1.000000000000000000, 1.000000000000000000, 1.000000000000000000, 1.000000000000000000, 1.000000000000000000, 1.000000000000000000, 1.000000000000000000, 1.000000000000000000, 1.000000000000000000, 1.000000000000000000, 1.000000000000000000, 1.000000000000000000, 1.000000000000000000, 1.000000000000000000, 1.000000000000000000, 1.000000000000000000, 1.000000000000000000, 1.000000000000000000, 1.000000000000000000, 1.000000000000000000, 1.000000000000000000, 1.000000000000000000, 1.000000000000000000, 1.000000000000000000, 1.000000000000000000, 1.000000000000000000, 1.000000000000000000, 1.000000000000000000, 1.000000000000000000, 1.000000000000000000, 1.000000000000000000, 1.000000000000000000, 1.000000000000000000, 1.000000000000000000, 1.000000000000000000, 1.000000000000000000, 1.000000000000000000, 1.000000000000000000, 1.000000000000000000, 1.000000000000000000, 1.000000000000000000, 1.000000000000000000, 1.000000000000000000, 1.000000000000000000, 1.000000000000000000, 1.000000000000000000, 1.000000000000000000, 1.000000000000000000, 1.000000000000000000, 1.000000000000000000, 1.000000000000000000, 1.000000000000000000, 1.000000000000000000, 1.000000000000000000, 1.000000000000000000, 1.000000000000000000, 1.000000000000000000, 1.000000000000000000, 1.000000000000000000),
 ( 0.3333333333333333703, 0.3333333333333333703, 0.3333333333333333703, 0.3333333333333333703, 0.3333333333333333703, 0.3333333333333333703, 0.3333333333333333703, 0.3333333333333333703, 0.3333333333333333703, 0.3333333333333333703, 0.3333333333333333703, 0.3333333333333333703, 0.3333333333333333703, 0.3333333333333333703, 0.3333333333333333703, 0.3333333333333333703, 0.3333333333333333703, 0.3333333333333333703, 0.3333333333333333703, 0.3333333333333333703, 0.3333333333333333703, 0.3333333333333333703, 0.3333333333333333703, 0.3333333333333333703, 0.3333333333333333703, 0.3333333333333333703, 0.3333333333333333703, 0.3333333333333333703, 0.3333333333333333703, 0.3333333333333333703, 0.3333333333333333703, 0.3333333333333333703, 0.3333333333333333703, 0.3333333333333333703, 0.3333333333333333703, 0.3333333333333333703, 0.3333333333333333703, 0.3333333333333333703, 0.3333333333333333703, 0.3333333333333333703, 0.3333333333333333703, 0.3333333333333333703, 0.3333333333333333703, 0.3333333333333333703, 0.3333333333333333703, 0.3333333333333333703, 0.3333333333333333703, 0.3333333333333333703, 0.3333333333333333703, 0.3333333333333333703, 0.3333333333333333703, 0.3333333333333333703, 0.3333333333333333703, 0.3333333333333333703, 0.3333333333333333703, 0.3333333333333333703, 0.3333333333333333703, 0.3333333333333333703, 0.3333333333333333703, 0.3333333333333333703, 0.3333333333333333703, 0.3333333333333333703, 0.3333333333333333703, 0.3333333333333333703, 0.3333333333333333703, 0.3333333333333333703, 0.3333333333333333703, 0.3333333333333333703, 0.3333333333333333703, 0.3333333333333333703, 0.3333333333333333703, 0.3333333333333333703, 0.3333333333333333703, 0.3333333333333333703, 0.3333333333333333703, 0.3333333333333333703, 0.3333333333333333703, 0.3333333333333333703, 0.3333333333333333703, 0.3333333333333333703, 0.3333333333333333703, 0.3333333333333333703, 0.3333333333333333703, 0.3333333333333333703, 0.3333333333333333703, 0.3333333333333333703, 0.3333333333333333703, 0.3333333333333333703, 0.3333333333333333703, 0.3333333333333333703, 0.3333333333333333703, 0.3333333333333333703, 0.3333333333333333703, 0.3333333333333333703, 0.3333333333333333703, 0.3333333333333333703, 0.3333333333333333703, 0.3333333333333333703, 0.3333333333333333703, 0.3333333333333333703, 0.3333333333333333703, 0.3333333333333333703, 0.3333333333333333703, 0.3333333333333333703, 0.3333333333333333703, 0.3333333333333333703, 0.3333333333333333703, 0.3333333333333333703, 0.3333333333333333703, 0.3333333333333333703, 0.3333333333333333703, 0.3333333333333333703, 0.3333333333333333703, 0.3333333333333333703, 0.3333333333333333703, 0.3333333333333333703, 0.3333333333333333703, 0.3333333333333333703, 0.3333333333333333703, 0.3333333333333333703, 0.3333333333333333703, 0.3333333333333333703, 0.3333333333333333703, 0.3333333333333333703, 0.3333333333333333703, 0.3333333333333333703, 0.3333333333333333703, 0.3333333333333333703, 0.3333333333333333703, 0.3333333333333333703, 0.3333333333333333703, 0.3333333333333333703, 0.3333333333333333703, 0.3333333333333333703, 0.3333333333333333703, 0.3333333333333333703, 0.3333333333333333703, 0.3333333333333333703, 0.3333333333333333703, 0.3333333333333333703, 0.3333333333333333703, 0.3333333333333333703, 0.3333333333333333703, 0.3333333333333333703, 0.3333333333333333703, 0.3333333333333333703, 0.3333333333333333703, 0.3333333333333333703, 0.3333333333333333703, 0.3333333333333333703, 0.3333333333333333703, 0.3333333333333333703, 0.3333333333333333703, 0.3333333333333333703, 0.3333333333333333703, 0.3333333333333333703, 0.3333333333333333703, 0.3333333333333333703, 0.3333333333333333703, 0.3333333333333333703, 0.3333333333333333703, 0.3333333333333333703, 0.3333333333333333703, 0.3333333333333333703, 0.3333333333333333703, 0.3333333333333333703, 0.3333333333333333703, 0.3333333333333333703, 0.3333333333333333703, 0.3333333333333333703, 0.3333333333333333703, 0.3333333333333333703, 0.3333333333333333703, 0.3333333333333333703, 0.3333333333333333703, 0.3333333333333333703, 0.3333333333333333703, 0.3333333333333333703, 0.3333333333333333703, 0.3333333333333333703, 0.3333333333333333703, 0.3333333333333333703, 0.3333333333333333703, 0.3333333333333333703, 0.3333333333333333703, 0.3333333333333333703, 0.3333333333333333703, 0.3333333333333333703, 0.3333333333333333703, 0.3333333333333333703, 0.3333333333333333703, 0.3333333333333333703, 0.3333333333333333703, 0.3333333333333333703, 0.3333333333333333703, 0.3333333333333333703, 0.3333333333333333703, 0.3333333333333333703, 0.3333333333333333703, 0.3333333333333333703, 0.3333333333333333703, 0.3333333333333333703, 0.3333333333333333703, 0.3333333333333333703, 0.3333333333333333703, 0.3333333333333333703, 0.3333333333333333703, 0.3333333333333333703, 0.3333333333333333703, 0.3333333333333333703, 0.3333333333333333703, 0.3333333333333333703, 0.3333333333333333703, 0.3333333333333333703, 0.3333333333333333703, 0.3333333333333333703, 0.3333333333333333703, 0.3333333333333333703, 0.3333333333333333703, 0.3333333333333333703, 0.3333333333333333703, 0.3333333333333333703, 0.3333333333333333703, 0.3333333333333333703, 0.3333333333333333703, 0.3333333333333333703, 0.3333333333333333703, 0.3333333333333333703, 0.3333333333333333703, 0.3333333333333333703, 0.3333333333333333703, 0.3333333333333333703, 0.3333333333333333703, 0.3333333333333333703, 0.3333333333333333703, 0.3333333333333333703, 0.3333333333333333703, 0.3333333333333333703, 0.3333333333333333703, 0.3333333333333333703, 0.3333333333333333703, 0.3333333333333333703, 0.3333333333333333703, 0.3333333333333333703, 0.3333333333333333703, 0.3333333333333333703),
 ( 0.3333333333333333703, 0.3333333333333333703, 0.3333333333333333703, 0.3333333333333333703, 0.3333333333333333703, 0.3333333333333333703, 0.3333333333333333703, 0.3333333333333333703, 0.3333333333333333703, 0.3333333333333333703, 0.3333333333333333703, 0.3333333333333333703, 0.3333333333333333703, 0.3333333333333333703, 0.3333333333333333703, 0.3333333333333333703, 0.3333333333333333703, 0.3333333333333333703, 0.3333333333333333703, 0.3333333333333333703, 0.3333333333333333703, 0.3333333333333333703, 0.3333333333333333703, 0.3333333333333333703, 0.3333333333333333703, 0.3333333333333333703, 0.3333333333333333703, 0.3333333333333333703, 0.3333333333333333703, 0.3333333333333333703, 0.3333333333333333703, 0.3333333333333333703, 0.3333333333333333703, 0.3333333333333333703, 0.3333333333333333703, 0.3333333333333333703, 0.3333333333333333703, 0.3333333333333333703, 0.3333333333333333703, 0.3333333333333333703, 0.3333333333333333703, 0.3333333333333333703, 0.3333333333333333703, 0.3333333333333333703, 0.3333333333333333703, 0.3333333333333333703, 0.3333333333333333703, 0.3333333333333333703, 0.3333333333333333703, 0.3333333333333333703, 0.3333333333333333703, 0.3333333333333333703, 0.3333333333333333703, 0.3333333333333333703, 0.3333333333333333703, 0.3333333333333333703, 0.3333333333333333703, 0.3333333333333333703, 0.3333333333333333703, 0.3333333333333333703, 0.3333333333333333703, 0.3333333333333333703, 0.3333333333333333703, 0.3333333333333333703, 0.3333333333333333703, 0.3333333333333333703, 0.3333333333333333703, 0.3333333333333333703, 0.3333333333333333703, 0.3333333333333333703, 0.3333333333333333703, 0.3333333333333333703, 0.3333333333333333703, 0.3333333333333333703, 0.3333333333333333703, 0.3333333333333333703, 0.3333333333333333703, 0.3333333333333333703, 0.3333333333333333703, 0.3333333333333333703, 0.3333333333333333703, 0.3333333333333333703, 0.3333333333333333703, 0.3333333333333333703, 0.3333333333333333703, 0.3333333333333333703, 0.3333333333333333703, 0.3333333333333333703, 0.3333333333333333703, 0.3333333333333333703, 0.3333333333333333703, 0.3333333333333333703, 0.3333333333333333703, 0.3333333333333333703, 0.3333333333333333703, 0.3333333333333333703, 0.3333333333333333703, 0.3333333333333333703, 0.3333333333333333703, 0.3333333333333333703, 0.3333333333333333703, 0.3333333333333333703, 0.3333333333333333703, 0.3333333333333333703, 0.3333333333333333703, 0.3333333333333333703, 0.3333333333333333703, 0.3333333333333333703, 0.3333333333333333703, 0.3333333333333333703, 0.3333333333333333703, 0.3333333333333333703, 0.3333333333333333703, 0.3333333333333333703, 0.3333333333333333703, 0.3333333333333333703, 0.3333333333333333703, 0.3333333333333333703, 0.3333333333333333703, 0.3333333333333333703, 0.3333333333333333703, 0.3333333333333333703, 0.3333333333333333703, 0.3333333333333333703, 0.3333333333333333703, 0.3333333333333333703, 0.3333333333333333703, 0.3333333333333333703, 0.3333333333333333703, 0.3333333333333333703, 0.3333333333333333703, 0.3333333333333333703, 0.3333333333333333703, 0.3333333333333333703, 0.3333333333333333703, 0.3333333333333333703, 0.3333333333333333703, 0.3333333333333333703, 0.3333333333333333703, 0.3333333333333333703, 0.3333333333333333703, 0.3333333333333333703, 0.3333333333333333703, 0.3333333333333333703, 0.3333333333333333703, 0.3333333333333333703, 0.3333333333333333703, 0.3333333333333333703, 0.3333333333333333703, 0.3333333333333333703, 0.3333333333333333703, 0.3333333333333333703, 0.3333333333333333703, 0.3333333333333333703, 0.3333333333333333703, 0.3333333333333333703, 0.3333333333333333703, 0.3333333333333333703, 0.3333333333333333703, 0.3333333333333333703, 0.3333333333333333703, 0.3333333333333333703, 0.3333333333333333703, 0.3333333333333333703, 0.3333333333333333703, 0.3333333333333333703, 0.3333333333333333703, 0.3333333333333333703, 0.3333333333333333703, 0.3333333333333333703, 0.3333333333333333703, 0.3333333333333333703, 0.3333333333333333703, 0.3333333333333333703, 0.3333333333333333703, 0.3333333333333333703, 0.3333333333333333703, 0.3333333333333333703, 0.3333333333333333703, 0.3333333333333333703, 0.3333333333333333703, 0.3333333333333333703, 0.3333333333333333703, 0.3333333333333333703, 0.3333333333333333703, 0.3333333333333333703, 0.3333333333333333703, 0.3333333333333333703, 0.3333333333333333703, 0.3333333333333333703, 0.3333333333333333703, 0.3333333333333333703, 0.3333333333333333703, 0.3333333333333333703, 0.3333333333333333703, 0.3333333333333333703, 0.3333333333333333703, 0.3333333333333333703, 0.3333333333333333703, 0.3333333333333333703, 0.3333333333333333703, 0.3333333333333333703, 0.3333333333333333703, 0.3333333333333333703, 0.3333333333333333703, 0.3333333333333333703, 0.3333333333333333703, 0.3333333333333333703, 0.3333333333333333703, 0.3333333333333333703, 0.3333333333333333703, 0.3333333333333333703, 0.3333333333333333703, 0.3333333333333333703, 0.3333333333333333703, 0.3333333333333333703, 0.3333333333333333703, 0.3333333333333333703, 0.3333333333333333703, 0.3333333333333333703, 0.3333333333333333703, 0.3333333333333333703, 0.3333333333333333703, 0.3333333333333333703, 0.3333333333333333703, 0.3333333333333333703, 0.3333333333333333703, 0.3333333333333333703, 0.3333333333333333703, 0.3333333333333333703, 0.3333333333333333703, 0.3333333333333333703, 0.3333333333333333703, 0.3333333333333333703, 0.3333333333333333703, 0.3333333333333333703, 0.3333333333333333703, 0.3333333333333333703, 0.3333333333333333703, 0.3333333333333333703, 0.3333333333333333703, 0.3333333333333333703, 0.3333333333333333703, 0.3333333333333333703, 0.3333333333333333703, 0.3333333333333333703),
 ( 1.000000000000000000, 1.000000000000000000, 1.000000000000000000, 1.000000000000000000, 1.000000000000000000, 1.000000000000000000, 1.000000000000000000, 1.000000000000000000, 1.000000000000000000, 1.000000000000000000, 1.000000000000000000, 1.000000000000000000, 1.000000000000000000, 1.000000000000000000, 1.000000000000000000, 1.000000000000000000, 1.000000000000000000, 1.000000000000000000, 1.000000000000000000, 1.000000000000000000, 1.000000000000000000, 1.000000000000000000, 1.000000000000000000, 1.000000000000000000, 1.000000000000000000, 1.000000000000000000, 1.000000000000000000, 1.000000000000000000, 1.000000000000000000, 1.000000000000000000, 1.000000000000000000, 1.000000000000000000, 1.000000000000000000, 1.000000000000000000, 1.000000000000000000, 1.000000000000000000, 1.000000000000000000, 1.000000000000000000, 1.000000000000000000, 1.000000000000000000, 1.000000000000000000, 1.000000000000000000, 1.000000000000000000, 1.000000000000000000, 1.000000000000000000, 1.000000000000000000, 1.000000000000000000, 1.000000000000000000, 1.000000000000000000, 1.000000000000000000, 1.000000000000000000, 1.000000000000000000, 1.000000000000000000, 1.000000000000000000, 1.000000000000000000, 1.000000000000000000, 1.000000000000000000, 1.000000000000000000, 1.000000000000000000, 1.000000000000000000, 1.000000000000000000, 1.000000000000000000, 1.000000000000000000, 1.000000000000000000, 1.000000000000000000, 1.000000000000000000, 1.000000000000000000, 1.000000000000000000, 1.000000000000000000, 1.000000000000000000, 1.000000000000000000, 1.000000000000000000, 1.000000000000000000, 1.000000000000000000, 1.000000000000000000, 1.000000000000000000, 1.000000000000000000, 1.000000000000000000, 1.000000000000000000, 1.000000000000000000, 1.000000000000000000, 1.000000000000000000, 1.000000000000000000, 1.000000000000000000, 1.000000000000000000, 1.000000000000000000, 1.000000000000000000, 1.000000000000000000, 1.000000000000000000, 1.000000000000000000, 1.000000000000000000, 1.000000000000000000, 1.000000000000000000, 1.000000000000000000, 1.000000000000000000, 1.000000000000000000, 1.000000000000000000, 1.000000000000000000, 1.000000000000000000, 1.000000000000000000, 1.000000000000000000, 1.000000000000000000, 1.000000000000000000, 1.000000000000000000, 1.000000000000000000, 1.000000000000000000, 1.000000000000000000, 1.000000000000000000, 1.000000000000000000, 1.000000000000000000, 1.000000000000000000, 1.000000000000000000, 1.000000000000000000, 1.000000000000000000, 1.000000000000000000, 1.000000000000000000, 1.000000000000000000, 1.000000000000000000, 1.000000000000000000, 1.000000000000000000, 1.000000000000000000, 1.000000000000000000, 1.000000000000000000, 1.000000000000000000, 1.000000000000000000, 1.000000000000000000, 1.000000000000000000, 1.000000000000000000, 1.000000000000000000, 1.000000000000000000, 1.000000000000000000, 1.000000000000000000, 1.000000000000000000, 1.000000000000000000, 1.000000000000000000, 1.000000000000000000, 1.000000000000000000, 1.000000000000000000, 1.000000000000000000, 1.000000000000000000, 1.000000000000000000, 1.000000000000000000, 1.000000000000000000, 1.000000000000000000, 1.000000000000000000, 1.000000000000000000, 1.000000000000000000, 1.000000000000000000, 1.000000000000000000, 1.000000000000000000, 1.000000000000000000, 1.000000000000000000, 1.000000000000000000, 1.000000000000000000, 1.000000000000000000, 1.000000000000000000, 1.000000000000000000, 1.000000000000000000, 1.000000000000000000, 1.000000000000000000, 1.000000000000000000, 1.000000000000000000, 1.000000000000000000, 1.000000000000000000, 1.000000000000000000, 1.000000000000000000, 1.000000000000000000, 1.000000000000000000, 1.000000000000000000, 1.000000000000000000, 1.000000000000000000, 1.000000000000000000, 1.000000000000000000, 1.000000000000000000, 1.000000000000000000, 1.000000000000000000, 1.000000000000000000, 1.000000000000000000, 1.000000000000000000, 1.000000000000000000, 1.000000000000000000, 1.000000000000000000, 1.000000000000000000, 1.000000000000000000, 1.000000000000000000, 1.000000000000000000, 1.000000000000000000, 1.000000000000000000, 1.000000000000000000, 1.000000000000000000, 1.000000000000000000, 1.000000000000000000, 1.000000000000000000, 1.000000000000000000, 1.000000000000000000, 1.000000000000000000, 1.000000000000000000, 1.000000000000000000, 1.000000000000000000, 1.000000000000000000, 1.000000000000000000, 1.000000000000000000, 1.000000000000000000, 1.000000000000000000, 1.000000000000000000, 1.000000000000000000, 1.000000000000000000, 1.000000000000000000, 1.000000000000000000, 1.000000000000000000, 1.000000000000000000, 1.000000000000000000, 1.000000000000000000, 1.000000000000000000, 1.000000000000000000, 1.000000000000000000, 1.000000000000000000, 1.000000000000000000, 1.000000000000000000, 1.000000000000000000, 1.000000000000000000, 1.000000000000000000, 1.000000000000000000, 1.000000000000000000, 1.000000000000000000, 1.000000000000000000, 1.000000000000000000, 1.000000000000000000, 1.000000000000000000, 1.000000000000000000, 1.000000000000000000, 1.000000000000000000, 1.000000000000000000, 1.000000000000000000, 1.000000000000000000, 1.000000000000000000, 1.000000000000000000, 1.000000000000000000, 1.000000000000000000, 1.000000000000000000, 1.000000000000000000, 1.000000000000000000, 1.000000000000000000, 1.000000000000000000, 1.000000000000000000, 1.000000000000000000) ) ) 
 REPRESENTATION_ITEM ( '' )  SURFACE ( )  );
#21947 = LINE ( 'NONE', #12928, #26465 ) ;
#21948 = VECTOR ( 'NONE', #27937, 1000.000000000000000 ) ;
#21949 = ORIENTED_EDGE ( 'NONE', *, *, #12144, .T. ) ;
#21950 = DIRECTION ( 'NONE',  ( 0.5877852522924731371, 1.586114251531760728E-16, 0.8090169943749474513 ) ) ;
#21951 = CARTESIAN_POINT ( 'NONE',  ( 168.6922820468853956, -1.999999999999970024, -32.39392330124607611 ) ) ;
#21952 = PLANE ( 'NONE',  #30247 ) ;
#21953 = ORIENTED_EDGE ( 'NONE', *, *, #19276, .T. ) ;
#21954 = CARTESIAN_POINT ( 'NONE',  ( 134.7287565553230024, -1.999999999999980460, -16.50000000000000000 ) ) ;
#21955 = DIRECTION ( 'NONE',  ( 0.5840962589317576503, -0.8116843969807016057, 0.000000000000000000 ) ) ;
#21956 = AXIS2_PLACEMENT_3D ( 'NONE', #8933, #13232, #18104 ) ;
#21957 = CARTESIAN_POINT ( 'NONE',  ( 12.26413032053702779, 8.815164712426300397, -16.54932944099246228 ) ) ;
#21958 = EDGE_CURVE ( 'NONE', #25168, #10075, #18753, .T. ) ;
#21959 = CARTESIAN_POINT ( 'NONE',  ( 33.26400919001463308, -11.80307911188568148, -18.11217348381727632 ) ) ;
#21960 = ORIENTED_EDGE ( 'NONE', *, *, #4160, .T. ) ;
#21961 = VECTOR ( 'NONE', #27606, 1000.000000000000000 ) ;
#21962 = CARTESIAN_POINT ( 'NONE',  ( 9.116630548627156827, 16.16256849206635238, -17.05302909012592494 ) ) ;
#21963 = CARTESIAN_POINT ( 'NONE',  ( 27.51942754507220812, -5.605608590038333006, -14.64806962472005658 ) ) ;
#21964 = CARTESIAN_POINT ( 'NONE',  ( 12.79981923948071554, 9.689364640521217709, -16.15445150739013158 ) ) ;
#21965 = FACE_BOUND ( 'NONE', #9818, .T. ) ;
#21966 = EDGE_LOOP ( 'NONE', ( #641, #21929, #27106, #18652 ) ) ;
#21967 = ORIENTED_EDGE ( 'NONE', *, *, #1373, .F. ) ;
#21968 = ORIENTED_EDGE ( 'NONE', *, *, #4631, .T. ) ;
#21969 = DIRECTION ( 'NONE',  ( 0.000000000000000000, 0.000000000000000000, -1.000000000000000000 ) ) ;
#21970 = CARTESIAN_POINT ( 'NONE',  ( 11.48043977940431226, 9.236673419044803879, -15.85762597608872326 ) ) ;
#21971 = CARTESIAN_POINT ( 'NONE',  ( 111.5443916382889569, -4.999999999999986677, -81.04174428570250655 ) ) ;
#21972 = ORIENTED_EDGE ( 'NONE', *, *, #9203, .T. ) ;
#21973 = LINE ( 'NONE', #3080, #13015 ) ;
#21974 = EDGE_LOOP ( 'NONE', ( #22265, #16066, #1028, #17227, #21221 ) ) ;
#21975 = EDGE_CURVE ( 'NONE', #21788, #2498, #7014, .T. ) ;
#21976 = CARTESIAN_POINT ( 'NONE',  ( 12.50603416232391929, 8.608717614871036261, -16.38042650914619358 ) ) ;
#21977 = ORIENTED_EDGE ( 'NONE', *, *, #5599, .T. ) ;
#21978 = CARTESIAN_POINT ( 'NONE',  ( 19.05076746314986025, 7.350425291474770084, -20.38782652337943446 ) ) ;
#21979 = CARTESIAN_POINT ( 'NONE',  ( 25.79824969357368047, -12.24460132778619226, -15.92960863319586906 ) ) ;
#21980 = CARTESIAN_POINT ( 'NONE',  ( 2.500000000000000444, -2.357898499370430834, 3.469446951953614189E-15 ) ) ;
#21981 = VERTEX_POINT ( 'NONE', #6719 ) ;
#21982 = CARTESIAN_POINT ( 'NONE',  ( 420.0000000000002274, 34.64101615137744972, 10.00000000000000178 ) ) ;
#21983 = VECTOR ( 'NONE', #19326, 1000.000000000000000 ) ;
#21984 = APPLICATION_PROTOCOL_DEFINITION ( 'draft international standard', 'automotive_design', 1998, #2103 ) ;
#21985 = ORIENTED_EDGE ( 'NONE', *, *, #13137, .T. ) ;
#21986 = CARTESIAN_POINT ( 'NONE',  ( 18.78845540754137744, 2.550960650414936914, -18.75190108346638951 ) ) ;
#21987 = AXIS2_PLACEMENT_3D ( 'NONE', #216, #16533, #11641 ) ;
#21988 = CARTESIAN_POINT ( 'NONE',  ( 15.46244301724551740, 3.702889819443702990, -17.82701508041758842 ) ) ;
#21989 = LINE ( 'NONE', #5817, #7123 ) ;
#21990 = FACE_BOUND ( 'NONE', #7244, .T. ) ;
#21991 =( GEOMETRIC_REPRESENTATION_CONTEXT ( 3 ) GLOBAL_UNCERTAINTY_ASSIGNED_CONTEXT ( ( #22945 ) ) GLOBAL_UNIT_ASSIGNED_CONTEXT ( ( #3412, #23878, #976 ) ) REPRESENTATION_CONTEXT ( 'NONE', 'WORKASPACE' ) );
#21992 = MANIFOLD_SOLID_BREP ( 'Fill Pattern1', #21886 ) ;
#21993 = ORIENTED_EDGE ( 'NONE', *, *, #22492, .F. ) ;
#21994 = ADVANCED_FACE ( 'NONE', ( #9128 ), #25623, .T. ) ;
#21995 = DIRECTION ( 'NONE',  ( -0.8090169943749474513, -2.183098979609982436E-16, -0.5877852522924731371 ) ) ;
#21996 = LINE ( 'NONE', #2790, #7213 ) ;
#21997 = CARTESIAN_POINT ( 'NONE',  ( 161.1922820468853388, -1.999999999999973577, -10.74328820663507678 ) ) ;
#21998 = PRODUCT_RELATED_PRODUCT_CATEGORY ( 'part', '', ( #20070 ) ) ;
#21999 = CARTESIAN_POINT ( 'NONE',  ( 158.6922820468853672, -1.999999999999973577, -15.07341522555727664 ) ) ;
#22000 = CARTESIAN_POINT ( 'NONE',  ( 11.36920530384750805, 13.65748684056475426, -15.68605758175906040 ) ) ;
#22002 = AXIS2_PLACEMENT_3D ( 'NONE', #24339, #9981, #21741 ) ;
#22001 = FACE_OUTER_BOUND ( 'NONE', #19469, .T. ) ;
#22003 = ORIENTED_EDGE ( 'NONE', *, *, #11861, .F. ) ;
#22004 = LINE ( 'NONE', #5379, #10497 ) ;
#22005 = ORIENTED_EDGE ( 'NONE', *, *, #11570, .T. ) ;
#22006 = CONICAL_SURFACE ( 'NONE', #19086, 2.055000000000000160, 0.7853981633974721488 ) ;
#22007 = CARTESIAN_POINT ( 'NONE',  ( 12.50016782010997751, 8.570776461014483871, -15.13004124836345632 ) ) ;
#22008 = VERTEX_POINT ( 'NONE', #4573 ) ;
#22009 = CARTESIAN_POINT ( 'NONE',  ( 10.67335300198236148, 9.023663108408856104, -16.40923739229002010 ) ) ;
#22010 = DIRECTION ( 'NONE',  ( -0.06678507476159963041, 0.9947851038922184141, -0.07708664516786083165 ) ) ;
#22011 = CARTESIAN_POINT ( 'NONE',  ( -6.499999999999928946, -11.25833024919774417, -18.00000000000000000 ) ) ;
#22012 = PLANE ( 'NONE',  #20479 ) ;
#22013 = CARTESIAN_POINT ( 'NONE',  ( -24.00000000000017053, 34.64101615137744972, 0.000000000000000000 ) ) ;
#22014 = ORIENTED_EDGE ( 'NONE', *, *, #5600, .F. ) ;
#22015 = CARTESIAN_POINT ( 'NONE',  ( 12.86479781618563045, 9.514843269526567227, -16.11816302316177030 ) ) ;
#22016 = CARTESIAN_POINT ( 'NONE',  ( 34.66364242521329686, -12.71642730124038501, -18.97786663347613256 ) ) ;
#22017 = CARTESIAN_POINT ( 'NONE',  ( 18.88762249820254624, 5.002188274287570735, -13.90571046850145542 ) ) ;
#22018 = ORIENTED_EDGE ( 'NONE', *, *, #25411, .F. ) ;
#22019 = PRODUCT ( 'base plate', 'base plate', '', ( #3232 ) ) ;
#22020 = DIRECTION ( 'NONE',  ( -0.5877852522924731371, -1.586114251531760728E-16, -0.8090169943749474513 ) ) ;
#22021 = CARTESIAN_POINT ( 'NONE',  ( 14.73435313093308174, 9.569269045654692718, -13.91804818168885305 ) ) ;
#22022 = DIRECTION ( 'NONE',  ( -0.5877852522924731371, -1.586114251531760728E-16, -0.8090169943749474513 ) ) ;
#22023 = LINE ( 'NONE', #8124, #4491 ) ;
#22024 =( LENGTH_UNIT ( ) NAMED_UNIT ( * ) SI_UNIT ( .MILLI., .METRE. ) );
#22025 = CARTESIAN_POINT ( 'NONE',  ( 24.38930386813997586, -0.5518329404549096040, -18.38842912410832753 ) ) ;
#22026 = CARTESIAN_POINT ( 'NONE',  ( 22.65897993816424716, 3.718266075228530365, -15.21131701836175232 ) ) ;
#22027 = ORIENTED_EDGE ( 'NONE', *, *, #21002, .F. ) ;
#22028 = EDGE_LOOP ( 'NONE', ( #27636, #25716, #11446, #28243 ) ) ;
#22029 = CYLINDRICAL_SURFACE ( 'NONE', #24974, 9.000000000000007105 ) ;
#22030 = LINE ( 'NONE', #20179, #4547 ) ;
#22031 = EDGE_CURVE ( 'NONE', #5352, #16324, #27657, .T. ) ;
#22032 = EDGE_CURVE ( 'NONE', #25023, #5352, #25481, .T. ) ;
#22033 = CARTESIAN_POINT ( 'NONE',  ( 158.6922820468853104, -1.999999999999974909, -0.6060766987539614181 ) ) ;
#22034 = DIRECTION ( 'NONE',  ( 0.000000000000000000, 0.000000000000000000, 1.000000000000000000 ) ) ;
#22035 = ADVANCED_FACE ( 'NONE', ( #11725 ), #19804, .T. ) ;
#22036 = CARTESIAN_POINT ( 'NONE',  ( 143.6922820468854525, -10.00000000000000355, -15.07341522555727664 ) ) ;
#22037 = ORIENTED_EDGE ( 'NONE', *, *, #10994, .F. ) ;
#22038 = CARTESIAN_POINT ( 'NONE',  ( 11.48043977940431226, 9.236673419044803879, -15.85762597608872326 ) ) ;
#22039 = CARTESIAN_POINT ( 'NONE',  ( 15.93484470893836935, 6.939319753835953009, -14.67888072223970752 ) ) ;
#22040 = CARTESIAN_POINT ( 'NONE',  ( 22.68884594494833706, -6.762261587817247843, -18.56982216542981234 ) ) ;
#22041 = ORIENTED_EDGE ( 'NONE', *, *, #21938, .F. ) ;
#22042 = FACE_OUTER_BOUND ( 'NONE', #24012, .T. ) ;
#22043 = DIRECTION ( 'NONE',  ( -0.5877852522924731371, -1.586114251531760235E-16, 0.8090169943749474513 ) ) ;
#22044 = DIRECTION ( 'NONE',  ( -0.9510565162951536422, 0.000000000000000000, -0.3090169943749472292 ) ) ;
#22045 = CARTESIAN_POINT ( 'NONE',  ( 427.0000000000002274, 34.64101615137744972, 12.00000000000000178 ) ) ;
#22046 = VECTOR ( 'NONE', #6770, 1000.000000000000000 ) ;
#22047 = AXIS2_PLACEMENT_3D ( 'NONE', #11012, #20470, #25364 ) ;
#22048 = LINE ( 'NONE', #5573, #21013 ) ;
#22049 = DIRECTION ( 'NONE',  ( 0.5877852522924731371, 1.586114251531760728E-16, 0.8090169943749474513 ) ) ;
#22051 = VERTEX_POINT ( 'NONE', #16162 ) ;
#22050 = CARTESIAN_POINT ( 'NONE',  ( 21.58242789233717573, 5.264303332692052528, -18.32037006577847293 ) ) ;
#22052 = VERTEX_POINT ( 'NONE', #25337 ) ;
#22053 = LINE ( 'NONE', #26808, #24686 ) ;
#22054 = CARTESIAN_POINT ( 'NONE',  ( 12.27664511671607883, 9.495749246718952818, -15.31080714918738295 ) ) ;
#22055 = DIRECTION ( 'NONE',  ( -0.8090169943749474513, -2.183098979609982436E-16, 0.5877852522924731371 ) ) ;
#22056 = CARTESIAN_POINT ( 'NONE',  ( 143.6922820468854525, -10.00000000000000355, -26.58683881228715506 ) ) ;
#22057 = CARTESIAN_POINT ( 'NONE',  ( 23.66272512268759343, 2.894330346666426745, -16.12005855839824520 ) ) ;
#22058 = CARTESIAN_POINT ( 'NONE',  ( 137.0152310637605808, -1.999999999999979572, -34.70218595412750773 ) ) ;
#22059 = CARTESIAN_POINT ( 'NONE',  ( 19.52525132842032107, 6.402381508982842639, -20.74126646842140431 ) ) ;
#22060 = VERTEX_POINT ( 'NONE', #11874 ) ;
#22061 = DIRECTION ( 'NONE',  ( 0.3090169943749472292, 8.338696094057992503E-17, -0.9510565162951536422 ) ) ;
#22062 = CARTESIAN_POINT ( 'NONE',  ( 31.07149168920019733, -7.992644923617350905, -17.88177209202816087 ) ) ;
#22063 = VECTOR ( 'NONE', #8392, 1000.000000000000000 ) ;
#22064 = CARTESIAN_POINT ( 'NONE',  ( 25.07021298685211619, 1.093672866225363638, -16.25732641482299812 ) ) ;
#22065 = ORIENTED_EDGE ( 'NONE', *, *, #6571, .T. ) ;
#22066 = CARTESIAN_POINT ( 'NONE',  ( 27.89048517759004753, -11.43816616845083445, -12.79876095355805177 ) ) ;
#22067 = EDGE_LOOP ( 'NONE', ( #8247, #27775, #3486, #2614 ) ) ;
#22068 = AXIS2_PLACEMENT_3D ( 'NONE', #12177, #9578, #16302 ) ;
#22069 = CARTESIAN_POINT ( 'NONE',  ( -19.99999999999998934, 55.00000000000000711, 29.99999999999999289 ) ) ;
#22070 = EDGE_CURVE ( 'NONE', #14866, #25730, #28259, .T. ) ;
#22071 = ORIENTED_EDGE ( 'NONE', *, *, #18422, .F. ) ;
#22072 = DIRECTION ( 'NONE',  ( 1.000000000000000000, -1.840388255087189623E-16, 0.000000000000000000 ) ) ;
#22073 = CARTESIAN_POINT ( 'NONE',  ( 3.999999999999998224, 2.309401076758477167, -2.450000000000000178 ) ) ;
#22074 = EDGE_CURVE ( 'NONE', #17531, #12785, #9428, .T. ) ;
#22075 = CARTESIAN_POINT ( 'NONE',  ( 162.0152310637604387, -1.999999999999973133, -8.721423840594312082 ) ) ;
#22076 = EDGE_CURVE ( 'NONE', #2523, #13085, #12026, .T. ) ;
#22077 = CARTESIAN_POINT ( 'NONE',  ( 17.83091951040035283, 10.74857467630938501, -15.40187535130914753 ) ) ;
#22078 = CARTESIAN_POINT ( 'NONE',  ( 33.42826320546385688, -10.41623213582910523, -18.33855703361424361 ) ) ;
#22079 = CARTESIAN_POINT ( 'NONE',  ( 9.915248083523094280, 16.41276333319327918, -16.50506225043874409 ) ) ;
#22080 = FACE_OUTER_BOUND ( 'NONE', #11590, .T. ) ;
#22081 = LINE ( 'NONE', #17785, #1769 ) ;
#22082 = CARTESIAN_POINT ( 'NONE',  ( 9.661883061612440926, 16.25482663361732705, -17.94384837343789130 ) ) ;
#22083 = FACE_OUTER_BOUND ( 'NONE', #13116, .T. ) ;
#22084 = DIRECTION ( 'NONE',  ( -1.000000000000000000, -2.908569913943825554E-16, 0.000000000000000000 ) ) ;
#22085 = VERTEX_POINT ( 'NONE', #13721 ) ;
#22086 = DIRECTION ( 'NONE',  ( 0.9510565162951535312, 2.566386769018988816E-16, -0.3090169943749475623 ) ) ;
#22087 = DIRECTION ( 'NONE',  ( -0.5877852522924731371, -1.586114251531760728E-16, -0.8090169943749474513 ) ) ;
#22088 = DIRECTION ( 'NONE',  ( 1.000000000000000000, 0.000000000000000000, 0.000000000000000000 ) ) ;
#22090 = VERTEX_POINT ( 'NONE', #20730 ) ;
#22089 = CIRCLE ( 'NONE', #8911, 1.500000000000001332 ) ;
#22091 = ORIENTED_EDGE ( 'NONE', *, *, #12802, .F. ) ;
#22092 = CARTESIAN_POINT ( 'NONE',  ( 13.36610298980765776, 7.620062051554192806, -15.71863358442526781 ) ) ;
#22093 = CARTESIAN_POINT ( 'NONE',  ( 14.69524703049083492, 10.61837011038446654, -14.15659040230468690 ) ) ;
#22094 = CARTESIAN_POINT ( 'NONE',  ( 28.02603357813017482, -6.678172375388682802, -19.11289830413424440 ) ) ;
#22095 = CARTESIAN_POINT ( 'NONE',  ( 144.5152310637606092, -4.999999999999978684, -28.60870317832789311 ) ) ;
#22096 = DIRECTION ( 'NONE',  ( 0.000000000000000000, 0.000000000000000000, 1.000000000000000000 ) ) ;
#22097 = DIRECTION ( 'NONE',  ( 0.000000000000000000, 0.000000000000000000, -1.000000000000000000 ) ) ;
#22098 = VECTOR ( 'NONE', #25313, 1000.000000000000000 ) ;
#22099 = ORIENTED_EDGE ( 'NONE', *, *, #19542, .F. ) ;
#22100 = FACE_OUTER_BOUND ( 'NONE', #4073, .T. ) ;
#22101 = CARTESIAN_POINT ( 'NONE',  ( 166.1922820468853672, -9.999999999999996447, -30.91696583120936026 ) ) ;
#22102 = VERTEX_POINT ( 'NONE', #23184 ) ;
#22103 = EDGE_CURVE ( 'NONE', #15438, #952, #1809, .T. ) ;
#22104 = CARTESIAN_POINT ( 'NONE',  ( 137.2287565553230309, -4.999999999999980460, -12.16987298107779303 ) ) ;
#22105 = PLANE ( 'NONE',  #9933 ) ;
#22106 = AXIS2_PLACEMENT_3D ( 'NONE', #17475, #11062, #1321 ) ;
#22107 = ADVANCED_FACE ( 'NONE', ( #20336 ), #25234, .T. ) ;
#22108 = ADVANCED_FACE ( 'NONE', ( #20635, #4320 ), #29726, .T. ) ;
#22109 = EDGE_CURVE ( 'NONE', #7751, #29440, #6318, .T. ) ;
#22110 = CARTESIAN_POINT ( 'NONE',  ( 13.12362514754451759, 8.570858352459396201, -15.91189866610160841 ) ) ;
#22111 = CARTESIAN_POINT ( 'NONE',  ( 35.18065281855160720, -20.53155141575438591, -20.22037173032050461 ) ) ;
#22112 = ORIENTED_EDGE ( 'NONE', *, *, #16939, .T. ) ;
#22113 = CARTESIAN_POINT ( 'NONE',  ( 9.153102208164984432, 15.99530481237056989, -17.03794677594065021 ) ) ;
#22114 = CARTESIAN_POINT ( 'NONE',  ( 27.95388715220626707, -5.541385876428546631, -15.41148221666858831 ) ) ;
#22115 = CARTESIAN_POINT ( 'NONE',  ( 10.35865266338826984, 16.97210907862488938, -17.91126819201198472 ) ) ;
#22116 = FACE_BOUND ( 'NONE', #13177, .T. ) ;
#22117 = VERTEX_POINT ( 'NONE', #20050 ) ;
#22118 = DIRECTION ( 'NONE',  ( 1.110223024625156540E-16, 2.995891024602366092E-32, 1.000000000000000000 ) ) ;
#22119 = ORIENTED_EDGE ( 'NONE', *, *, #23958, .T. ) ;
#22120 = CARTESIAN_POINT ( 'NONE',  ( 11.47181023233108021, 9.274170903235749108, -15.86135313853478657 ) ) ;
#22121 = CARTESIAN_POINT ( 'NONE',  ( 139.5152310637605524, -10.00000000000000533, -4.391296821672111328 ) ) ;
#22122 = VERTEX_POINT ( 'NONE', #6465 ) ;
#22123 = DIRECTION ( 'NONE',  ( -0.9510565162951536422, -2.566386769018988816E-16, -0.3090169943749472292 ) ) ;
#22124 = ORIENTED_EDGE ( 'NONE', *, *, #27766, .F. ) ;
#22125 = CARTESIAN_POINT ( 'NONE',  ( 12.02817646543008934, 9.315460371489308500, -16.69127922251917795 ) ) ;
#22126 = CARTESIAN_POINT ( 'NONE',  ( 20.94368124868196901, 3.275021729503806878, -20.72479390824751633 ) ) ;
#22127 = CARTESIAN_POINT ( 'NONE',  ( 22.56675539556120924, 5.189497681140571750, -18.50903523470404011 ) ) ;
#22128 = DIRECTION ( 'NONE',  ( -0.9510565162951536422, -2.566386769018988816E-16, -0.3090169943749472292 ) ) ;
#22129 = VECTOR ( 'NONE', #5632, 1000.000000000000000 ) ;
#22130 = CARTESIAN_POINT ( 'NONE',  ( 35.98907965336992731, -19.67091466371804742, -20.42083605867238205 ) ) ;
#22131 = ADVANCED_FACE ( 'NONE', ( #29877 ), #27559, .T. ) ;
#22132 = CARTESIAN_POINT ( 'NONE',  ( 16.89609864265585060, 4.102175112930991574, -14.31125941877678720 ) ) ;
#22133 = SURFACE_STYLE_USAGE ( .BOTH. , #21537 ) ;
#22134 = DIRECTION ( 'NONE',  ( 0.000000000000000000, 0.000000000000000000, 1.000000000000000000 ) ) ;
#22135 = ADVANCED_FACE ( 'NONE', ( #29422 ), #13766, .T. ) ;
#22136 = EDGE_CURVE ( 'NONE', #26624, #20158, #8589, .T. ) ;
#22137 = EDGE_CURVE ( 'NONE', #9311, #25636, #6610, .T. ) ;
#22138 = LINE ( 'NONE', #5819, #9884 ) ;
#22139 = CARTESIAN_POINT ( 'NONE',  ( 35.16668739017224965, -20.46881214373840763, -20.22602438870426766 ) ) ;
#22140 = DIRECTION ( 'NONE',  ( -0.5877852522924731371, -1.586114251531760235E-16, 0.8090169943749474513 ) ) ;
#22141 = LINE ( 'NONE', #24591, #2702 ) ;
#22142 = VECTOR ( 'NONE', #23155, 1000.000000000000000 ) ;
#22143 = CARTESIAN_POINT ( 'NONE',  ( 12.27549906412561675, 9.499463866199420181, -15.31139863700699344 ) ) ;
#22144 = DIRECTION ( 'NONE',  ( -2.698458740408365879E-16, 1.000000000000000000, 0.000000000000000000 ) ) ;
#22145 = VERTEX_POINT ( 'NONE', #22949 ) ;
#22146 = CARTESIAN_POINT ( 'NONE',  ( 420.0000000000002274, 27.64101615137744972, 14.00000000000000178 ) ) ;
#22147 = ORIENTED_EDGE ( 'NONE', *, *, #4948, .F. ) ;
#22148 = CARTESIAN_POINT ( 'NONE',  ( 12.49899259368311988, 8.570259324921714494, -15.13097775544467005 ) ) ;
#22149 = ORIENTED_EDGE ( 'NONE', *, *, #4699, .F. ) ;
#22150 = CARTESIAN_POINT ( 'NONE',  ( 10.65857126575392400, 9.091031811597934720, -16.41538236262689310 ) ) ;
#22151 = DIRECTION ( 'NONE',  ( 1.000000000000000000, 2.908569913943825554E-16, -6.938893903907227392E-16 ) ) ;
#22152 = DIRECTION ( 'NONE',  ( -0.000000000000000000, -0.000000000000000000, 1.000000000000000000 ) ) ;
#22153 = DIRECTION ( 'NONE',  ( -2.698458740408365879E-16, 1.000000000000000000, 0.000000000000000000 ) ) ;
#22154 = ORIENTED_EDGE ( 'NONE', *, *, #29958, .T. ) ;
#22155 = CARTESIAN_POINT ( 'NONE',  ( 12.82413367917259706, 9.577855520724041227, -16.14439663126654523 ) ) ;
#22156 = VERTEX_POINT ( 'NONE', #17747 ) ;
#22157 = CARTESIAN_POINT ( 'NONE',  ( 34.58206770820681442, -12.34995000336197890, -18.95321163875382453 ) ) ;
#22158 = CARTESIAN_POINT ( 'NONE',  ( 22.09544204423535874, -4.864148257255451746, -14.35781331922719772 ) ) ;
#22159 = ORIENTED_EDGE ( 'NONE', *, *, #23339, .F. ) ;
#22160 = EDGE_LOOP ( 'NONE', ( #7820, #21809, #2480, #17977 ) ) ;
#22161 = VERTEX_POINT ( 'NONE', #27105 ) ;
#22162 = DIRECTION ( 'NONE',  ( -1.110223024625156540E-16, 0.000000000000000000, -1.000000000000000000 ) ) ;
#22163 = CARTESIAN_POINT ( 'NONE',  ( 13.51621490077814691, 9.019785729699995258, -14.32023381125561556 ) ) ;
#22164 = CARTESIAN_POINT ( 'NONE',  ( -4.000000000000003553, 0.3904826640787941172, -2.138334675343480417E-15 ) ) ;
#22165 = DIRECTION ( 'NONE',  ( -0.000000000000000000, -0.000000000000000000, 1.000000000000000000 ) ) ;
#22166 = ADVANCED_FACE ( 'NONE', ( #15613, #17887, #6765, #18351 ), #16057, .T. ) ;
#22167 =( NAMED_UNIT ( * ) PLANE_ANGLE_UNIT ( ) SI_UNIT ( $, .RADIAN. ) );
#22168 = CARTESIAN_POINT ( 'NONE',  ( 23.76385019584477831, -1.264968635605209446, -19.12809044524397351 ) ) ;
#22169 = CARTESIAN_POINT ( 'NONE',  ( 22.35455276305805938, 2.055732105393538678, -20.05127887597516434 ) ) ;
#22170 = VECTOR ( 'NONE', #21544, 1000.000000000000000 ) ;
#22171 = ORIENTED_EDGE ( 'NONE', *, *, #11652, .F. ) ;
#22172 = VERTEX_POINT ( 'NONE', #25384 ) ;
#22173 = DIRECTION ( 'NONE',  ( 0.000000000000000000, 0.000000000000000000, 1.000000000000000000 ) ) ;
#22174 = CARTESIAN_POINT ( 'NONE',  ( 420.0000000000002274, 34.64101615137744972, 12.00000000000000178 ) ) ;
#22175 = CARTESIAN_POINT ( 'NONE',  ( 139.5152310637605808, -1.999999999999978684, -21.71180489736090991 ) ) ;
#22176 = FACE_OUTER_BOUND ( 'NONE', #25772, .T. ) ;
#22177 = DIRECTION ( 'NONE',  ( -0.9510565162951536422, 0.000000000000000000, -0.3090169943749472292 ) ) ;
#22178 = DIRECTION ( 'NONE',  ( -2.698458740408365879E-16, 1.000000000000000000, 0.000000000000000000 ) ) ;
#22179 = CARTESIAN_POINT ( 'NONE',  ( 11.47219014545126647, 9.272428573238919114, -15.86119603109536058 ) ) ;
#22180 = CARTESIAN_POINT ( 'NONE',  ( 15.19603151210977821, 9.502094893032342782, -14.87270315361914896 ) ) ;
#22181 = CARTESIAN_POINT ( 'NONE',  ( 25.47985489653468605, -2.350970512090694520, -13.88367939857760014 ) ) ;
#22182 = ORIENTED_EDGE ( 'NONE', *, *, #29927, .F. ) ;
#22183 = DIRECTION ( 'NONE',  ( 0.000000000000000000, 0.000000000000000000, 1.000000000000000000 ) ) ;
#22184 = CARTESIAN_POINT ( 'NONE',  ( 152.0152310637605524, -10.00000000000000000, -26.04193191628311155 ) ) ;
#22185 = CARTESIAN_POINT ( 'NONE',  ( 36.04859390953723874, -22.18451583373416014, -36.50100000000000477 ) ) ;
#22186 = CARTESIAN_POINT ( 'NONE',  ( -7.806255641895631925E-14, -4.618802153517044928, -0.3572655899081716435 ) ) ;
#22187 = VECTOR ( 'NONE', #19069, 1000.000000000000000 ) ;
#22188 = CARTESIAN_POINT ( 'NONE',  ( -24.99999999999998934, 60.00000000000000711, 29.99999999999999289 ) ) ;
#22189 = PLANE ( 'NONE',  #2944 ) ;
#22190 = CARTESIAN_POINT ( 'NONE',  ( 18.80472905218952917, 2.352968372735388503, -20.19605574946481497 ) ) ;
#22191 = ORIENTED_EDGE ( 'NONE', *, *, #12111, .T. ) ;
#22192 = CARTESIAN_POINT ( 'NONE',  ( 147.0152310637605808, -1.999999999999976241, -26.04193191628311155 ) ) ;
#22193 = CARTESIAN_POINT ( 'NONE',  ( 12.27687350794345456, 9.494798321042301481, -15.31070534102384251 ) ) ;
#22194 = DIRECTION ( 'NONE',  ( -2.698458740408366372E-16, 1.000000000000000000, 0.000000000000000000 ) ) ;
#22195 = DIRECTION ( 'NONE',  ( 0.000000000000000000, -0.5000000000000012212, -0.8660254037844380415 ) ) ;
#22196 = ORIENTED_EDGE ( 'NONE', *, *, #8104, .F. ) ;
#22197 = CARTESIAN_POINT ( 'NONE',  ( 23.66601916330066402, 2.199037240492611733, -18.57254039386976885 ) ) ;
#22198 = DIRECTION ( 'NONE',  ( 0.3090169943749475623, 8.338696094058001131E-17, 0.9510565162951536422 ) ) ;
#22199 = CARTESIAN_POINT ( 'NONE',  ( 20.97270766892557603, 0.7925772802953747753, -14.00178974354743033 ) ) ;
#22200 = ORIENTED_EDGE ( 'NONE', *, *, #11318, .F. ) ;
#22201 = CARTESIAN_POINT ( 'NONE',  ( 35.54859390953724585, -22.18451583373416014, -18.06010107863414405 ) ) ;
#22202 = VECTOR ( 'NONE', #10780, 999.9999999999998863 ) ;
#22203 = EDGE_CURVE ( 'NONE', #4780, #13842, #20302, .T. ) ;
#22204 = CARTESIAN_POINT ( 'NONE',  ( 22.59934115267691368, -6.304331921927718518, -14.46034029096162143 ) ) ;
#22205 = EDGE_CURVE ( 'NONE', #10296, #981, #29126, .T. ) ;
#22206 = CARTESIAN_POINT ( 'NONE',  ( 19.83814782303322133, -0.7621604502531613701, -13.87429439740111370 ) ) ;
#22207 = VECTOR ( 'NONE', #15695, 1000.000000000000000 ) ;
#22208 = ORIENTED_EDGE ( 'NONE', *, *, #27967, .F. ) ;
#22209 = CARTESIAN_POINT ( 'NONE',  ( 27.11191462667604313, -11.78482644060662743, -13.28705938033944989 ) ) ;
#22210 = VECTOR ( 'NONE', #28084, 1000.000000000000000 ) ;
#22211 = VECTOR ( 'NONE', #1786, 1000.000000000000000 ) ;
#22212 = CARTESIAN_POINT ( 'NONE',  ( 161.1922820468853956, -1.999999999999972689, -30.91696583120936026 ) ) ;
#22213 = ORIENTED_EDGE ( 'NONE', *, *, #21137, .F. ) ;
#22214 = LINE ( 'NONE', #7880, #25838 ) ;
#22215 = DIRECTION ( 'NONE',  ( -2.698458740408365879E-16, 1.000000000000000000, 0.000000000000000000 ) ) ;
#22216 = DIRECTION ( 'NONE',  ( -0.9510565162951536422, -2.566386769018988323E-16, 0.3090169943749475623 ) ) ;
#22217 = DIRECTION ( 'NONE',  ( 0.9510565162951535312, 2.566386769018988816E-16, -0.3090169943749475623 ) ) ;
#22218 = CARTESIAN_POINT ( 'NONE',  ( 26.88076058338416274, -6.009164776401831887, -18.61148891559023255 ) ) ;
#22219 = DIRECTION ( 'NONE',  ( -0.9773680663943724589, 3.177847737406115317E-17, -0.2115458881484709175 ) ) ;
#22220 = CARTESIAN_POINT ( 'NONE',  ( 36.54460969663918490, -22.16661687567949457, -18.62492107750662029 ) ) ;
#22221 = CARTESIAN_POINT ( 'NONE',  ( 95.85195911941896441, -4.999999999999991118, 69.64052469288915859 ) ) ;
#22222 = CARTESIAN_POINT ( 'NONE',  ( 9.912057827679275235, 16.42739425315605928, -16.50652470164456531 ) ) ;
#22223 = CIRCLE ( 'NONE', #23205, 4.000000000000000000 ) ;
#22224 = DIRECTION ( 'NONE',  ( 0.000000000000000000, 0.000000000000000000, -1.000000000000000000 ) ) ;
#22225 = CARTESIAN_POINT ( 'NONE',  ( 161.1922820468853104, -10.00000000000000000, -2.083034168790677043 ) ) ;
#22226 = CARTESIAN_POINT ( 'NONE',  ( 15.00903923349565972, 9.404056492746565965, -14.40919036548495669 ) ) ;
#22227 = CARTESIAN_POINT ( 'NONE',  ( 152.0152310637605808, -4.999999999999976907, -34.70218595412750773 ) ) ;
#22228 = LINE ( 'NONE', #15197, #11953 ) ;
#22229 = CARTESIAN_POINT ( 'NONE',  ( 11.31072706937237982, 10.01291882189198112, -15.92796669285280764 ) ) ;
#22230 = EDGE_LOOP ( 'NONE', ( #21368, #17478, #964, #21524 ) ) ;
#22231 = AXIS2_PLACEMENT_3D ( 'NONE', #6365, #11081, #8928 ) ;
#22232 = DIRECTION ( 'NONE',  ( -2.698458740408365879E-16, 1.000000000000000000, -0.000000000000000000 ) ) ;
#22233 = CARTESIAN_POINT ( 'NONE',  ( 144.5152310637605524, -1.999999999999978018, -2.627941064794695691 ) ) ;
#22234 = AXIS2_PLACEMENT_3D ( 'NONE', #16714, #28812, #5418 ) ;
#22235 = LINE ( 'NONE', #26384, #5408 ) ;
#22236 = ORIENTED_EDGE ( 'NONE', *, *, #30164, .F. ) ;
#22237 = EDGE_LOOP ( 'NONE', ( #17990, #15198, #17997, #21099, #10503 ) ) ;
#22238 = CARTESIAN_POINT ( 'NONE',  ( 13.92371455371928590, 7.866402339252101861, -15.27421329262669936 ) ) ;
#22239 = ADVANCED_FACE ( 'NONE', ( #1602 ), #15758, .T. ) ;
#22240 = EDGE_CURVE ( 'NONE', #15364, #26933, #25082, .T. ) ;
#22241 = CARTESIAN_POINT ( 'NONE',  ( 16.38450301900381945, 9.168174629645104545, -21.04437084800770918 ) ) ;
#22242 = EDGE_CURVE ( 'NONE', #27200, #12000, #22794, .T. ) ;
#22243 = CARTESIAN_POINT ( 'NONE',  ( 30.62762753239542590, -8.735908549479720620, -17.37160549233551876 ) ) ;
#22244 = DIRECTION ( 'NONE',  ( -2.698458740408365879E-16, 1.000000000000000000, 0.000000000000000000 ) ) ;
#22245 = DIRECTION ( 'NONE',  ( -0.5877852522924731371, 0.000000000000000000, 0.8090169943749474513 ) ) ;
#22246 = EDGE_CURVE ( 'NONE', #26241, #18105, #20490, .T. ) ;
#22247 = FACE_OUTER_BOUND ( 'NONE', #9960, .T. ) ;
#22248 = AXIS2_PLACEMENT_3D ( 'NONE', #97, #8785, #15806 ) ;
#22249 = VERTEX_POINT ( 'NONE', #28007 ) ;
#22250 = ORIENTED_EDGE ( 'NONE', *, *, #9367, .T. ) ;
#22251 = LINE ( 'NONE', #17807, #1627 ) ;
#22252 = CARTESIAN_POINT ( 'NONE',  ( 169.5152310637604103, -9.999999999999996447, -4.391296821672111328 ) ) ;
#22253 = VECTOR ( 'NONE', #29886, 1000.000000000000000 ) ;
#22254 = CARTESIAN_POINT ( 'NONE',  ( 146.1922820468853956, -10.00000000000000355, -4.936203717676158398 ) ) ;
#22255 = DIRECTION ( 'NONE',  ( 0.000000000000000000, 0.000000000000000000, 1.000000000000000000 ) ) ;
#22256 = CARTESIAN_POINT ( 'NONE',  ( 12.14965596459611774, 8.983642127099937369, -16.62385966901067391 ) ) ;
#22257 = CARTESIAN_POINT ( 'NONE',  ( 35.54859390954303677, -22.18451583373416014, -15.55638201429745848 ) ) ;
#22258 = VERTEX_POINT ( 'NONE', #27862 ) ;
#22259 = CARTESIAN_POINT ( 'NONE',  ( 9.098468484354940600, 16.24586203394349582, -17.06302340752861824 ) ) ;
#22260 = ORIENTED_EDGE ( 'NONE', *, *, #29445, .T. ) ;
#22261 = CARTESIAN_POINT ( 'NONE',  ( 21.94319337455657859, -4.318501116253552041, -18.82930321547734920 ) ) ;
#22262 = CARTESIAN_POINT ( 'NONE',  ( 12.87265939729807762, 9.517981781931423413, -16.11192280467173532 ) ) ;
#22263 = FACE_BOUND ( 'NONE', #10660, .T. ) ;
#22264 = ORIENTED_EDGE ( 'NONE', *, *, #21169, .F. ) ;
#22265 = ORIENTED_EDGE ( 'NONE', *, *, #21724, .T. ) ;
#22266 = PLANE ( 'NONE',  #771 ) ;
#22267 = CONICAL_SURFACE ( 'NONE', #14930, 2.041999999999999815, 1.047197551196591858 ) ;
#22268 = CARTESIAN_POINT ( 'NONE',  ( 11.47310491742633687, 9.268236560789974376, -15.86081749295074594 ) ) ;
#22269 = DIRECTION ( 'NONE',  ( 1.734723475976807587E-16, 0.000000000000000000, 1.000000000000000000 ) ) ;
#22270 = VERTEX_POINT ( 'NONE', #16359 ) ;
#22271 = ORIENTED_EDGE ( 'NONE', *, *, #29135, .T. ) ;
#22272 = PLANE ( 'NONE',  #28157 ) ;
#22273 = ORIENTED_EDGE ( 'NONE', *, *, #22462, .T. ) ;
#22274 = CARTESIAN_POINT ( 'NONE',  ( 9.661883107508126400, 16.25482642313383508, -17.91565355200308218 ) ) ;
#22275 = VERTEX_POINT ( 'NONE', #28462 ) ;
#22276 = VECTOR ( 'NONE', #3815, 1000.000000000000000 ) ;
#22277 = CARTESIAN_POINT ( 'NONE',  ( 17.94761415789183445, 0.5003475314714088684, -19.87472444338139965 ) ) ;
#22278 = CARTESIAN_POINT ( 'NONE',  ( 17.49129197179432538, 0.06586305242593921971, -19.15772692538415356 ) ) ;
#22279 = EDGE_CURVE ( 'NONE', #6635, #18739, #25682, .T. ) ;
#22280 = CARTESIAN_POINT ( 'NONE',  ( 149.7287565553229456, -1.999999999999976685, 0.8205080756887930260 ) ) ;
#22281 = ADVANCED_FACE ( 'NONE', ( #356 ), #23694, .T. ) ;
#22282 = VERTEX_POINT ( 'NONE', #4920 ) ;
#22283 = EDGE_CURVE ( 'NONE', #15020, #8203, #9482, .T. ) ;
#22284 = DIRECTION ( 'NONE',  ( -2.698458740408365879E-16, 1.000000000000000000, 0.000000000000000000 ) ) ;
#22285 = CARTESIAN_POINT ( 'NONE',  ( 17.08157517049449581, 7.460725202527481947, -14.57009041681831896 ) ) ;
#22286 = ORIENTED_EDGE ( 'NONE', *, *, #5974, .F. ) ;
#22287 = CARTESIAN_POINT ( 'NONE',  ( 5.000000000000000000, -6.123233995736766282E-16, -23.00000000000000000 ) ) ;
#22288 = FACE_BOUND ( 'NONE', #23381, .T. ) ;
#22289 = VECTOR ( 'NONE', #2169, 1000.000000000000000 ) ;
#22290 = B_SPLINE_CURVE_WITH_KNOTS ( 'NONE', 3,
 ( #1246, #6427, #29372, #26908, #8245, #1864, #13126, #1556, #11141, #20445, #6273, #1699, #17699, #17400, #20291, #22454, #12980, #17556, #3680, #22751, #22293, #24747, #25047, #15259, #27060, #4132, #26750, #27221, #29678, #15565, #13425, #5820, #10836, #18005, #24588, #5970, #1400, #15106, #12825, #10691, #24438, #8396, #29525, #20004, #24899, #20144, #3983, #8695, #6116, #15413, #8544, #27374, #3533, #22139, #17845, #13728, #157, #9435, #18761, #18158, #6723, #8984, #8844, #16465, #29977, #9289, #13869, #30127, #20893, #11733, #23056, #14169, #28114, #15862, #23495, #11428, #4873, #18305 ),
 .UNSPECIFIED., .F., .F.,
 ( 4, 2, 2, 2, 2, 2, 2, 2, 2, 2, 2, 2, 2, 2, 2, 2, 2, 2, 2, 2, 2, 2, 2, 2, 2, 2, 2, 2, 2, 2, 2, 2, 2, 2, 2, 2, 2, 2, 4 ),
 ( 0.04625696548581515605, 0.1003381136405422785, 0.1505071704608134109, 0.1755916988709489979, 0.1881339630760167636, 0.1944050951785506465, 0.2006762272810845571, 0.2086934065084689038, 0.2167105857358532783, 0.2327449441906219718, 0.2648136611001593588, 0.2968823780096967457, 0.3129167364644654947, 0.3209339156918498137, 0.3289510949192341882, 0.3346579968240730452, 0.3403648987289118466, 0.3517787025385894495, 0.3746063101579446553, 0.4202615253966550668, 0.5115719558740758899, 0.6028823863514967130, 0.6485376015902071245, 0.6713652092095623303, 0.6827790130192399332, 0.6941928168289175360, 0.7036545619149295883, 0.7131163070009416405, 0.7320397971729657449, 0.7698867775170139538, 0.8077337578610620517, 0.8266572480330862671, 0.8361189931190984304, 0.8455807382051104826, 0.8552319420672911399, 0.8648831459294716861, 0.8841855536538327787, 0.9227903691025551858, 1.000000000000000000 ),
 .UNSPECIFIED. ) ;
#22291 = ORIENTED_EDGE ( 'NONE', *, *, #4908, .F. ) ;
#22292 = DIRECTION ( 'NONE',  ( 0.3090169943749475623, 8.338696094058001131E-17, 0.9510565162951536422 ) ) ;
#22293 = CARTESIAN_POINT ( 'NONE',  ( 32.96569147872224903, -11.36116021242123608, -19.12347989294568151 ) ) ;
#22294 = DIRECTION ( 'NONE',  ( -2.698458740408365879E-16, 1.000000000000000000, 0.000000000000000000 ) ) ;
#22295 = VECTOR ( 'NONE', #13194, 1000.000000000000000 ) ;
#22296 = ORIENTED_EDGE ( 'NONE', *, *, #21134, .T. ) ;
#22297 = VERTEX_POINT ( 'NONE', #30171 ) ;
#22298 = LINE ( 'NONE', #3536, #21706 ) ;
#22299 = CARTESIAN_POINT ( 'NONE',  ( 12.24519447470441413, 9.516128708456710328, -15.33325952276184445 ) ) ;
#22300 = ORIENTED_EDGE ( 'NONE', *, *, #16738, .F. ) ;
#22301 = DIRECTION ( 'NONE',  ( 1.110223024625156540E-16, 2.995891024602366092E-32, 1.000000000000000000 ) ) ;
#22302 = ORIENTED_EDGE ( 'NONE', *, *, #12374, .T. ) ;
#22303 = FACE_OUTER_BOUND ( 'NONE', #27527, .T. ) ;
#22304 = ORIENTED_EDGE ( 'NONE', *, *, #155, .F. ) ;
#22305 = CARTESIAN_POINT ( 'NONE',  ( 10.66464987567688993, 9.063154531648658363, -16.41286864359600983 ) ) ;
#22306 = CARTESIAN_POINT ( 'NONE',  ( 168.6922820468853672, -9.999999999999996447, -23.73366926340167637 ) ) ;
#22307 = CARTESIAN_POINT ( 'NONE',  ( 111.9672181541861278, -4.999999999999986677, -81.34894573147012409 ) ) ;
#22308 = ORIENTED_EDGE ( 'NONE', *, *, #11534, .F. ) ;
#22309 = LINE ( 'NONE', #7671, #2775 ) ;
#22310 = ORIENTED_EDGE ( 'NONE', *, *, #27256, .F. ) ;
#22311 = CARTESIAN_POINT ( 'NONE',  ( 10.35864918915110877, 16.97212501191939538, -17.93331994345748370 ) ) ;
#22312 = CARTESIAN_POINT ( 'NONE',  ( 35.14511844984765787, -14.87944403499761670, -19.12340528518704730 ) ) ;
#22313 = CARTESIAN_POINT ( 'NONE',  ( 23.76365953361780470, 2.837943588559999508, -16.54419024451982168 ) ) ;
#22314 = ORIENTED_EDGE ( 'NONE', *, *, #3862, .F. ) ;
#22315 = EDGE_CURVE ( 'NONE', #929, #18003, #28313, .T. ) ;
#22316 = EDGE_LOOP ( 'NONE', ( #24066, #21872, #14323, #8207 ) ) ;
#22317 = EDGE_CURVE ( 'NONE', #4321, #17684, #14214, .T. ) ;
#22318 = VECTOR ( 'NONE', #19925, 1000.000000000000000 ) ;
#22319 = CYLINDRICAL_SURFACE ( 'NONE', #9632, 13.00000000000000178 ) ;
#22320 = CARTESIAN_POINT ( 'NONE',  ( 13.76974871631934860, 5.358497188706473402, -17.46738557873778674 ) ) ;
#22321 = EDGE_CURVE ( 'NONE', #27966, #21114, #20778, .T. ) ;
#22322 = CARTESIAN_POINT ( 'NONE',  ( 8.000000000000015987, -1.555946510856142551, -4.932911297836637843 ) ) ;
#22323 = EDGE_CURVE ( 'NONE', #6890, #27640, #14513, .T. ) ;
#22324 = DIRECTION ( 'NONE',  ( -3.216245299353268764E-16, 1.000000000000000000, 0.000000000000000000 ) ) ;
#22325 = CARTESIAN_POINT ( 'NONE',  ( 27.61484239614359737, -11.78684095324212855, -18.66559939683001446 ) ) ;
#22326 = VECTOR ( 'NONE', #11761, 1000.000000000000000 ) ;
#22327 = CARTESIAN_POINT ( 'NONE',  ( 19.10622122644073428, 3.678778577015775042, -19.67015202264490625 ) ) ;
#22328 = VERTEX_POINT ( 'NONE', #16213 ) ;
#22329 = CARTESIAN_POINT ( 'NONE',  ( 119.9999999999999858, -30.00000000000000000, -15.00000000000000000 ) ) ;
#22330 = AXIS2_PLACEMENT_3D ( 'NONE', #10384, #21686, #10079 ) ;
#22331 = DIRECTION ( 'NONE',  ( 0.000000000000000000, 1.000000000000000000, 0.000000000000000000 ) ) ;
#22332 = FACE_OUTER_BOUND ( 'NONE', #4051, .T. ) ;
#22333 = LINE ( 'NONE', #4015, #12526 ) ;
#22334 = CARTESIAN_POINT ( 'NONE',  ( 37.54859390953724585, -22.18451583373416014, -15.00000000000000000 ) ) ;
#22335 = DIRECTION ( 'NONE',  ( 0.000000000000000000, 0.000000000000000000, 1.000000000000000000 ) ) ;
#22336 = UNCERTAINTY_MEASURE_WITH_UNIT (LENGTH_MEASURE( 1.000000000000000082E-05 ), #24465, 'distance_accuracy_value', 'NONE');
#22337 = CARTESIAN_POINT ( 'NONE',  ( 11.60705119439842292, 8.210639978236427439, -17.01629833992986462 ) ) ;
#22338 = ORIENTED_EDGE ( 'NONE', *, *, #3005, .T. ) ;
#22339 = CARTESIAN_POINT ( 'NONE',  ( 10.33811693838771717, 18.38618951776012267, -17.91928203681695564 ) ) ;
#22340 = CARTESIAN_POINT ( 'NONE',  ( 23.72517123929712213, -5.798560033841243744, -19.46542475990168342 ) ) ;
#22341 = ORIENTED_EDGE ( 'NONE', *, *, #25662, .F. ) ;
#22342 = CARTESIAN_POINT ( 'NONE',  ( 133.6922820468854241, -10.00000000000000711, -35.24709285013155835 ) ) ;
#22343 = CIRCLE ( 'NONE', #27267, 0.4999999999999986677 ) ;
#22344 = DIRECTION ( 'NONE',  ( -2.698458740408365879E-16, 1.000000000000000000, 0.000000000000000000 ) ) ;
#22345 = ORIENTED_EDGE ( 'NONE', *, *, #12895, .T. ) ;
#22346 = CARTESIAN_POINT ( 'NONE',  ( 9.905109554012803130, 16.45925992188944420, -16.51025697316969953 ) ) ;
#22347 = DIRECTION ( 'NONE',  ( -0.8090169943749474513, -2.183098979609982436E-16, -0.5877852522924731371 ) ) ;
#22348 = FILL_AREA_STYLE_COLOUR ( '', #15103 ) ;
#22349 = CARTESIAN_POINT ( 'NONE',  ( 24.43075134246613800, -6.859861339260811874, -14.00379227226492951 ) ) ;
#22350 = AXIS2_PLACEMENT_3D ( 'NONE', #18603, #23180, #4005 ) ;
#22351 = ORIENTED_EDGE ( 'NONE', *, *, #10348, .F. ) ;
#22352 = CARTESIAN_POINT ( 'NONE',  ( 12.90791573655052282, -5.000000000000014211, 39.72647976162691918 ) ) ;
#22353 = CARTESIAN_POINT ( 'NONE',  ( 12.27289197906229745, 9.513064554772155290, -15.31235135250446078 ) ) ;
#22354 = AXIS2_PLACEMENT_3D ( 'NONE', #21542, #643, #26587 ) ;
#22355 = CARTESIAN_POINT ( 'NONE',  ( 144.7287565553230309, -10.00000000000000355, -25.16025403784439973 ) ) ;
#22356 = CARTESIAN_POINT ( 'NONE',  ( 79.06642017383501297, -4.999999999999995559, 57.44511679343214894 ) ) ;
#22357 = CARTESIAN_POINT ( 'NONE',  ( 21.94319337455657859, -4.318501116253552041, -18.82930321547734920 ) ) ;
#22358 = CARTESIAN_POINT ( 'NONE',  ( 172.2287565553229456, -9.999999999999994671, -29.49038105676660493 ) ) ;
#22359 = CARTESIAN_POINT ( 'NONE',  ( 20.90484242567171691, 8.469164366756103846, -17.19731680296963106 ) ) ;
#22360 = EDGE_CURVE ( 'NONE', #7643, #18212, #2508, .T. ) ;
#22361 = ORIENTED_EDGE ( 'NONE', *, *, #13179, .T. ) ;
#22362 = EDGE_CURVE ( 'NONE', #26545, #3816, #15426, .T. ) ;
#22363 = LINE ( 'NONE', #3899, #22756 ) ;
#22364 =( NAMED_UNIT ( * ) SI_UNIT ( $, .STERADIAN. ) SOLID_ANGLE_UNIT ( ) );
#22365 = CARTESIAN_POINT ( 'NONE',  ( 23.25962485557060688, -10.00107805802020167, -16.29084171305886386 ) ) ;
#22366 = CARTESIAN_POINT ( 'NONE',  ( 20.11894618883271946, -4.454955732405634805, -18.36807076737963129 ) ) ;
#22367 =( REPRESENTATION_RELATIONSHIP ('NONE','NONE', #5250, #6235 ) REPRESENTATION_RELATIONSHIP_WITH_TRANSFORMATION ( #17545 )SHAPE_REPRESENTATION_RELATIONSHIP( ) );
#22368 = VERTEX_POINT ( 'NONE', #2354 ) ;
#22369 = CARTESIAN_POINT ( 'NONE',  ( 26.48263329513011755, -12.06126822337667903, -13.95730679897583038 ) ) ;
#22370 = VECTOR ( 'NONE', #5255, 1000.000000000000000 ) ;
#22371 = DIRECTION ( 'NONE',  ( 1.000000000000000000, 2.698458740408365879E-16, -1.110223024625156540E-16 ) ) ;
#22372 = VECTOR ( 'NONE', #22486, 1000.000000000000000 ) ;
#22373 = ORIENTED_EDGE ( 'NONE', *, *, #28760, .F. ) ;
#22374 = AXIS2_PLACEMENT_3D ( 'NONE', #2459, #18462, #27815 ) ;
#22375 = DIRECTION ( 'NONE',  ( -2.698458740408365879E-16, 1.000000000000000000, 0.000000000000000000 ) ) ;
#22376 = DIRECTION ( 'NONE',  ( -1.000000000000000000, 0.000000000000000000, 0.000000000000000000 ) ) ;
#22377 = LINE ( 'NONE', #24823, #29012 ) ;
#22378 = DIRECTION ( 'NONE',  ( -1.110223024625156540E-16, 0.000000000000000000, -1.000000000000000000 ) ) ;
#22379 = CARTESIAN_POINT ( 'NONE',  ( 23.13192804015912785, -6.366449129859712563, -15.65771855518050870 ) ) ;
#22380 = CYLINDRICAL_SURFACE ( 'NONE', #27808, 1.499999999999996225 ) ;
#22381 = EDGE_CURVE ( 'NONE', #11253, #3713, #21095, .T. ) ;
#22382 = CARTESIAN_POINT ( 'NONE',  ( 32.72409873491027099, -9.637868425582460929, -18.36260606011342844 ) ) ;
#22383 = DIRECTION ( 'NONE',  ( -0.9510565162951536422, -2.566386769018988816E-16, -0.3090169943749472292 ) ) ;
#22384 = CARTESIAN_POINT ( 'NONE',  ( 9.916775705961365261, 16.40575746196480011, -16.50441451066904364 ) ) ;
#22385 = LINE ( 'NONE', #6506, #1044 ) ;
#22386 = DIRECTION ( 'NONE',  ( 0.9510565162951536422, 0.000000000000000000, -0.3090169943749475623 ) ) ;
#22387 = CARTESIAN_POINT ( 'NONE',  ( 9.661883061612440926, 16.25482663361732705, -17.92015940598198753 ) ) ;
#22388 = CARTESIAN_POINT ( 'NONE',  ( 167.0152310637604387, -1.999999999999971800, -8.721423840594312082 ) ) ;
#22389 = ORIENTED_EDGE ( 'NONE', *, *, #18980, .T. ) ;
#22390 = DIRECTION ( 'NONE',  ( -0.000000000000000000, -0.000000000000000000, -1.000000000000000000 ) ) ;
#22391 = CARTESIAN_POINT ( 'NONE',  ( 9.981537699549546616, 16.10875070413535681, -16.47763325427154868 ) ) ;
#22392 = ORIENTED_EDGE ( 'NONE', *, *, #28365, .T. ) ;
#22393 = VECTOR ( 'NONE', #7363, 1000.000000000000000 ) ;
#22394 = LINE ( 'NONE', #15046, #16845 ) ;
#22395 = CARTESIAN_POINT ( 'NONE',  ( 129.5152310637605524, -10.00000000000000888, -4.391296821672111328 ) ) ;
#22396 = CARTESIAN_POINT ( 'NONE',  ( 17.17204249742301059, 10.23148044644768362, -15.96021614775051667 ) ) ;
#22397 = ORIENTED_EDGE ( 'NONE', *, *, #6601, .T. ) ;
#22398 = CIRCLE ( 'NONE', #9209, 12.50000000000000000 ) ;
#22399 = ORIENTED_EDGE ( 'NONE', *, *, #27764, .T. ) ;
#22400 = CARTESIAN_POINT ( 'NONE',  ( 8.944585198251687075, 16.95159039956950764, -17.91368623377419667 ) ) ;
#22401 = CARTESIAN_POINT ( 'NONE',  ( 34.19383894405228830, -12.60584912221051290, -20.92049940795970997 ) ) ;
#22402 = CARTESIAN_POINT ( 'NONE',  ( 16.80873327975549003, 11.45062080556171757, -15.01659013532395370 ) ) ;
#22403 = CARTESIAN_POINT ( 'NONE',  ( 26.69342817538273138, -7.978421288772274522, -19.59580293194042966 ) ) ;
#22404 = DIRECTION ( 'NONE',  ( -0.5877852522924731371, 0.000000000000000000, 0.8090169943749474513 ) ) ;
#22405 = DIRECTION ( 'NONE',  ( 0.3090169943749475623, 8.338696094058001131E-17, 0.9510565162951536422 ) ) ;
#22406 = LINE ( 'NONE', #13534, #5485 ) ;
#22407 = ORIENTED_EDGE ( 'NONE', *, *, #8422, .T. ) ;
#22408 = ORIENTED_EDGE ( 'NONE', *, *, #2384, .F. ) ;
#22409 = CARTESIAN_POINT ( 'NONE',  ( 5.000000000000000000, -6.123233995736766282E-16, -18.00000000000000000 ) ) ;
#22410 = AXIS2_PLACEMENT_3D ( 'NONE', #30098, #18276, #20419 ) ;
#22411 = VECTOR ( 'NONE', #6609, 1000.000000000000000 ) ;
#22412 = CARTESIAN_POINT ( 'NONE',  ( 167.0152310637604387, -4.999999999999971578, 1.702185954127501066 ) ) ;
#22413 = DIRECTION ( 'NONE',  ( 1.000000000000000000, 4.440892098500622217E-16, 0.000000000000000000 ) ) ;
#22414 = AXIS2_PLACEMENT_3D ( 'NONE', #10460, #21919, #1179 ) ;
#22415 = MECHANICAL_DESIGN_GEOMETRIC_PRESENTATION_REPRESENTATION (  '', ( #14118 ), #21927 ) ;
#22416 = CARTESIAN_POINT ( 'NONE',  ( 13.12048998592846871, 8.569482736746577345, -15.91439669260688561 ) ) ;
#22417 = EDGE_CURVE ( 'NONE', #18049, #24756, #8688, .T. ) ;
#22418 = ADVANCED_FACE ( 'NONE', ( #11626 ), #20786, .T. ) ;
#22419 = CARTESIAN_POINT ( 'NONE',  ( 35.34747194004189907, -20.28098136206135749, -19.25482875754748946 ) ) ;
#22420 = VERTEX_POINT ( 'NONE', #5068 ) ;
#22421 = CARTESIAN_POINT ( 'NONE',  ( 9.112356771736518368, 16.18216857766665484, -17.05479705382001399 ) ) ;
#22422 = EDGE_CURVE ( 'NONE', #9840, #16411, #7219, .T. ) ;
#22423 = EDGE_LOOP ( 'NONE', ( #2362, #16290, #18278, #17095, #17806 ) ) ;
#22424 = ADVANCED_FACE ( 'NONE', ( #9179 ), #9333, .F. ) ;
#22425 = CARTESIAN_POINT ( 'NONE',  ( 31.22280883588763700, -10.09333740185288875, -13.86128061636125786 ) ) ;
#22426 = CARTESIAN_POINT ( 'NONE',  ( 13.14063544215093948, 9.636405190433555035, -15.89834116682275145 ) ) ;
#22427 = FACE_BOUND ( 'NONE', #2178, .T. ) ;
#22428 = ORIENTED_EDGE ( 'NONE', *, *, #17211, .F. ) ;
#22429 = VERTEX_POINT ( 'NONE', #18959 ) ;
#22430 = DIRECTION ( 'NONE',  ( -0.8090169943749474513, -2.183098979609982436E-16, -0.5877852522924731371 ) ) ;
#22431 = CARTESIAN_POINT ( 'NONE',  ( 11.47293561586387867, 9.269010148984008879, -15.86088772249501666 ) ) ;
#22432 = FACE_OUTER_BOUND ( 'NONE', #14291, .T. ) ;
#22433 = LINE ( 'NONE', #11126, #13957 ) ;
#22434 = EDGE_LOOP ( 'NONE', ( #7143, #19524, #16994, #28673 ) ) ;
#22435 = AXIS2_PLACEMENT_3D ( 'NONE', #7052, #14199, #28298 ) ;
#22436 = CARTESIAN_POINT ( 'NONE',  ( 9.661883061612440926, 16.25482663361732705, -21.33333333332589632 ) ) ;
#22437 = ORIENTED_EDGE ( 'NONE', *, *, #13818, .T. ) ;
#22438 = AXIS2_PLACEMENT_3D ( 'NONE', #12690, #12241, #19407 ) ;
#22439 = CARTESIAN_POINT ( 'NONE',  ( 13.73972855572809060, 6.741564148929986011, -15.48174541850189811 ) ) ;
#22440 = CARTESIAN_POINT ( 'NONE',  ( 18.97315296117551497, 8.914538345978252565, -15.07232217507325345 ) ) ;
#22441 = VECTOR ( 'NONE', #28191, 1000.000000000000000 ) ;
#22442 = LINE ( 'NONE', #1999, #18916 ) ;
#22443 = EDGE_LOOP ( 'NONE', ( #13124, #24859, #28811, #5389 ) ) ;
#22444 = CARTESIAN_POINT ( 'NONE',  ( 6.306224973830111935, -5.000000000000015987, 19.40856478368036875 ) ) ;
#22445 = CARTESIAN_POINT ( 'NONE',  ( 23.66272512268759343, 2.894330346666426745, -16.12005855839824520 ) ) ;
#22446 = ORIENTED_EDGE ( 'NONE', *, *, #1417, .T. ) ;
#22447 = CARTESIAN_POINT ( 'NONE',  ( 159.7287565553228887, -10.00000000000000000, 0.8205080756887930260 ) ) ;
#22448 = VECTOR ( 'NONE', #1149, 1000.000000000000000 ) ;
#22449 = FACE_OUTER_BOUND ( 'NONE', #21654, .T. ) ;
#22450 = AXIS2_PLACEMENT_3D ( 'NONE', #28774, #26451, #2806 ) ;
#22451 = VERTEX_POINT ( 'NONE', #7373 ) ;
#22452 = PLANE ( 'NONE',  #148 ) ;
#22453 = EDGE_CURVE ( 'NONE', #563, #9294, #25991, .T. ) ;
#22454 = CARTESIAN_POINT ( 'NONE',  ( 32.67186286342521839, -11.06527230177895227, -18.43913201350460440 ) ) ;
#22455 = VECTOR ( 'NONE', #20971, 1000.000000000000000 ) ;
#22456 = LINE ( 'NONE', #5821, #12633 ) ;
#22457 = ORIENTED_EDGE ( 'NONE', *, *, #10478, .T. ) ;
#22458 = EDGE_CURVE ( 'NONE', #2266, #6973, #28751, .T. ) ;
#22459 = VERTEX_POINT ( 'NONE', #5680 ) ;
#22460 = EDGE_CURVE ( 'NONE', #22503, #10636, #28920, .T. ) ;
#22461 = PLANE ( 'NONE',  #25117 ) ;
#22462 = EDGE_CURVE ( 'NONE', #26251, #4310, #5827, .T. ) ;
#22463 = CARTESIAN_POINT ( 'NONE',  ( 11.05541531668977662, 17.68942339022145305, -17.93331994345748726 ) ) ;
#22464 = CARTESIAN_POINT ( 'NONE',  ( 35.52699606538937616, -23.08748816067360465, -19.11185354855568619 ) ) ;
#22465 = VERTEX_POINT ( 'NONE', #7662 ) ;
#22466 = CARTESIAN_POINT ( 'NONE',  ( 164.5152310637604671, -9.999999999999998224, -11.28819510263909542 ) ) ;
#22467 = CARTESIAN_POINT ( 'NONE',  ( 10.67100603215144794, 9.034109945373653972, -16.41023209856668785 ) ) ;
#22468 = CARTESIAN_POINT ( 'NONE',  ( 156.1922820468853388, -10.00000000000000178, -4.936203717676158398 ) ) ;
#22469 = CARTESIAN_POINT ( 'NONE',  ( 133.6922820468854241, -4.999999999999981348, -23.73366926340167282 ) ) ;
#22470 = ORIENTED_EDGE ( 'NONE', *, *, #3113, .T. ) ;
#22471 = CARTESIAN_POINT ( 'NONE',  ( 147.2287565553230309, -4.999999999999977796, -29.49038105676659427 ) ) ;
#22472 = ORIENTED_EDGE ( 'NONE', *, *, #11075, .F. ) ;
#22473 = CARTESIAN_POINT ( 'NONE',  ( 12.86851577213266928, 9.516150637207879015, -16.11522534726903899 ) ) ;
#22475 = VECTOR ( 'NONE', #13231, 999.9999999999998863 ) ;
#22474 = CARTESIAN_POINT ( 'NONE',  ( 36.35319451023849524, -20.30668983862152288, -19.44923342519521370 ) ) ;
#22476 = CARTESIAN_POINT ( 'NONE',  ( 22.89472691350227507, 1.279074496056108901, -19.72372301458170796 ) ) ;
#22477 = ORIENTED_EDGE ( 'NONE', *, *, #6746, .F. ) ;
#22478 = LINE ( 'NONE', #18030, #28703 ) ;
#22479 = CARTESIAN_POINT ( 'NONE',  ( 96.45015875629363222, -4.999999999999991118, -70.07514216931596707 ) ) ;
#22480 = CARTESIAN_POINT ( 'NONE',  ( 130.7287565553229456, -4.999999999999983125, 0.5000000000000052180 ) ) ;
#22481 = PRESENTATION_LAYER_ASSIGNMENT (  '', '', ( #24857 ) ) ;
#22482 = CARTESIAN_POINT ( 'NONE',  ( 28.67999647541807207, -5.919990246138143952, -18.25217309140403188 ) ) ;
#22483 = CARTESIAN_POINT ( 'NONE',  ( 27.04162508513615393, -6.753966733322825711, -13.61186222264828771 ) ) ;
#22484 = ORIENTED_EDGE ( 'NONE', *, *, #16733, .T. ) ;
#22485 = PLANE ( 'NONE',  #20564 ) ;
#22486 = DIRECTION ( 'NONE',  ( 0.9510565162951535312, 2.566386769018988816E-16, -0.3090169943749475623 ) ) ;
#22487 = CARTESIAN_POINT ( 'NONE',  ( 153.6922820468854525, -1.999999999999974021, -32.39392330124607611 ) ) ;
#22488 = VECTOR ( 'NONE', #21923, 999.9999999999998863 ) ;
#22489 = DIRECTION ( 'NONE',  ( -0.000000000000000000, -0.000000000000000000, -1.000000000000000000 ) ) ;
#22490 = CARTESIAN_POINT ( 'NONE',  ( -7.999999999999998224, -3.098204225878191664, -4.684209322808124298 ) ) ;
#22491 = AXIS2_PLACEMENT_3D ( 'NONE', #5118, #4666, #11827 ) ;
#22492 = EDGE_CURVE ( 'NONE', #23715, #5737, #22004, .T. ) ;
#22493 = EDGE_CURVE ( 'NONE', #18100, #24253, #17410, .T. ) ;
#22494 = DIRECTION ( 'NONE',  ( 0.000000000000000000, 2.775557561562890735E-17, -1.000000000000000000 ) ) ;
#22495 = CARTESIAN_POINT ( 'NONE',  ( 12.27065153619900961, 7.644304191818388716, -16.55295716654172722 ) ) ;
#22496 = EDGE_CURVE ( 'NONE', #1053, #28447, #3390, .T. ) ;
#22497 = CARTESIAN_POINT ( 'NONE',  ( 12.50226005284522657, 8.571700941790735939, -15.12837371066060221 ) ) ;
#22498 = ADVANCED_FACE ( 'NONE', ( #19552 ), #5975, .T. ) ;
#22499 = CARTESIAN_POINT ( 'NONE',  ( 0.000000000000000000, 0.000000000000000000, -15.00000000000000000 ) ) ;
#22500 = VERTEX_POINT ( 'NONE', #24009 ) ;
#22501 = DIRECTION ( 'NONE',  ( 0.9510565162951536422, 0.000000000000000000, -0.3090169943749475623 ) ) ;
#22502 = DIRECTION ( 'NONE',  ( 1.000000000000000000, 0.000000000000000000, 0.000000000000000000 ) ) ;
#22503 = VERTEX_POINT ( 'NONE', #10390 ) ;
#22504 = CARTESIAN_POINT ( 'NONE',  ( 9.641359250860388030, 17.66885243249017634, -17.90483003768722625 ) ) ;
#22505 = CARTESIAN_POINT ( 'NONE',  ( 159.5152310637604955, -1.999999999999973133, -21.71180489736091346 ) ) ;
#22506 = CARTESIAN_POINT ( 'NONE',  ( 420.0000000000002274, 41.64101615137744972, 14.00000000000000178 ) ) ;
#22507 = LINE ( 'NONE', #1608, #29658 ) ;
#22509 = ORIENTED_EDGE ( 'NONE', *, *, #1042, .F. ) ;
#22508 = CARTESIAN_POINT ( 'NONE',  ( 26.72358035960067824, -3.685970424986596772, -17.59444040205794835 ) ) ;
#22510 = ORIENTED_EDGE ( 'NONE', *, *, #15932, .T. ) ;
#22511 = DIRECTION ( 'NONE',  ( -2.698458740408365879E-16, 1.000000000000000000, 0.000000000000000000 ) ) ;
#22512 = CARTESIAN_POINT ( 'NONE',  ( 12.24516416863347956, 9.516115402270077794, -15.33328367062981279 ) ) ;
#22513 = CARTESIAN_POINT ( 'NONE',  ( 32.45272648307624053, -11.02157468472264412, -17.82583700188536824 ) ) ;
#22514 = CARTESIAN_POINT ( 'NONE',  ( 167.2287565553229172, -1.999999999999971356, -12.16987298107780369 ) ) ;
#22515 = CARTESIAN_POINT ( 'NONE',  ( 24.36497833745277930, -6.082191617938494055, -18.74521747929614435 ) ) ;
#22516 = PLANE ( 'NONE',  #9117 ) ;
#22517 = CARTESIAN_POINT ( 'NONE',  ( 21.82779397375749753, -0.5565768812632180262, -18.88406021698092729 ) ) ;
#22518 = VERTEX_POINT ( 'NONE', #12683 ) ;
#22519 = CARTESIAN_POINT ( 'NONE',  ( 20.00000000000017053, 41.64101615137744972, 12.00000000000000178 ) ) ;
#22520 = ORIENTED_EDGE ( 'NONE', *, *, #27131, .T. ) ;
#22521 = EDGE_LOOP ( 'NONE', ( #285, #29267, #19657, #11841 ) ) ;
#22522 = SURFACE_STYLE_USAGE ( .BOTH. , #18370 ) ;
#22523 = CARTESIAN_POINT ( 'NONE',  ( 15.84550288711180777, 10.06862660282224731, -14.00251831694083826 ) ) ;
#22524 = CARTESIAN_POINT ( 'NONE',  ( 27.48568275346891809, -3.109927088581168952, -18.71928346135984711 ) ) ;
#22525 = ADVANCED_FACE ( 'NONE', ( #15114 ), #24445, .T. ) ;
#22526 = ORIENTED_EDGE ( 'NONE', *, *, #9235, .F. ) ;
#22527 = CARTESIAN_POINT ( 'NONE',  ( 29.72799312938100513, -7.689056491358781997, -15.42978383025728384 ) ) ;
#22528 = DIRECTION ( 'NONE',  ( -2.698458740408365879E-16, 1.000000000000000000, 0.000000000000000000 ) ) ;
#22529 = ORIENTED_EDGE ( 'NONE', *, *, #26, .F. ) ;
#22530 = DIRECTION ( 'NONE',  ( -0.9510565162951536422, -2.566386769018988816E-16, -0.3090169943749472292 ) ) ;
#22531 = CARTESIAN_POINT ( 'NONE',  ( 153.6922820468853388, -10.00000000000000178, -0.6060766987539614181 ) ) ;
#22532 = EDGE_CURVE ( 'NONE', #19023, #20837, #795, .T. ) ;
#22533 = CARTESIAN_POINT ( 'NONE',  ( 132.2287565553230024, -10.00000000000000888, -20.83012701892220164 ) ) ;
#22534 = AXIS2_PLACEMENT_3D ( 'NONE', #21378, #7351, #25821 ) ;
#22535 = CARTESIAN_POINT ( 'NONE',  ( 149.5152310637605524, -1.999999999999975797, -21.71180489736091346 ) ) ;
#22536 = EDGE_CURVE ( 'NONE', #7334, #2624, #3539, .T. ) ;
#22537 = CARTESIAN_POINT ( 'NONE',  ( 24.00126410897001605, -3.753019607378720757, -14.48453144943877113 ) ) ;
#22538 = CARTESIAN_POINT ( 'NONE',  ( 21.44014932938603835, 4.813297736510089742, -15.98289606589226075 ) ) ;
#22539 = CARTESIAN_POINT ( 'NONE',  ( 33.21349783521664278, -10.00660656636812007, -19.57461044683394746 ) ) ;
#22540 = FACE_OUTER_BOUND ( 'NONE', #4111, .T. ) ;
#22541 = CARTESIAN_POINT ( 'NONE',  ( 11.47464782381437587, 9.261287281732329291, -15.86016978468419936 ) ) ;
#22542 = CARTESIAN_POINT ( 'NONE',  ( 5.000000000000000000, 6.123233995736766282E-16, 23.00000000000000000 ) ) ;
#22543 = LINE ( 'NONE', #24374, #26627 ) ;
#22544 = CARTESIAN_POINT ( 'NONE',  ( 13.17827647522021906, 8.595009676161804890, -15.86834059905992511 ) ) ;
#22545 = CARTESIAN_POINT ( 'NONE',  ( 158.6922820468853388, -4.999999999999975131, -9.266330736598359152 ) ) ;
#22546 = ORIENTED_EDGE ( 'NONE', *, *, #3403, .F. ) ;
#22547 = CARTESIAN_POINT ( 'NONE',  ( 131.1922820468854241, -1.999999999999981792, -10.74328820663507322 ) ) ;
#22548 = CARTESIAN_POINT ( 'NONE',  ( 12.50226005284522657, 8.571700941790735939, -15.12837371066060221 ) ) ;
#22549 = EDGE_LOOP ( 'NONE', ( #17718, #9439, #4300, #5656 ) ) ;
#22550 = LINE ( 'NONE', #8638, #13907 ) ;
#22551 = LINE ( 'NONE', #8932, #1026 ) ;
#22552 = AXIS2_PLACEMENT_3D ( 'NONE', #23533, #14655, #7209 ) ;
#22553 = CARTESIAN_POINT ( 'NONE',  ( 164.7287565553228603, -4.999999999999972466, 0.8205080756888000204 ) ) ;
#22554 = ORIENTED_EDGE ( 'NONE', *, *, #1376, .T. ) ;
#22555 = ORIENTED_EDGE ( 'NONE', *, *, #20685, .F. ) ;
#22556 = CARTESIAN_POINT ( 'NONE',  ( 8.945111769380243771, 16.94917547725161810, -17.84906893764549451 ) ) ;
#22557 = CARTESIAN_POINT ( 'NONE',  ( 35.65609946332594404, -19.17501105436304343, -21.36250568352834378 ) ) ;
#22558 = CARTESIAN_POINT ( 'NONE',  ( 19.52525132842032107, 6.402381508982842639, -20.74126646842140431 ) ) ;
#22559 = CARTESIAN_POINT ( 'NONE',  ( 27.15293434934692129, -9.258526923162836653, -12.62629486378885701 ) ) ;
#22560 = CARTESIAN_POINT ( 'NONE',  ( 0.000000000000000000, 0.000000000000000000, -2.450000000000000622 ) ) ;
#22561 = CIRCLE ( 'NONE', #17184, 5.000000000000000888 ) ;
#22562 = FACE_OUTER_BOUND ( 'NONE', #16995, .T. ) ;
#22563 = CIRCLE ( 'NONE', #7918, 2.041999999999999815 ) ;
#22564 = CARTESIAN_POINT ( 'NONE',  ( 171.1922820468853672, -1.999999999999969580, -28.06379628232387802 ) ) ;
#22565 = CARTESIAN_POINT ( 'NONE',  ( 20.30290135898079384, 0.5855005908018823257, -19.57000235946889433 ) ) ;
#22566 = EDGE_CURVE ( 'NONE', #19566, #30087, #10086, .T. ) ;
#22567 = ORIENTED_EDGE ( 'NONE', *, *, #20770, .T. ) ;
#22568 = LINE ( 'NONE', #1666, #7942 ) ;
#22569 = FILL_AREA_STYLE_COLOUR ( '', #13121 ) ;
#22570 = CARTESIAN_POINT ( 'NONE',  ( 0.000000000000000000, 0.000000000000000000, -18.00000000000000000 ) ) ;
#22571 = CARTESIAN_POINT ( 'NONE',  ( 13.11965390131543430, 8.569119222385459977, -15.91506261175275760 ) ) ;
#22572 = CARTESIAN_POINT ( 'NONE',  ( 35.54859390954303677, -21.18451583373416014, -15.55638201429745848 ) ) ;
#22573 = CARTESIAN_POINT ( 'NONE',  ( 12.74802704355670535, 7.622310320333636646, -14.93249076938322162 ) ) ;
#22574 = ORIENTED_EDGE ( 'NONE', *, *, #24912, .F. ) ;
#22575 = VECTOR ( 'NONE', #2704, 1000.000000000000000 ) ;
#22576 = CARTESIAN_POINT ( 'NONE',  ( 27.21278356834291756, -7.014839303453253905, -18.45691071023835761 ) ) ;
#22577 = CARTESIAN_POINT ( 'NONE',  ( 10.35864918915110877, 16.97212501191939538, -17.92015940598198753 ) ) ;
#22578 = DIRECTION ( 'NONE',  ( -0.7071067811865490160, -0.7071067811865460184, 0.000000000000000000 ) ) ;
#22579 = ORIENTED_EDGE ( 'NONE', *, *, #29997, .F. ) ;
#22580 = DIRECTION ( 'NONE',  ( 0.3090169943749475623, 8.338696094058001131E-17, 0.9510565162951536422 ) ) ;
#22581 = DIRECTION ( 'NONE',  ( 0.000000000000000000, -2.775557561562890735E-17, 1.000000000000000000 ) ) ;
#22582 = DIRECTION ( 'NONE',  ( -2.698458740408365879E-16, 1.000000000000000000, 0.000000000000000000 ) ) ;
#22583 = ORIENTED_EDGE ( 'NONE', *, *, #15891, .F. ) ;
#22584 = CARTESIAN_POINT ( 'NONE',  ( 0.000000000000000000, 0.000000000000000000, -5.000000000000000888 ) ) ;
#22585 = ORIENTED_EDGE ( 'NONE', *, *, #1665, .F. ) ;
#22586 = CARTESIAN_POINT ( 'NONE',  ( 13.12362514754451759, 8.570858352459396201, -15.91189866610160841 ) ) ;
#22587 = CARTESIAN_POINT ( 'NONE',  ( 25.07020310977553024, -1.264175079641418398, -16.65545549153034699 ) ) ;
#22588 = CARTESIAN_POINT ( 'NONE',  ( 16.15008960989130671, 4.591438144365319829, -20.60273134265763062 ) ) ;
#22589 = FACE_OUTER_BOUND ( 'NONE', #22160, .T. ) ;
#22590 = DIRECTION ( 'NONE',  ( -0.9510565162951536422, -2.566386769018988323E-16, 0.3090169943749475623 ) ) ;
#22591 = EDGE_CURVE ( 'NONE', #14514, #11139, #19399, .T. ) ;
#22592 = ADVANCED_FACE ( 'NONE', ( #21548 ), #8251, .T. ) ;
#22593 = CARTESIAN_POINT ( 'NONE',  ( 17.36512755686010934, 0.5347363583120325892, -15.24149349723765390 ) ) ;
#22594 = VECTOR ( 'NONE', #20362, 1000.000000000000000 ) ;
#22595 = ORIENTED_EDGE ( 'NONE', *, *, #2177, .F. ) ;
#22596 = PLANE ( 'NONE',  #23700 ) ;
#22597 = DIRECTION ( 'NONE',  ( 1.000000000000000000, 2.698458740408365879E-16, -1.110223024625156540E-16 ) ) ;
#22598 = VERTEX_POINT ( 'NONE', #29213 ) ;
#22599 = VERTEX_POINT ( 'NONE', #2955 ) ;
#22600 = CARTESIAN_POINT ( 'NONE',  ( 174.5152310637603819, -9.999999999999994671, -4.391296821672111328 ) ) ;
#22601 = VECTOR ( 'NONE', #12231, 1000.000000000000000 ) ;
#22602 = CARTESIAN_POINT ( 'NONE',  ( 138.6922820468854525, -4.999999999999980460, -15.07341522555727309 ) ) ;
#22603 = LINE ( 'NONE', #17846, #22899 ) ;
#22604 = ORIENTED_EDGE ( 'NONE', *, *, #8492, .T. ) ;
#22605 = VERTEX_POINT ( 'NONE', #29063 ) ;
#22606 = DIRECTION ( 'NONE',  ( -0.8090169943749474513, -2.183098979609982436E-16, 0.5877852522924731371 ) ) ;
#22607 = CARTESIAN_POINT ( 'NONE',  ( 11.05541533128794107, 17.68942332327241829, -17.91551483529627120 ) ) ;
#22608 = LINE ( 'NONE', #8701, #15572 ) ;
#22609 = ORIENTED_EDGE ( 'NONE', *, *, #13526, .T. ) ;
#22610 = CARTESIAN_POINT ( 'NONE',  ( -20.00000000000017053, 34.64101615137744972, -10.00000000000000000 ) ) ;
#22611 = VECTOR ( 'NONE', #21806, 1000.000000000000000 ) ;
#22612 = CARTESIAN_POINT ( 'NONE',  ( 9.641354186875979337, 17.66887565656821124, -17.90893343548146177 ) ) ;
#22613 = LINE ( 'NONE', #8705, #8795 ) ;
#22614 = CARTESIAN_POINT ( 'NONE',  ( 163.6922820468853388, -1.999999999999972689, -17.92658477444275889 ) ) ;
#22615 = EDGE_LOOP ( 'NONE', ( #28057, #3415, #28586, #10114, #21968 ) ) ;
#22616 = FACE_OUTER_BOUND ( 'NONE', #4451, .T. ) ;
#22617 = ORIENTED_EDGE ( 'NONE', *, *, #1277, .T. ) ;
#22618 = CARTESIAN_POINT ( 'NONE',  ( 10.35864919664826900, 16.97212497753646687, -17.91558149794984445 ) ) ;
#22619 = CARTESIAN_POINT ( 'NONE',  ( 34.63381380623899020, -13.58242311684542081, -20.01117170570581649 ) ) ;
#22620 = CARTESIAN_POINT ( 'NONE',  ( 16.94076125623460527, 0.4124075662712927692, -16.40086227390004936 ) ) ;
#22621 = VERTEX_POINT ( 'NONE', #12233 ) ;
#22622 = ORIENTED_EDGE ( 'NONE', *, *, #19196, .T. ) ;
#22623 = DIRECTION ( 'NONE',  ( -0.8090169943749474513, -2.183098979609982436E-16, -0.5877852522924731371 ) ) ;
#22624 = CARTESIAN_POINT ( 'NONE',  ( -4.000000000000008882, 6.928203230275508773, 0.000000000000000000 ) ) ;
#22625 = DIRECTION ( 'NONE',  ( -0.9510565162951536422, -2.566386769018988323E-16, 0.3090169943749475623 ) ) ;
#22626 = ADVANCED_FACE ( 'NONE', ( #652 ), #26445, .T. ) ;
#22627 = CARTESIAN_POINT ( 'NONE',  ( 28.67543231808702942, -10.82877479041544433, -19.00874469794426602 ) ) ;
#22628 = EDGE_CURVE ( 'NONE', #13085, #17128, #4553, .T. ) ;
#22629 = CARTESIAN_POINT ( 'NONE',  ( 28.63860307613198941, -6.423989724335291918, -15.76775560094196749 ) ) ;
#22630 = ORIENTED_EDGE ( 'NONE', *, *, #27696, .T. ) ;
#22631 = EDGE_CURVE ( 'NONE', #28890, #12774, #18586, .T. ) ;
#22632 = ORIENTED_EDGE ( 'NONE', *, *, #7240, .T. ) ;
#22633 = DIRECTION ( 'NONE',  ( 2.081668171172168119E-15, 0.000000000000000000, -1.000000000000000000 ) ) ;
#22634 = DIRECTION ( 'NONE',  ( 0.000000000000000000, 0.000000000000000000, 1.000000000000000000 ) ) ;
#22635 = AXIS2_PLACEMENT_3D ( 'NONE', #21770, #17040, #21467 ) ;
#22636 = DIRECTION ( 'NONE',  ( 1.000000000000000000, 4.440892098500622217E-16, 0.000000000000000000 ) ) ;
#22637 = CARTESIAN_POINT ( 'NONE',  ( 13.00000000000000178, 0.000000000000000000, 18.00000000000000000 ) ) ;
#22638 = CARTESIAN_POINT ( 'NONE',  ( 167.0152310637604671, -4.999999999999972466, -17.38167787843871182 ) ) ;
#22639 = DIRECTION ( 'NONE',  ( 0.000000000000000000, 0.000000000000000000, 1.000000000000000000 ) ) ;
#22640 = UNCERTAINTY_MEASURE_WITH_UNIT (LENGTH_MEASURE( 1.000000000000000082E-05 ), #18116, 'distance_accuracy_value', 'NONE');
#22641 = CARTESIAN_POINT ( 'NONE',  ( 13.16425014233558954, 7.550783913790151125, -15.87799427043765021 ) ) ;
#22642 = AXIS2_PLACEMENT_3D ( 'NONE', #3103, #24443, #29212 ) ;
#22643 = CARTESIAN_POINT ( 'NONE',  ( 10.33811693838771717, 18.38618951776012267, -17.92279151347708677 ) ) ;
#22644 = CARTESIAN_POINT ( 'NONE',  ( 29.95311431238071975, -11.57681909846818691, -12.96816900313696230 ) ) ;
#22645 = FACE_OUTER_BOUND ( 'NONE', #20437, .T. ) ;
#22646 = DIRECTION ( 'NONE',  ( -1.000000000000000000, 0.000000000000000000, 0.000000000000000000 ) ) ;
#22647 = ORIENTED_EDGE ( 'NONE', *, *, #23954, .T. ) ;
#22648 = CARTESIAN_POINT ( 'NONE',  ( 9.649959050778257108, 17.62941265384766254, -17.56860460898032628 ) ) ;
#22649 = LINE ( 'NONE', #7186, #7693 ) ;
#22650 = LINE ( 'NONE', #8889, #21942 ) ;
#22651 = CARTESIAN_POINT ( 'NONE',  ( 169.5152310637604955, -9.999999999999994671, -30.37205893520531319 ) ) ;
#22653 = ORIENTED_EDGE ( 'NONE', *, *, #13757, .F. ) ;
#22652 = CARTESIAN_POINT ( 'NONE',  ( 25.67262840375075328, -3.322766148301121714, -14.04542551033457798 ) ) ;
#22654 = ORIENTED_EDGE ( 'NONE', *, *, #28493, .F. ) ;
#22655 = FACE_OUTER_BOUND ( 'NONE', #3363, .T. ) ;
#22656 = CARTESIAN_POINT ( 'NONE',  ( 11.05541531668977662, 17.68942339022145305, -21.33333333332589632 ) ) ;
#22657 = CARTESIAN_POINT ( 'NONE',  ( 34.39741479528305490, -17.01287786994462792, -20.00997473120332515 ) ) ;
#22658 = DIRECTION ( 'NONE',  ( -0.000000000000000000, 0.000000000000000000, 1.000000000000000000 ) ) ;
#22659 = CARTESIAN_POINT ( 'NONE',  ( 26.61709978538234012, -3.831456866606135492, -17.85214630790261836 ) ) ;
#22660 = CONICAL_SURFACE ( 'NONE', #7057, 5.000000000000000000, 0.2131563744996336218 ) ;
#22661 = PLANE ( 'NONE',  #9606 ) ;
#22662 = CARTESIAN_POINT ( 'NONE',  ( 21.98307778806466928, -1.383504679822651795, -14.66368364926259460 ) ) ;
#22663 = EDGE_LOOP ( 'NONE', ( #3689, #2013, #18015, #28174, #25968 ) ) ;
#22664 = DIRECTION ( 'NONE',  ( 0.9510565162951535312, 2.566386769018988816E-16, -0.3090169943749475623 ) ) ;
#22665 = VERTEX_POINT ( 'NONE', #13841 ) ;
#22666 = CARTESIAN_POINT ( 'NONE',  ( 26.19910047366428429, -13.48590472426672626, -13.82108881675422829 ) ) ;
#22667 = CARTESIAN_POINT ( 'NONE',  ( 27.65280983889778810, -8.379432582749632985, -19.23476105915534973 ) ) ;
#22668 = ADVANCED_FACE ( 'NONE', ( #16286 ), #4409, .T. ) ;
#22669 = EDGE_CURVE ( 'NONE', #22621, #10540, #11549, .T. ) ;
#22670 = EDGE_CURVE ( 'NONE', #19094, #20748, #20569, .T. ) ;
#22671 = EDGE_CURVE ( 'NONE', #26944, #24422, #20864, .T. ) ;
#22672 = ORIENTED_EDGE ( 'NONE', *, *, #6263, .F. ) ;
#22673 = DIRECTION ( 'NONE',  ( 0.000000000000000000, 0.000000000000000000, -1.000000000000000000 ) ) ;
#22674 = PLANE ( 'NONE',  #22106 ) ;
#22675 = VERTEX_POINT ( 'NONE', #23316 ) ;
#22676 = ORIENTED_EDGE ( 'NONE', *, *, #8799, .T. ) ;
#22677 = DIRECTION ( 'NONE',  ( 0.5000000000000017764, 0.8660254037844375974, 0.000000000000000000 ) ) ;
#22678 = CARTESIAN_POINT ( 'NONE',  ( -17.25000000000017053, 34.64101615137744972, -10.00000000000000000 ) ) ;
#22679 = CARTESIAN_POINT ( 'NONE',  ( 176.1922820468852819, -9.999999999999994671, -13.59645775552055902 ) ) ;
#22680 = VECTOR ( 'NONE', #26910, 1000.000000000000000 ) ;
#22681 = LINE ( 'NONE', #6500, #9677 ) ;
#22682 = CARTESIAN_POINT ( 'NONE',  ( 27.60672911170952304, -4.775276709060196190, -16.23362067418393195 ) ) ;
#22683 = CARTESIAN_POINT ( 'NONE',  ( 19.54522145393098498, 6.247755356217567169, -19.64858106251988801 ) ) ;
#22684 = CARTESIAN_POINT ( 'NONE',  ( 35.26378566547066384, -17.41255297500571331, -21.24391863398521352 ) ) ;
#22685 = CARTESIAN_POINT ( 'NONE',  ( 83.18461569156667679, -4.999999999999994671, 60.43716097570526102 ) ) ;
#22686 = CARTESIAN_POINT ( 'NONE',  ( 12.48484057295006977, 8.564241722236854315, -15.14223913367768759 ) ) ;
#22687 = DIRECTION ( 'NONE',  ( 0.9510565162951536422, 0.000000000000000000, -0.3090169943749475623 ) ) ;
#22688 = CARTESIAN_POINT ( 'NONE',  ( 142.0152310637606092, -1.999999999999978018, -15.61832212156129707 ) ) ;
#22689 = CARTESIAN_POINT ( 'NONE',  ( 13.25994536507779742, 8.631100619704961119, -15.80324905228922994 ) ) ;
#22690 = DIRECTION ( 'NONE',  ( 1.000000000000000000, 2.698458740408365879E-16, -1.110223024625156540E-16 ) ) ;
#22691 = EDGE_LOOP ( 'NONE', ( #8243, #11032, #26639, #4130, #9485, #4731 ) ) ;
#22692 = CYLINDRICAL_SURFACE ( 'NONE', #22722, 5.000000000000000000 ) ;
#22693 = CARTESIAN_POINT ( 'NONE',  ( 12.49860086554322436, 8.570087612320898884, -15.13128986298120537 ) ) ;
#22694 = VERTEX_POINT ( 'NONE', #27789 ) ;
#22695 = DIRECTION ( 'NONE',  ( 0.9510565162951535312, 2.566386769018988816E-16, -0.3090169943749475623 ) ) ;
#22696 = FACE_OUTER_BOUND ( 'NONE', #10001, .T. ) ;
#22697 = ORIENTED_EDGE ( 'NONE', *, *, #13691, .T. ) ;
#22698 = CARTESIAN_POINT ( 'NONE',  ( -7.806255641895631925E-14, -4.618802153517044928, -2.092734410091829034 ) ) ;
#22699 = VERTEX_POINT ( 'NONE', #17709 ) ;
#22700 = CARTESIAN_POINT ( 'NONE',  ( 13.38095672321806795, 7.626547943635540783, -15.70680086385617358 ) ) ;
#22701 = CARTESIAN_POINT ( 'NONE',  ( 34.21167138940940333, -12.68596085309027899, -20.92588972839351058 ) ) ;
#22702 = CARTESIAN_POINT ( 'NONE',  ( 20.32371149932726695, 7.300285753667301591, -19.85501735805741319 ) ) ;
#22703 = AXIS2_PLACEMENT_3D ( 'NONE', #9937, #5526, #19249 ) ;
#22704 = EDGE_CURVE ( 'NONE', #12785, #13256, #8961, .T. ) ;
#22705 = CARTESIAN_POINT ( 'NONE',  ( 17.63088349262504551, 4.212901655933308120, -18.95607689789294170 ) ) ;
#22706 = DIRECTION ( 'NONE',  ( 1.000000000000000000, 2.698458740408365879E-16, -1.779203565104417375E-16 ) ) ;
#22707 = AXIS2_PLACEMENT_3D ( 'NONE', #26838, #28721, #21056 ) ;
#22708 = ADVANCED_FACE ( 'NONE', ( #23031 ), #9258, .T. ) ;
#22709 = FACE_OUTER_BOUND ( 'NONE', #14345, .T. ) ;
#22710 = ADVANCED_FACE ( 'NONE', ( #6997 ), #18277, .T. ) ;
#22711 = CARTESIAN_POINT ( 'NONE',  ( 23.15972007162554291, -8.148303969466700991, -13.79129035937103431 ) ) ;
#22712 = ORIENTED_EDGE ( 'NONE', *, *, #18596, .F. ) ;
#22713 = CARTESIAN_POINT ( 'NONE',  ( 18.70776367089402825, -5.000000000000012434, -57.57657626727587541 ) ) ;
#22714 = AXIS2_PLACEMENT_3D ( 'NONE', #3922, #13219, #17196 ) ;
#22716 = ORIENTED_EDGE ( 'NONE', *, *, #3135, .T. ) ;
#22715 =( NAMED_UNIT ( * ) PLANE_ANGLE_UNIT ( ) SI_UNIT ( $, .RADIAN. ) );
#22717 = CARTESIAN_POINT ( 'NONE',  ( -8.000000000000000000, 3.871967595402115769, -0.4989386132324554746 ) ) ;
#22718 = CARTESIAN_POINT ( 'NONE',  ( 93.42506966527585632, -4.999999999999992006, 67.87728629368646693 ) ) ;
#22719 = VECTOR ( 'NONE', #29146, 1000.000000000000000 ) ;
#22720 = LINE ( 'NONE', #15826, #5360 ) ;
#22721 = CARTESIAN_POINT ( 'NONE',  ( 32.48803055552120611, -10.90163289162770432, -13.69202896798154256 ) ) ;
#22722 = AXIS2_PLACEMENT_3D ( 'NONE', #13368, #20678, #11231 ) ;
#22723 = CARTESIAN_POINT ( 'NONE',  ( 10.67054149815029618, 9.036200773601834157, -16.41042721873081689 ) ) ;
#22724 = ORIENTED_EDGE ( 'NONE', *, *, #18758, .F. ) ;
#22725 = VECTOR ( 'NONE', #784, 1000.000000000000000 ) ;
#22726 = CARTESIAN_POINT ( 'NONE',  ( 25.79824969357368047, -12.24460132778619226, -15.92960863319586906 ) ) ;
#22727 = CARTESIAN_POINT ( 'NONE',  ( 139.7287565553230309, -4.999999999999980460, -16.49999999999999289 ) ) ;
#22728 = CARTESIAN_POINT ( 'NONE',  ( 10.35864918915110877, 16.97212501191939538, -19.66666666666842644 ) ) ;
#22729 = FACE_BOUND ( 'NONE', #24303, .T. ) ;
#22730 = ORIENTED_EDGE ( 'NONE', *, *, #15163, .T. ) ;
#22731 = CARTESIAN_POINT ( 'NONE',  ( 149.5152310637605240, -4.999999999999976907, -1.659952520591373703E-14 ) ) ;
#22732 = DIRECTION ( 'NONE',  ( 0.000000000000000000, 0.000000000000000000, 1.000000000000000000 ) ) ;
#22733 = DIRECTION ( 'NONE',  ( 0.000000000000000000, 0.000000000000000000, 1.000000000000000000 ) ) ;
#22734 = ORIENTED_EDGE ( 'NONE', *, *, #14057, .T. ) ;
#22735 = CARTESIAN_POINT ( 'NONE',  ( -8.000000000000001776, -4.336808689942017736E-15, 0.000000000000000000 ) ) ;
#22736 = ORIENTED_EDGE ( 'NONE', *, *, #3117, .F. ) ;
#22737 = CARTESIAN_POINT ( 'NONE',  ( 13.11714404544056656, 8.568033937426095648, -15.91706119101506545 ) ) ;
#22738 = CARTESIAN_POINT ( 'NONE',  ( 19.88518670226333995, -2.923732859705698850, -17.09422515135678111 ) ) ;
#22739 = CARTESIAN_POINT ( 'NONE',  ( 17.31888479101057143, -0.09998177899580885930, -18.75936487049801116 ) ) ;
#22740 = VECTOR ( 'NONE', #2100, 1000.000000000000000 ) ;
#22741 = DIRECTION ( 'NONE',  ( -1.000000000000000000, 0.000000000000000000, -0.000000000000000000 ) ) ;
#22742 = DIRECTION ( 'NONE',  ( -2.698458740408365879E-16, 1.000000000000000000, 0.000000000000000000 ) ) ;
#22743 = EDGE_CURVE ( 'NONE', #28787, #5689, #20711, .T. ) ;
#22744 = VECTOR ( 'NONE', #22958, 1000.000000000000000 ) ;
#22745 = CARTESIAN_POINT ( 'NONE',  ( 17.33713706444265412, 0.9871066061555996418, -18.79342181739402307 ) ) ;
#22746 = PRESENTATION_LAYER_ASSIGNMENT (  '', '', ( #7166 ) ) ;
#22747 = LINE ( 'NONE', #22287, #18809 ) ;
#22748 = LINE ( 'NONE', #11425, #6459 ) ;
#22749 = ORIENTED_EDGE ( 'NONE', *, *, #23845, .T. ) ;
#22750 = LINE ( 'NONE', #15861, #1470 ) ;
#22751 = CARTESIAN_POINT ( 'NONE',  ( 32.89062095351589932, -11.25267498498577723, -18.96775996542842435 ) ) ;
#22752 = DIRECTION ( 'NONE',  ( -0.9510565162951536422, -2.566386769018988323E-16, 0.3090169943749475623 ) ) ;
#22753 = ORIENTED_EDGE ( 'NONE', *, *, #8980, .F. ) ;
#22754 = EDGE_LOOP ( 'NONE', ( #24618, #2158, #10931, #20927 ) ) ;
#22755 = DIRECTION ( 'NONE',  ( 0.9510565162951535312, 2.566386769018988816E-16, -0.3090169943749475623 ) ) ;
#22756 = VECTOR ( 'NONE', #22664, 1000.000000000000000 ) ;
#22757 = CARTESIAN_POINT ( 'NONE',  ( 17.12833724908345800, 9.171387755021909172, -19.38714867094073213 ) ) ;
#22758 = CARTESIAN_POINT ( 'NONE',  ( 12.78959314398258940, 9.756708335562493062, -14.89936416525698526 ) ) ;
#22759 = CARTESIAN_POINT ( 'NONE',  ( 33.75544676243647757, -14.12885555826641593, -19.81592319558764004 ) ) ;
#22760 = EDGE_CURVE ( 'NONE', #11002, #29409, #21024, .T. ) ;
#22761 = VERTEX_POINT ( 'NONE', #6851 ) ;
#22762 = ORIENTED_EDGE ( 'NONE', *, *, #30163, .F. ) ;
#22763 = CIRCLE ( 'NONE', #26679, 129.8897274573438381 ) ;
#22764 = CARTESIAN_POINT ( 'NONE',  ( 143.6922820468853956, -4.999999999999979572, -0.6060766987539614181 ) ) ;
#22765 = PRODUCT_RELATED_PRODUCT_CATEGORY ( 'part', '', ( #1074 ) ) ;
#22766 = AXIS2_PLACEMENT_3D ( 'NONE', #1111, #3104, #12833 ) ;
#22767 = CARTESIAN_POINT ( 'NONE',  ( 12.75568354342045119, 7.625663700289499580, -14.92639070443840588 ) ) ;
#22768 = LINE ( 'NONE', #17415, #23452 ) ;
#22769 = CARTESIAN_POINT ( 'NONE',  ( 157.2287565553229456, -10.00000000000000000, -12.16987298107780369 ) ) ;
#22770 = VERTEX_POINT ( 'NONE', #16145 ) ;
#22771 = LINE ( 'NONE', #22926, #24210 ) ;
#22772 = ORIENTED_EDGE ( 'NONE', *, *, #16902, .F. ) ;
#22773 = CARTESIAN_POINT ( 'NONE',  ( 12.86785267122296794, 9.515866005961482799, -16.11575320936711364 ) ) ;
#22774 = CARTESIAN_POINT ( 'NONE',  ( 34.36632712588347260, -12.38074715364594347, -19.93031689919964222 ) ) ;
#22775 = CARTESIAN_POINT ( 'NONE',  ( 25.21413058671614849, -1.115224416820481457, -18.44856734933592080 ) ) ;
#22776 = PRODUCT_DEFINITION_SHAPE ( 'NONE', 'NONE',  #28218 ) ;
#22777 = ORIENTED_EDGE ( 'NONE', *, *, #11476, .T. ) ;
#22778 = CARTESIAN_POINT ( 'NONE',  ( 162.0152310637605524, -9.999999999999998224, -32.93883019725009120 ) ) ;
#22779 = CARTESIAN_POINT ( 'NONE',  ( 167.2287565553229172, -9.999999999999998224, -12.16987298107780369 ) ) ;
#22780 = CARTESIAN_POINT ( 'NONE',  ( 26.95082352492110189, -12.40836276091286194, -17.97502949936508898 ) ) ;
#22781 = CARTESIAN_POINT ( 'NONE',  ( 26.47302276827314671, -6.985584592454325836, -13.42065591321591711 ) ) ;
#22782 = VECTOR ( 'NONE', #23550, 1000.000000000000000 ) ;
#22783 = ORIENTED_EDGE ( 'NONE', *, *, #18205, .T. ) ;
#22784 = DIRECTION ( 'NONE',  ( -1.387778780781445676E-16, 0.000000000000000000, -1.000000000000000000 ) ) ;
#22785 = CIRCLE ( 'NONE', #849, 7.000000000000006217 ) ;
#22786 = FACE_OUTER_BOUND ( 'NONE', #4415, .T. ) ;
#22787 = DIRECTION ( 'NONE',  ( 1.000000000000000000, 4.440892098500622217E-16, 0.000000000000000000 ) ) ;
#22788 = LINE ( 'NONE', #11772, #1704 ) ;
#22789 = CARTESIAN_POINT ( 'NONE',  ( 10.33811693838771717, 18.38618951776012267, -17.98596209335946128 ) ) ;
#22790 = DIRECTION ( 'NONE',  ( -1.110223024625156540E-16, 0.000000000000000000, -1.000000000000000000 ) ) ;
#22791 = ADVANCED_FACE ( 'NONE', ( #25461 ), #2430, .T. ) ;
#22792 = EDGE_CURVE ( 'NONE', #23986, #7041, #6125, .T. ) ;
#22793 = EDGE_LOOP ( 'NONE', ( #2740, #14339 ) ) ;
#22794 = LINE ( 'NONE', #1902, #23727 ) ;
#22795 = ORIENTED_EDGE ( 'NONE', *, *, #22381, .T. ) ;
#22796 = CARTESIAN_POINT ( 'NONE',  ( 9.641350810849047548, 17.66889113945805789, -17.97192418671891190 ) ) ;
#22797 = EDGE_CURVE ( 'NONE', #17495, #29391, #9413, .T. ) ;
#22798 = VECTOR ( 'NONE', #19371, 1000.000000000000000 ) ;
#22799 = LINE ( 'NONE', #27977, #4304 ) ;
#22800 = CARTESIAN_POINT ( 'NONE',  ( 18.80816768961129881, 6.772028514247487863, -18.23967922641782380 ) ) ;
#22801 = LINE ( 'NONE', #27419, #28333 ) ;
#22802 = CARTESIAN_POINT ( 'NONE',  ( 0.000000000000000000, 1.178949249685215417, -2.042000000000002036 ) ) ;
#22803 = EDGE_CURVE ( 'NONE', #29492, #3119, #2724, .T. ) ;
#22805 = VERTEX_POINT ( 'NONE', #20010 ) ;
#22804 = CARTESIAN_POINT ( 'NONE',  ( 23.77086030874127687, -7.150112426529108944, -14.59934731766091431 ) ) ;
#22806 = VERTEX_POINT ( 'NONE', #3841 ) ;
#22807 = CARTESIAN_POINT ( 'NONE',  ( 4.000000000000000000, 0.000000000000000000, -2.450000000000000622 ) ) ;
#22808 = CARTESIAN_POINT ( 'NONE',  ( 12.46291758456249354, 9.612344561400664844, -15.15973035232449462 ) ) ;
#22809 = ORIENTED_EDGE ( 'NONE', *, *, #11652, .T. ) ;
#22810 = CIRCLE ( 'NONE', #26234, 3.000000000000002665 ) ;
#22811 = CARTESIAN_POINT ( 'NONE',  ( 35.54859390953724585, -22.18451583373416014, -17.99055332684694974 ) ) ;
#22812 = FACE_OUTER_BOUND ( 'NONE', #20275, .T. ) ;
#22813 = CARTESIAN_POINT ( 'NONE',  ( 21.16681283796276603, -5.103637247178538061, -17.00692323485822754 ) ) ;
#22814 = FACE_OUTER_BOUND ( 'NONE', #24432, .T. ) ;
#22815 = CARTESIAN_POINT ( 'NONE',  ( 23.33644427035094537, 1.513498076802863190, -16.07814869553001103 ) ) ;
#22816 = ORIENTED_EDGE ( 'NONE', *, *, #20076, .F. ) ;
#22817 = LINE ( 'NONE', #20804, #1815 ) ;
#22818 = CIRCLE ( 'NONE', #15014, 0.5000000000000004441 ) ;
#22819 = SHAPE_REPRESENTATION ( 'Pedal Return Coil Spring', ( #13190 ), #21465 ) ;
#22820 = CARTESIAN_POINT ( 'NONE',  ( 18.00441060066494003, 9.543425513107552050, -19.87907960298149490 ) ) ;
#22821 = CARTESIAN_POINT ( 'NONE',  ( 27.90801785101615096, -12.26699769840798204, -14.39122685649866717 ) ) ;
#22822 = ORIENTED_EDGE ( 'NONE', *, *, #12331, .T. ) ;
#22823 = VERTEX_POINT ( 'NONE', #13134 ) ;
#22824 = DIRECTION ( 'NONE',  ( 1.110223024625156540E-16, 2.995891024602366092E-32, 1.000000000000000000 ) ) ;
#22825 = VECTOR ( 'NONE', #13654, 1000.000000000000000 ) ;
#22826 = LINE ( 'NONE', #18380, #25038 ) ;
#22827 = EDGE_LOOP ( 'NONE', ( #21695, #16358, #25282, #30170 ) ) ;
#22828 = DIRECTION ( 'NONE',  ( -0.9510565162951536422, 0.000000000000000000, -0.3090169943749472292 ) ) ;
#22829 = AXIS2_PLACEMENT_3D ( 'NONE', #29826, #27207, #24890 ) ;
#22830 = DIRECTION ( 'NONE',  ( -2.698458740408365879E-16, 1.000000000000000000, 0.000000000000000000 ) ) ;
#22831 = CARTESIAN_POINT ( 'NONE',  ( 167.2287565553229456, -9.999999999999998224, -20.83012701892220520 ) ) ;
#22832 = CARTESIAN_POINT ( 'NONE',  ( 6.686525924292798351, -5.377136764700183313, -0.3167204509598521289 ) ) ;
#22833 = CARTESIAN_POINT ( 'NONE',  ( 25.04368804655567970, -3.332730676350641463, -14.85212872609148427 ) ) ;
#22834 = CARTESIAN_POINT ( 'NONE',  ( 16.95656709563420250, 3.789241241613106048, -19.64973185778705655 ) ) ;
#22835 = EDGE_CURVE ( 'NONE', #26603, #27706, #9511, .T. ) ;
#22837 = ORIENTED_EDGE ( 'NONE', *, *, #6479, .T. ) ;
#22836 = CARTESIAN_POINT ( 'NONE',  ( 34.19383894405228830, -12.60584912221051290, -20.92049940795970997 ) ) ;
#22838 = DIRECTION ( 'NONE',  ( 0.000000000000000000, 0.000000000000000000, -1.000000000000000000 ) ) ;
#22839 = CARTESIAN_POINT ( 'NONE',  ( 11.47257016429183452, 9.270685755423764718, -15.86103888016343255 ) ) ;
#22840 = EDGE_CURVE ( 'NONE', #12109, #4141, #21625, .T. ) ;
#22841 = DIRECTION ( 'NONE',  ( -0.9510565162951536422, -2.566386769018988816E-16, -0.3090169943749472292 ) ) ;
#22842 = PLANE ( 'NONE',  #10489 ) ;
#22843 = ADVANCED_FACE ( 'NONE', ( #19183 ), #21170, .T. ) ;
#22844 = CARTESIAN_POINT ( 'NONE',  ( 9.663058643182488083, 16.24943526668553062, -17.89776827055807118 ) ) ;
#22845 = LINE ( 'NONE', #4072, #23411 ) ;
#22846 = EDGE_LOOP ( 'NONE', ( #30130, #9853 ) ) ;
#22847 = CARTESIAN_POINT ( 'NONE',  ( 80.33489972152645464, -4.999999999999995559, 58.36672113073498736 ) ) ;
#22848 = CARTESIAN_POINT ( 'NONE',  ( 11.92109019680886206, 8.606374460406147620, -15.56934379943068336 ) ) ;
#22849 = ORIENTED_EDGE ( 'NONE', *, *, #24493, .F. ) ;
#22850 = DIRECTION ( 'NONE',  ( -2.698458740408365879E-16, 1.000000000000000000, 0.000000000000000000 ) ) ;
#22851 = CARTESIAN_POINT ( 'NONE',  ( 36.04859390953723874, -22.18451583373416014, -15.00000000000000000 ) ) ;
#22852 = CARTESIAN_POINT ( 'NONE',  ( 175.7287565553229456, -9.999999999999994671, -30.76635726929469783 ) ) ;
#22853 = ORIENTED_EDGE ( 'NONE', *, *, #13280, .T. ) ;
#22854 = CARTESIAN_POINT ( 'NONE',  ( 9.111692801717447665, 16.18521362881060455, -17.05508072787638696 ) ) ;
#22855 = CARTESIAN_POINT ( 'NONE',  ( 33.26197456417788345, -12.91194637099222575, -20.70907993653955970 ) ) ;
#22856 = AXIS2_PLACEMENT_3D ( 'NONE', #596, #21634, #12925 ) ;
#22857 = CARTESIAN_POINT ( 'NONE',  ( 18.26618351132839280, 3.382507019981081164, -13.19753224271465797 ) ) ;
#22858 = CARTESIAN_POINT ( 'NONE',  ( 18.30550780621970475, 8.505200139115956404, -19.80988581799093140 ) ) ;
#22859 = CARTESIAN_POINT ( 'NONE',  ( 137.0152310637605808, -4.999999999999980460, -34.70218595412750773 ) ) ;
#22860 = CARTESIAN_POINT ( 'NONE',  ( 23.45579420008465732, -3.438291973250592992, -12.29892528769388349 ) ) ;
#22861 = AXIS2_PLACEMENT_3D ( 'NONE', #1937, #15790, #18387 ) ;
#22862 = ORIENTED_EDGE ( 'NONE', *, *, #1075, .T. ) ;
#22863 = FACE_OUTER_BOUND ( 'NONE', #22434, .T. ) ;
#22864 = ORIENTED_EDGE ( 'NONE', *, *, #26709, .F. ) ;
#22865 = CARTESIAN_POINT ( 'NONE',  ( 153.6922820468854525, -10.00000000000000000, -32.39392330124607611 ) ) ;
#22866 = PLANE ( 'NONE',  #21620 ) ;
#22867 = LINE ( 'NONE', #15979, #26324 ) ;
#22868 = CARTESIAN_POINT ( 'NONE',  ( 33.90312036197754963, -11.11655558909185615, -17.69153855583423862 ) ) ;
#22869 = VECTOR ( 'NONE', #17880, 999.9999999999998863 ) ;
#22870 = ORIENTED_EDGE ( 'NONE', *, *, #17039, .F. ) ;
#22871 = CARTESIAN_POINT ( 'NONE',  ( 10.67335300198236148, 9.023663108408856104, -16.40923739229002010 ) ) ;
#22872 = ORIENTED_EDGE ( 'NONE', *, *, #13962, .F. ) ;
#22873 = EDGE_CURVE ( 'NONE', #14794, #23543, #429, .T. ) ;
#22874 = EDGE_CURVE ( 'NONE', #22770, #11670, #12007, .T. ) ;
#22875 = CARTESIAN_POINT ( 'NONE',  ( 26.87449084144840938, -11.88902188497427481, -13.49525739704605343 ) ) ;
#22876 = DIRECTION ( 'NONE',  ( 0.5877852522924731371, 0.000000000000000000, 0.8090169943749474513 ) ) ;
#22877 = ADVANCED_FACE ( 'NONE', ( #2722 ), #14739, .T. ) ;
#22878 = CARTESIAN_POINT ( 'NONE',  ( 10.36430886937160167, 16.94616899698690204, -17.73806594831300032 ) ) ;
#22879 = DIRECTION ( 'NONE',  ( 1.000000000000000000, 2.698458740408365879E-16, -1.110223024625156540E-16 ) ) ;
#22880 = AXIS2_PLACEMENT_3D ( 'NONE', #17436, #22331, #8575 ) ;
#22881 = EDGE_CURVE ( 'NONE', #29503, #10414, #18883, .T. ) ;
#22882 = CARTESIAN_POINT ( 'NONE',  ( 0.2500000000000002220, 0.000000000000000000, 4.000000000000000000 ) ) ;
#22883 = CLOSED_SHELL ( 'NONE', ( #22424, #1410, #29085, #25934, #13478, #4199, #8620, #1477, #21305, #8322, #13224, #30024, #1038, #4099, #20000, #10975, #22592, #22946, #7368, #17372, #18653, #2716, #28800, #8068, #5466, #29923, #5931, #26432, #5716, #6019, #1687, #14235, #16660, #20545, #17994, #15555, #22108, #18797, #5473, #20204, #16136, #683 ) ) ;
#22884 = EDGE_LOOP ( 'NONE', ( #12766, #11298, #8183, #29064 ) ) ;
#22885 = CARTESIAN_POINT ( 'NONE',  ( 162.2287565553229172, -4.999999999999974243, -12.16987298107780013 ) ) ;
#22886 = CARTESIAN_POINT ( 'NONE',  ( 12.50076791318051761, 8.571041463825640250, -15.12956297801270900 ) ) ;
#22888 = ORIENTED_EDGE ( 'NONE', *, *, #10771, .F. ) ;
#22887 = DIRECTION ( 'NONE',  ( 0.3090169943749475623, 8.338696094058001131E-17, 0.9510565162951536422 ) ) ;
#22889 = ORIENTED_EDGE ( 'NONE', *, *, #23593, .F. ) ;
#22890 = DIRECTION ( 'NONE',  ( -2.698458740408365879E-16, 1.000000000000000000, 0.000000000000000000 ) ) ;
#22891 = VERTEX_POINT ( 'NONE', #12455 ) ;
#22892 = CARTESIAN_POINT ( 'NONE',  ( 17.47275436513300662, 10.49281628697410262, -12.44556591811621082 ) ) ;
#22893 = ORIENTED_EDGE ( 'NONE', *, *, #3678, .T. ) ;
#22894 = CARTESIAN_POINT ( 'NONE',  ( 17.31888479101057143, -0.09998177899580885930, -18.75936487049801116 ) ) ;
#22895 = CARTESIAN_POINT ( 'NONE',  ( 24.88259999727891625, -1.109419405293186944, -15.69091174474707451 ) ) ;
#22896 = CARTESIAN_POINT ( 'NONE',  ( 19.54218497767158169, 4.227554098413554229, -14.22708607227295730 ) ) ;
#22897 = LINE ( 'NONE', #27362, #28718 ) ;
#22898 = CARTESIAN_POINT ( 'NONE',  ( 6.941579719855231367, -5.000000000000015987, 21.36398562578804317 ) ) ;
#22899 = VECTOR ( 'NONE', #22752, 999.9999999999998863 ) ;
#22900 = CARTESIAN_POINT ( 'NONE',  ( 17.18819971663578272, 0.8441372818425427749, -18.45219435416397502 ) ) ;
#22901 = ORIENTED_EDGE ( 'NONE', *, *, #20651, .F. ) ;
#22902 = VECTOR ( 'NONE', #10490, 1000.000000000000000 ) ;
#22903 = PLANE ( 'NONE',  #30118 ) ;
#22904 = CARTESIAN_POINT ( 'NONE',  ( 174.5152310637604103, -9.999999999999994671, -2.627941064794695691 ) ) ;
#22905 = ORIENTED_EDGE ( 'NONE', *, *, #1454, .T. ) ;
#22906 = CARTESIAN_POINT ( 'NONE',  ( 10.35864918915110877, 16.97212501191939538, -17.91796598306941135 ) ) ;
#22907 = DIRECTION ( 'NONE',  ( 0.000000000000000000, 0.000000000000000000, 1.000000000000000000 ) ) ;
#22908 = CARTESIAN_POINT ( 'NONE',  ( 129.5152310637605808, -10.00000000000000888, -11.28819510263909187 ) ) ;
#22909 = ORIENTED_EDGE ( 'NONE', *, *, #8956, .T. ) ;
#22910 = ORIENTED_EDGE ( 'NONE', *, *, #20169, .T. ) ;
#22911 = EDGE_CURVE ( 'NONE', #20344, #19263, #16751, .T. ) ;
#22912 = LINE ( 'NONE', #30131, #28069 ) ;
#22913 = CARTESIAN_POINT ( 'NONE',  ( 17.08157517049449581, 7.460725202527481947, -14.57009041681831896 ) ) ;
#22914 = CARTESIAN_POINT ( 'NONE',  ( 11.40579136381300174, 16.08255417555669453, -16.73093107180499928 ) ) ;
#22915 = CARTESIAN_POINT ( 'NONE',  ( 35.54859390953724585, -22.18451583373416014, -16.11276402859391865 ) ) ;
#22916 = EDGE_CURVE ( 'NONE', #28553, #5044, #23569, .T. ) ;
#22917 = VECTOR ( 'NONE', #25787, 1000.000000000000000 ) ;
#22918 = ORIENTED_EDGE ( 'NONE', *, *, #16833, .T. ) ;
#22919 = CARTESIAN_POINT ( 'NONE',  ( 13.15390973649967599, 8.859676595473322536, -14.60899741038990562 ) ) ;
#22920 = VECTOR ( 'NONE', #21092, 999.9999999999998863 ) ;
#22921 = CARTESIAN_POINT ( 'NONE',  ( 12.81042928357508970, 7.649856678006609734, -14.88275739421262855 ) ) ;
#22922 = DIRECTION ( 'NONE',  ( -0.8090169943749474513, -2.183098979609982436E-16, -0.5877852522924731371 ) ) ;
#22923 = DIRECTION ( 'NONE',  ( 1.000000000000000000, 0.000000000000000000, 0.000000000000000000 ) ) ;
#22924 = VECTOR ( 'NONE', #12979, 1000.000000000000000 ) ;
#22925 = ORIENTED_EDGE ( 'NONE', *, *, #22422, .F. ) ;
#22926 = CARTESIAN_POINT ( 'NONE',  ( -4.000000000000005329, 2.309401076758490934, -2.450000000000000178 ) ) ;
#22927 = ORIENTED_EDGE ( 'NONE', *, *, #18210, .T. ) ;
#22928 = CARTESIAN_POINT ( 'NONE',  ( 13.41286507499157388, 9.756708335562493062, -15.68136934427840856 ) ) ;
#22929 = CARTESIAN_POINT ( 'NONE',  ( 33.01527616964045109, -10.33189599206409959, -17.18388710919138873 ) ) ;
#22930 = CARTESIAN_POINT ( 'NONE',  ( 26.47511176763426377, -7.718147522161595830, -18.64721581247919602 ) ) ;
#22931 = ORIENTED_EDGE ( 'NONE', *, *, #27554, .T. ) ;
#22932 = CARTESIAN_POINT ( 'NONE',  ( 152.2287565553229456, -1.999999999999975797, -3.509618943233403510 ) ) ;
#22933 = CARTESIAN_POINT ( 'NONE',  ( 8.295003646061877234, -5.000000000000015099, 25.52939616229333097 ) ) ;
#22934 = VECTOR ( 'NONE', #1449, 1000.000000000000000 ) ;
#22935 =( NAMED_UNIT ( * ) SI_UNIT ( $, .STERADIAN. ) SOLID_ANGLE_UNIT ( ) );
#22936 = CARTESIAN_POINT ( 'NONE',  ( 30.62762753239542590, -8.735908549479720620, -17.37160549233551876 ) ) ;
#22937 = CIRCLE ( 'NONE', #9746, 0.2000000000000000944 ) ;
#22938 = CARTESIAN_POINT ( 'NONE',  ( 23.31633574299079825, -8.368445843159939557, -15.61931793633953980 ) ) ;
#22939 = ORIENTED_EDGE ( 'NONE', *, *, #21161, .F. ) ;
#22940 = ADVANCED_FACE ( 'NONE', ( #10015 ), #16596, .T. ) ;
#22941 = LINE ( 'NONE', #23226, #12290 ) ;
#22942 = CARTESIAN_POINT ( 'NONE',  ( -16.00000000000017053, 34.64101615137744972, 4.999999999999998224 ) ) ;
#22943 = DIRECTION ( 'NONE',  ( 1.000000000000000000, 2.698458740408365879E-16, -1.110223024625156540E-16 ) ) ;
#22944 = CARTESIAN_POINT ( 'NONE',  ( 8.000000000000010658, 3.871967595402145967, -0.4989386132324691303 ) ) ;
#22945 = UNCERTAINTY_MEASURE_WITH_UNIT (LENGTH_MEASURE( 1.000000000000000082E-05 ), #3412, 'distance_accuracy_value', 'NONE');
#22946 = ADVANCED_FACE ( 'NONE', ( #28688, #16440, #4999 ), #28539, .F. ) ;
#22947 = CARTESIAN_POINT ( 'NONE',  ( 15.61762486822808604, 9.948436389806387226, -12.64537296286936829 ) ) ;
#22948 = CARTESIAN_POINT ( 'NONE',  ( 28.67543231808702942, -10.82877479041544433, -19.00874469794426602 ) ) ;
#22949 = CARTESIAN_POINT ( 'NONE',  ( 133.7287565553229172, -9.999999999999991118, -41.50000000000000000 ) ) ;
#22950 = VERTEX_POINT ( 'NONE', #5305 ) ;
#22951 = AXIS2_PLACEMENT_3D ( 'NONE', #25504, #11594, #4594 ) ;
#22952 = CARTESIAN_POINT ( 'NONE',  ( 9.641350810849047548, 17.66889113945805789, -19.66666666666842644 ) ) ;
#22953 = CARTESIAN_POINT ( 'NONE',  ( 16.71823672545656336, 7.456161109308904855, -19.47106720222115683 ) ) ;
#22954 = CARTESIAN_POINT ( 'NONE',  ( 153.6922820468854241, -10.00000000000000000, -26.58683881228715862 ) ) ;
#22955 = FACE_OUTER_BOUND ( 'NONE', #8111, .T. ) ;
#22957 = ORIENTED_EDGE ( 'NONE', *, *, #18656, .T. ) ;
#22956 = CARTESIAN_POINT ( 'NONE',  ( 24.36497833745277930, -6.082191617938494055, -18.74521747929614435 ) ) ;
#22958 = DIRECTION ( 'NONE',  ( -1.110223024625156540E-16, 0.000000000000000000, -1.000000000000000000 ) ) ;
#22959 = CARTESIAN_POINT ( 'NONE',  ( 11.05541531668977662, 17.68942339022145305, -17.94384837343789130 ) ) ;
#22960 = COLOUR_RGB ( '', 0.40784314, 0.44705882, 0.49803922) ;
#22961 = CARTESIAN_POINT ( 'NONE',  ( 33.54145741815126058, -13.16751478770765793, -19.75123935038191192 ) ) ;
#22962 = DIRECTION ( 'NONE',  ( 0.000000000000000000, 0.000000000000000000, -1.000000000000000000 ) ) ;
#22963 = VERTEX_POINT ( 'NONE', #9713 ) ;
#22964 = CARTESIAN_POINT ( 'NONE',  ( 24.81358459371387326, -5.676498915796258871, -18.90393244824272756 ) ) ;
#22965 = DIRECTION ( 'NONE',  ( 0.5877852522924731371, 1.586114251531760728E-16, -0.8090169943749474513 ) ) ;
#22966 = CARTESIAN_POINT ( 'NONE',  ( 22.60637541839240683, -1.101515789306901194, -14.68923631892221948 ) ) ;
#22967 = EDGE_LOOP ( 'NONE', ( #13884, #10456, #28648, #8514 ) ) ;
#22968 = DIRECTION ( 'NONE',  ( -0.9510565162951536422, 0.000000000000000000, -0.3090169943749472292 ) ) ;
#22969 = FILL_AREA_STYLE ('',( #8905 ) ) ;
#22970 = CARTESIAN_POINT ( 'NONE',  ( 16.02150382621726976, 6.204807860950024789, -14.00014022580063155 ) ) ;
#22971 = CARTESIAN_POINT ( 'NONE',  ( 25.78329585330208218, -10.67969159757694086, -14.14496057932236361 ) ) ;
#22972 = EDGE_LOOP ( 'NONE', ( #1861, #3814, #10320, #6150, #8722 ) ) ;
#22973 = CIRCLE ( 'NONE', #4918, 5.000000000000000888 ) ;
#22974 = EDGE_CURVE ( 'NONE', #10414, #2375, #2582, .T. ) ;
#22975 = CARTESIAN_POINT ( 'NONE',  ( -4.000000000000010658, -2.309401076758525573, -2.092734410091829034 ) ) ;
#22976 = VECTOR ( 'NONE', #1953, 1000.000000000000000 ) ;
#22977 = EDGE_CURVE ( 'NONE', #5008, #653, #29139, .T. ) ;
#22978 = CARTESIAN_POINT ( 'NONE',  ( 152.2287565553229740, -10.00000000000000178, -12.16987298107780369 ) ) ;
#22979 = CARTESIAN_POINT ( 'NONE',  ( 175.7287565553229456, -4.999999999999970690, 0.5000000000000029976 ) ) ;
#22980 = CARTESIAN_POINT ( 'NONE',  ( 2.000000000000026201, 3.464101615137736623, -2.450000000000000622 ) ) ;
#22981 = CARTESIAN_POINT ( 'NONE',  ( 158.6922820468854241, -9.999999999999998224, -35.24709285013155835 ) ) ;
#22982 = CARTESIAN_POINT ( 'NONE',  ( 9.328867290168380677, -5.000000000000015099, 28.71130127944392640 ) ) ;
#22983 = CARTESIAN_POINT ( 'NONE',  ( 23.64629180402988951, 0.1506760071912668364, -12.95843554106259710 ) ) ;
#22984 = CARTESIAN_POINT ( 'NONE',  ( 16.00562779705659011, 2.776126820729137190, -17.20623408552720690 ) ) ;
#22986 = ORIENTED_EDGE ( 'NONE', *, *, #20743, .F. ) ;
#22985 = CARTESIAN_POINT ( 'NONE',  ( 33.01522398464379648, -9.800858501837518943, -19.11635465682842394 ) ) ;
#22987 =( NAMED_UNIT ( * ) SI_UNIT ( $, .STERADIAN. ) SOLID_ANGLE_UNIT ( ) );
#22988 = CARTESIAN_POINT ( 'NONE',  ( 11.58682163191119230, 8.958038730125363003, -15.79767441425272345 ) ) ;
#22989 = CARTESIAN_POINT ( 'NONE',  ( 148.6922820468853672, -10.00000000000000355, -0.6060766987539614181 ) ) ;
#22990 = DIRECTION ( 'NONE',  ( 1.000000000000000000, 0.000000000000000000, 0.000000000000000000 ) ) ;
#22991 = CARTESIAN_POINT ( 'NONE',  ( 9.664814466656260095, 16.24138283641780944, -17.88982567228806175 ) ) ;
#22993 = EDGE_LOOP ( 'NONE', ( #16815, #3797, #21178, #27319, #19046 ) ) ;
#22992 = CARTESIAN_POINT ( 'NONE',  ( -0.6543471694412856809, -8.859816792613662173, -4.503584543331194290 ) ) ;
#22994 = ORIENTED_EDGE ( 'NONE', *, *, #8360, .F. ) ;
#22995 = CARTESIAN_POINT ( 'NONE',  ( 12.58353042223624918, -5.000000000000014211, -38.72812442006048883 ) ) ;
#22996 = CARTESIAN_POINT ( 'NONE',  ( 12.49742530276927610, 8.569573706352677789, -15.13222638044318735 ) ) ;
#22997 = ORIENTED_EDGE ( 'NONE', *, *, #23729, .T. ) ;
#22998 = CIRCLE ( 'NONE', #26855, 2.000000000000000000 ) ;
#22999 = CARTESIAN_POINT ( 'NONE',  ( 163.6922820468852819, -1.999999999999973577, -0.6060766987539614181 ) ) ;
#23000 = CARTESIAN_POINT ( 'NONE',  ( 14.49818551070089967, -5.000000000000013323, 44.62082686519693908 ) ) ;
#23001 = CARTESIAN_POINT ( 'NONE',  ( 16.01392728624657025, 9.853228751548474662, -15.03783782146776105 ) ) ;
#23002 = VERTEX_POINT ( 'NONE', #25764 ) ;
#23003 = ORIENTED_EDGE ( 'NONE', *, *, #3036, .F. ) ;
#23004 = CARTESIAN_POINT ( 'NONE',  ( 9.113844519079130180, 16.17534557870975576, -17.05418121134841414 ) ) ;
#23005 = CARTESIAN_POINT ( 'NONE',  ( 34.17142927738225922, -16.99764464586957402, -20.98398627866201238 ) ) ;
#23006 = CARTESIAN_POINT ( 'NONE',  ( 16.44673144568935541, 3.517958023484313301, -20.47440421422559353 ) ) ;
#23007 = CARTESIAN_POINT ( 'NONE',  ( 14.77364001808635585, 4.929448384924057791, -16.82930887520970131 ) ) ;
#23008 = DIRECTION ( 'NONE',  ( -0.8090169943749474513, -2.183098979609982436E-16, 0.5877852522924731371 ) ) ;
#23009 = CARTESIAN_POINT ( 'NONE',  ( 24.20684193479931068, 1.026663266619176840, -14.52337054612115708 ) ) ;
#23010 = ADVANCED_FACE ( 'NONE', ( #26378 ), #23940, .T. ) ;
#23011 = EDGE_CURVE ( 'NONE', #705, #21885, #15929, .T. ) ;
#23012 = VECTOR ( 'NONE', #187, 1000.000000000000000 ) ;
#23013 = ORIENTED_EDGE ( 'NONE', *, *, #19922, .F. ) ;
#23014 = EDGE_CURVE ( 'NONE', #26487, #15051, #12309, .T. ) ;
#23015 = CARTESIAN_POINT ( 'NONE',  ( 132.0152310637605524, -10.00000000000000711, -0.06116980274991495881 ) ) ;
#23016 = AXIS2_PLACEMENT_3D ( 'NONE', #6323, #13624, #18204 ) ;
#23017 = VERTEX_POINT ( 'NONE', #29469 ) ;
#23018 = ORIENTED_EDGE ( 'NONE', *, *, #13248, .F. ) ;
#23019 = PLANE ( 'NONE',  #3159 ) ;
#23020 = CARTESIAN_POINT ( 'NONE',  ( 174.7287565553229456, -1.999999999999968470, -33.82050807568879947 ) ) ;
#23021 = ORIENTED_EDGE ( 'NONE', *, *, #485, .T. ) ;
#23022 = CARTESIAN_POINT ( 'NONE',  ( 33.98852084862024725, -11.13792163938717472, -17.92802646347312034 ) ) ;
#23023 = CARTESIAN_POINT ( 'NONE',  ( 10.66743590522492369, 9.050377445005224786, -16.41171652237351353 ) ) ;
#23024 = PRODUCT_DEFINITION_SHAPE ( 'NONE', 'NONE',  #30268 ) ;
#23025 = VERTEX_POINT ( 'NONE', #12765 ) ;
#23026 = VECTOR ( 'NONE', #12556, 1000.000000000000000 ) ;
#23027 = CARTESIAN_POINT ( 'NONE',  ( 26.38113052396219516, -11.59678093645141672, -17.84452879788985769 ) ) ;
#23028 = CARTESIAN_POINT ( 'NONE',  ( 151.1922820468854241, -1.999999999999975797, -22.25671179336496053 ) ) ;
#23029 = CARTESIAN_POINT ( 'NONE',  ( 10.47212132250356120, 16.45172734403231729, -17.33476278219207956 ) ) ;
#23030 = LINE ( 'NONE', #24872, #26818 ) ;
#23031 = FACE_OUTER_BOUND ( 'NONE', #12530, .T. ) ;
#23032 = ORIENTED_EDGE ( 'NONE', *, *, #13945, .T. ) ;
#23033 = LINE ( 'NONE', #2135, #3227 ) ;
#23034 = CARTESIAN_POINT ( 'NONE',  ( 12.53458732174692258, 8.585986940276173485, -15.10260830673100330 ) ) ;
#23035 = ORIENTED_EDGE ( 'NONE', *, *, #23085, .F. ) ;
#23036 = DIRECTION ( 'NONE',  ( 0.3090169943749475623, 8.338696094058001131E-17, 0.9510565162951536422 ) ) ;
#23037 = VERTEX_POINT ( 'NONE', #29306 ) ;
#23038 = CARTESIAN_POINT ( 'NONE',  ( 9.667771292961528928, 16.22782245407549340, -17.88511957776909966 ) ) ;
#23039 = ADVANCED_FACE ( 'NONE', ( #21928 ), #12611, .F. ) ;
#23040 = CARTESIAN_POINT ( 'NONE',  ( 21.24065112674864864, -1.570060580458334965, -19.57950003236798864 ) ) ;
#23041 = CARTESIAN_POINT ( 'NONE',  ( 24.32739057165333207, -2.318628849198325348, -18.36682367714799824 ) ) ;
#23042 = ORIENTED_EDGE ( 'NONE', *, *, #6879, .F. ) ;
#23043 = CARTESIAN_POINT ( 'NONE',  ( 21.44014932938603835, 4.813297736510089742, -15.98289606589226075 ) ) ;
#23044 = DIRECTION ( 'NONE',  ( -0.8090169943749474513, -2.183098979609982436E-16, 0.5877852522924731371 ) ) ;
#23045 = CARTESIAN_POINT ( 'NONE',  ( 138.6922820468854525, -1.999999999999979128, -6.413161187712876909 ) ) ;
#23046 = CARTESIAN_POINT ( 'NONE',  ( 18.50902107916489570, 2.085137940960992697, -20.06823964296112450 ) ) ;
#23047 = CIRCLE ( 'NONE', #3543, 5.000000000000000888 ) ;
#23048 = ADVANCED_FACE ( 'NONE', ( #10467 ), #5609, .T. ) ;
#23049 = EDGE_CURVE ( 'NONE', #22599, #19874, #26686, .T. ) ;
#23050 = EDGE_CURVE ( 'NONE', #20351, #26883, #10628, .T. ) ;
#23051 = LINE ( 'NONE', #25783, #1801 ) ;
#23052 = EDGE_CURVE ( 'NONE', #11337, #21626, #10321, .T. ) ;
#23053 = CARTESIAN_POINT ( 'NONE',  ( 0.000000000000000000, 0.000000000000000000, 18.00000000000000000 ) ) ;
#23054 = VECTOR ( 'NONE', #3168, 1000.000000000000000 ) ;
#23055 = CARTESIAN_POINT ( 'NONE',  ( 10.35864918915110877, 16.97212501191939538, -17.98596209335946128 ) ) ;
#23056 = CARTESIAN_POINT ( 'NONE',  ( 35.54859390953724585, -22.18451583373416014, -17.99055332684694974 ) ) ;
#23057 = DIRECTION ( 'NONE',  ( 0.000000000000000000, 0.000000000000000000, 1.000000000000000000 ) ) ;
#23058 = ORIENTED_EDGE ( 'NONE', *, *, #14749, .F. ) ;
#23059 = ORIENTED_EDGE ( 'NONE', *, *, #13657, .T. ) ;
#23060 = CARTESIAN_POINT ( 'NONE',  ( 424.0000000000002274, 34.64101615137744972, 14.00000000000000178 ) ) ;
#23061 = CARTESIAN_POINT ( 'NONE',  ( 15.41431293496917121, 3.575304669039410133, -17.09800041271234150 ) ) ;
#23062 = CARTESIAN_POINT ( 'NONE',  ( 11.05541700792677062, 17.68941563399299710, -17.91138715956864047 ) ) ;
#23063 = CARTESIAN_POINT ( 'NONE',  ( 35.54859390954303677, -22.18451583373416014, -15.55638201429745848 ) ) ;
#23064 = VERTEX_POINT ( 'NONE', #29144 ) ;
#23065 = EDGE_LOOP ( 'NONE', ( #11016, #12012, #372, #30015 ) ) ;
#23066 = CARTESIAN_POINT ( 'NONE',  ( 9.642214727206800617, 17.66492910891761525, -17.80644250212319690 ) ) ;
#23067 = AXIS2_PLACEMENT_3D ( 'NONE', #12823, #22292, #17844 ) ;
#23068 = CARTESIAN_POINT ( 'NONE',  ( 12.76449053303042902, 7.629555522264023892, -14.91937138927071160 ) ) ;
#23069 = CARTESIAN_POINT ( 'NONE',  ( 180.7287565553229456, -3.999999999999994671, 0.5000000000000029976 ) ) ;
#23070 = CARTESIAN_POINT ( 'NONE',  ( 11.31764596240014598, -5.000000000000014211, 34.83213265805688508 ) ) ;
#23071 = ORIENTED_EDGE ( 'NONE', *, *, #9238, .T. ) ;
#23072 = LINE ( 'NONE', #29852, #17361 ) ;
#23073 = ORIENTED_EDGE ( 'NONE', *, *, #29578, .F. ) ;
#23074 = CARTESIAN_POINT ( 'NONE',  ( 10.46722255365007115, 16.47419372244215197, -17.33720764016775462 ) ) ;
#23075 = CARTESIAN_POINT ( 'NONE',  ( 33.78657425947636739, -10.78854458652579495, -19.16640759269550287 ) ) ;
#23076 = CARTESIAN_POINT ( 'NONE',  ( 25.73595588610537277, -4.826321120321507507, -18.84379041344559269 ) ) ;
#23077 = VERTEX_POINT ( 'NONE', #24232 ) ;
#23078 = FACE_OUTER_BOUND ( 'NONE', #667, .T. ) ;
#23079 = VECTOR ( 'NONE', #3317, 999.9999999999998863 ) ;
#23080 = CARTESIAN_POINT ( 'NONE',  ( 148.6922820468854241, -10.00000000000000178, -17.92658477444275889 ) ) ;
#23081 = CARTESIAN_POINT ( 'NONE',  ( 0.000000000000000000, 0.000000000000000000, 15.00000000000000000 ) ) ;
#23082 = CARTESIAN_POINT ( 'NONE',  ( 18.30550780621970475, 8.505200139115956404, -19.80988581799093140 ) ) ;
#23083 = CARTESIAN_POINT ( 'NONE',  ( 24.94059380785660451, 0.5691772567322460619, -14.01379559947946518 ) ) ;
#23084 = EDGE_CURVE ( 'NONE', #27188, #29946, #1495, .T. ) ;
#23086 = VERTEX_POINT ( 'NONE', #17494 ) ;
#23085 = EDGE_CURVE ( 'NONE', #26148, #20749, #3471, .T. ) ;
#23087 = CARTESIAN_POINT ( 'NONE',  ( 6.938893903907228378E-15, 55.00000000000000711, -1.040834085586084257E-14 ) ) ;
#23088 = CARTESIAN_POINT ( 'NONE',  ( 99.29987472633386858, -4.999999999999990230, -72.14558201428623363 ) ) ;
#23089 = CARTESIAN_POINT ( 'NONE',  ( 172.7287565553229456, -4.999999999999970690, 3.500000000000003109 ) ) ;
#23090 = CARTESIAN_POINT ( 'NONE',  ( 129.5152310637605808, -10.00000000000000888, -2.627941064794695691 ) ) ;
#23091 = VECTOR ( 'NONE', #6156, 1000.000000000000000 ) ;
#23092 = CARTESIAN_POINT ( 'NONE',  ( 10.72208662246453770, 16.62525560183325624, -15.95366392025685620 ) ) ;
#23093 = LINE ( 'NONE', #27102, #22411 ) ;
#23094 = ORIENTED_EDGE ( 'NONE', *, *, #29210, .F. ) ;
#23095 = DIRECTION ( 'NONE',  ( 0.9773680663943724589, 2.003532158470062816E-17, 0.2115458881484709175 ) ) ;
#23096 = ORIENTED_EDGE ( 'NONE', *, *, #9926, .F. ) ;
#23097 = CARTESIAN_POINT ( 'NONE',  ( 9.916118674515717046, 16.40877069192658055, -16.50468880802031890 ) ) ;
#23098 = CARTESIAN_POINT ( 'NONE',  ( 16.64656040655037827, 6.484405094197702724, -15.29036880746224014 ) ) ;
#23099 = DIRECTION ( 'NONE',  ( 0.000000000000000000, 1.000000000000000000, -1.224646799147353207E-16 ) ) ;
#23100 = LINE ( 'NONE', #22802, #10803 ) ;
#23102 = ORIENTED_EDGE ( 'NONE', *, *, #10410, .T. ) ;
#23101 = CARTESIAN_POINT ( 'NONE',  ( 29.66490191837812773, -8.365349891895018430, -17.62461620872172574 ) ) ;
#23103 = VERTEX_POINT ( 'NONE', #22547 ) ;
#23104 = LINE ( 'NONE', #20500, #11519 ) ;
#23105 = CARTESIAN_POINT ( 'NONE',  ( 12.27235684156208961, 9.528132359803098694, -15.31161062812042317 ) ) ;
#23106 = EDGE_CURVE ( 'NONE', #22675, #24876, #12913, .T. ) ;
#23107 = CARTESIAN_POINT ( 'NONE',  ( 35.54859390954303677, -22.18451583373416014, -15.55638201429745848 ) ) ;
#23108 = CARTESIAN_POINT ( 'NONE',  ( 148.6922820468853956, -1.999999999999977129, -9.266330736598359152 ) ) ;
#23109 = DIRECTION ( 'NONE',  ( 0.5877852522924731371, 0.000000000000000000, 0.8090169943749474513 ) ) ;
#23110 = CARTESIAN_POINT ( 'NONE',  ( 23.28032035799162358, -0.8411909528121862545, -14.99295998388115869 ) ) ;
#23111 = ORIENTED_EDGE ( 'NONE', *, *, #7198, .T. ) ;
#23112 = CARTESIAN_POINT ( 'NONE',  ( 158.6922820468853104, -4.999999999999974243, 2.247092850131519715 ) ) ;
#23113 = CARTESIAN_POINT ( 'NONE',  ( 19.75232399841803854, 1.290101960903724754, -14.36573431580270999 ) ) ;
#23114 = CARTESIAN_POINT ( 'NONE',  ( 28.07139740185986199, -11.61962552671339388, -17.78409693965565452 ) ) ;
#23115 = CIRCLE ( 'NONE', #17733, 2.928571428571432378 ) ;
#23116 = VERTEX_POINT ( 'NONE', #26846 ) ;
#23117 = CARTESIAN_POINT ( 'NONE',  ( 162.0152310637604671, -9.999999999999998224, -6.958068083716895558 ) ) ;
#23118 = CARTESIAN_POINT ( 'NONE',  ( 132.0152310637605524, -4.999999999999982236, -26.04193191628310800 ) ) ;
#23119 = DIRECTION ( 'NONE',  ( 0.5877852522924731371, 1.586114251531760728E-16, -0.8090169943749474513 ) ) ;
#23120 = LINE ( 'NONE', #22531, #8666 ) ;
#23121 = FACE_OUTER_BOUND ( 'NONE', #16203, .T. ) ;
#23122 = CARTESIAN_POINT ( 'NONE',  ( 9.870716668364401869, 16.61699007954640805, -16.53972800451630931 ) ) ;
#23123 = CARTESIAN_POINT ( 'NONE',  ( 18.38621934312857320, -2.136830130942094730, -15.12482301043797683 ) ) ;
#23124 = CARTESIAN_POINT ( 'NONE',  ( 16.12927480167980576, 2.990883400875756326, -18.25071113400840517 ) ) ;
#23126 = ORIENTED_EDGE ( 'NONE', *, *, #7945, .T. ) ;
#23125 = CARTESIAN_POINT ( 'NONE',  ( 33.20847722810714231, -12.67161117835268058, -20.69290897523819694 ) ) ;
#23127 = PRESENTATION_STYLE_ASSIGNMENT (( #27746 ) ) ;
#23128 = CARTESIAN_POINT ( 'NONE',  ( 12.37169234869624646, 8.529253869913038244, -15.23127513898213081 ) ) ;
#23129 = VECTOR ( 'NONE', #29607, 1000.000000000000000 ) ;
#23130 = DIRECTION ( 'NONE',  ( 0.000000000000000000, 0.4999999999999993339, -0.8660254037844390407 ) ) ;
#23131 = DIRECTION ( 'NONE',  ( 0.9510565162951536422, 2.566386769018988816E-16, 0.3090169943749472292 ) ) ;
#23132 = CARTESIAN_POINT ( 'NONE',  ( 17.29421355564066332, 9.360779442694735053, -19.18964209290773937 ) ) ;
#23133 = ORIENTED_EDGE ( 'NONE', *, *, #10559, .T. ) ;
#23134 = CARTESIAN_POINT ( 'NONE',  ( 149.7287565553230309, -4.999999999999976907, -25.16025403784439973 ) ) ;
#23135 = CARTESIAN_POINT ( 'NONE',  ( 12.52778158092594474, 8.582979361647906202, -15.10803260229456946 ) ) ;
#23136 = EDGE_CURVE ( 'NONE', #1908, #4171, #22228, .T. ) ;
#23137 = ORIENTED_EDGE ( 'NONE', *, *, #7058, .F. ) ;
#23138 = DIRECTION ( 'NONE',  ( -1.000000000000000000, 0.000000000000000000, 0.000000000000000000 ) ) ;
#23139 = CARTESIAN_POINT ( 'NONE',  ( 4.000000000000008882, -6.928203230275510549, -5.000000000000000888 ) ) ;
#23140 = ADVANCED_FACE ( 'NONE', ( #1645, #17642 ), #3622, .T. ) ;
#23141 = CARTESIAN_POINT ( 'NONE',  ( 17.88091890332929523, 4.544920326333207861, -13.91018511019278669 ) ) ;
#23142 = VERTEX_POINT ( 'NONE', #6060 ) ;
#23143 = CARTESIAN_POINT ( 'NONE',  ( 9.193626274318058123, 15.80945627937554576, -17.02118864906812234 ) ) ;
#23144 = CARTESIAN_POINT ( 'NONE',  ( 31.63980255171021483, -10.89810845426378982, -15.52824638758754183 ) ) ;
#23145 = CARTESIAN_POINT ( 'NONE',  ( 15.23446545079332815, 2.143032791470029341, -16.75203451335420368 ) ) ;
#23146 = CARTESIAN_POINT ( 'NONE',  ( 15.30293317557315902, 5.113330479851449617, -15.60941525921096051 ) ) ;
#23147 = CARTESIAN_POINT ( 'NONE',  ( 157.2287565553230024, -4.999999999999975131, -29.49038105676660138 ) ) ;
#23148 = CARTESIAN_POINT ( 'NONE',  ( 22.59259966355045890, -3.831908474886262184, -12.47183693924707804 ) ) ;
#23149 = VECTOR ( 'NONE', #19583, 1000.000000000000000 ) ;
#23150 = VERTEX_POINT ( 'NONE', #15346 ) ;
#23151 = CARTESIAN_POINT ( 'NONE',  ( -7.999999999999998224, 3.871967595402137974, -4.501061386767540640 ) ) ;
#23153 = VERTEX_POINT ( 'NONE', #20092 ) ;
#23152 = LINE ( 'NONE', #25446, #15067 ) ;
#23154 = ORIENTED_EDGE ( 'NONE', *, *, #29248, .F. ) ;
#23155 = DIRECTION ( 'NONE',  ( -2.698458740408365879E-16, 1.000000000000000000, 0.000000000000000000 ) ) ;
#23156 = DIRECTION ( 'NONE',  ( -2.698458740408365879E-16, 1.000000000000000000, 0.000000000000000000 ) ) ;
#23157 = CARTESIAN_POINT ( 'NONE',  ( 34.61014508914255572, -12.47609210860084161, -18.96169567217477692 ) ) ;
#23158 = CARTESIAN_POINT ( 'NONE',  ( 12.70479305047265761, 7.604386330824797646, -14.96685888413283294 ) ) ;
#23159 = VERTEX_POINT ( 'NONE', #24683 ) ;
#23160 = PLANE ( 'NONE',  #18563 ) ;
#23161 = LINE ( 'NONE', #25458, #5033 ) ;
#23162 = CARTESIAN_POINT ( 'NONE',  ( 10.47187086816178159, 16.45287595956923354, -17.33486661187913214 ) ) ;
#23163 = DIRECTION ( 'NONE',  ( -1.000000000000000000, -2.698458740408365879E-16, 0.000000000000000000 ) ) ;
#23164 = CARTESIAN_POINT ( 'NONE',  ( 152.0152310637605808, -1.999999999999974465, -34.70218595412750773 ) ) ;
#23165 = EDGE_CURVE ( 'NONE', #12496, #17958, #3773, .T. ) ;
#23166 = EDGE_CURVE ( 'NONE', #29853, #6425, #3234, .T. ) ;
#23167 = VERTEX_POINT ( 'NONE', #15503 ) ;
#23168 = DIRECTION ( 'NONE',  ( 0.9510565162951536422, 2.566386769018988816E-16, 0.3090169943749472292 ) ) ;
#23169 = EDGE_CURVE ( 'NONE', #1890, #29392, #24834, .T. ) ;
#23170 = VECTOR ( 'NONE', #25050, 1000.000000000000000 ) ;
#23171 = CARTESIAN_POINT ( 'NONE',  ( 12.56861602585598980, 8.601024833420110483, -15.07548682890769243 ) ) ;
#23172 = EDGE_CURVE ( 'NONE', #25866, #12094, #28852, .T. ) ;
#23173 = LINE ( 'NONE', #7300, #14956 ) ;
#23174 = ORIENTED_EDGE ( 'NONE', *, *, #22881, .F. ) ;
#23175 = CARTESIAN_POINT ( 'NONE',  ( 9.688134281814004822, 16.13443519152062677, -17.87669530545171881 ) ) ;
#23176 = CARTESIAN_POINT ( 'NONE',  ( 24.39898194048076974, -1.181968365584514791, -14.84216225329429051 ) ) ;
#23177 = CARTESIAN_POINT ( 'NONE',  ( 22.74932893098897324, -1.793276863599028381, -13.92998459126509836 ) ) ;
#23178 = CARTESIAN_POINT ( 'NONE',  ( 18.25949499138229726, 0.6315596619015936275, -15.69045325149238934 ) ) ;
#23179 = DIRECTION ( 'NONE',  ( -2.698458740408365879E-16, 1.000000000000000000, 0.000000000000000000 ) ) ;
#23180 = DIRECTION ( 'NONE',  ( -0.8090169943749474513, -2.183098979609982436E-16, -0.5877852522924731371 ) ) ;
#23181 = CARTESIAN_POINT ( 'NONE',  ( -5.690023276062409430, -5.952467836904174803, -0.1306530452038248968 ) ) ;
#23182 = CARTESIAN_POINT ( 'NONE',  ( 28.15048769591263067, -5.842385520647848551, -16.89978903947823241 ) ) ;
#23183 = VECTOR ( 'NONE', #16288, 1000.000000000000000 ) ;
#23184 = CARTESIAN_POINT ( 'NONE',  ( 132.0152310637605808, -1.999999999999981348, 1.702185954127501066 ) ) ;
#23185 = CARTESIAN_POINT ( 'NONE',  ( 13.94177938065702804, -5.000000000000014211, 42.90838487877751817 ) ) ;
#23186 = PLANE ( 'NONE',  #16039 ) ;
#23187 = VECTOR ( 'NONE', #28966, 1000.000000000000000 ) ;
#23188 = DIRECTION ( 'NONE',  ( -2.698458740408365879E-16, 1.000000000000000000, 0.000000000000000000 ) ) ;
#23189 = CARTESIAN_POINT ( 'NONE',  ( 3.345653888883659555, -2.687187980154746025, -2.310849780464848013 ) ) ;
#23190 = ADVANCED_FACE ( 'NONE', ( #3331 ), #15953, .T. ) ;
#23191 = CARTESIAN_POINT ( 'NONE',  ( 10.35870477237433818, 16.97187010017241349, -17.89775757279876700 ) ) ;
#23192 = DIRECTION ( 'NONE',  ( 1.000000000000000000, 0.000000000000000000, 0.000000000000000000 ) ) ;
#23193 = LINE ( 'NONE', #29526, #19959 ) ;
#23194 = ORIENTED_EDGE ( 'NONE', *, *, #10098, .F. ) ;
#23195 = CARTESIAN_POINT ( 'NONE',  ( 11.22298328736398965, 9.095422004326360721, -17.24198125015536576 ) ) ;
#23196 = ORIENTED_EDGE ( 'NONE', *, *, #21900, .T. ) ;
#23197 = DIRECTION ( 'NONE',  ( -0.9510565162951536422, -2.566386769018988323E-16, 0.3090169943749475623 ) ) ;
#23198 = CARTESIAN_POINT ( 'NONE',  ( 19.83745040964868522, -2.306422872736943575, -14.39351019504378293 ) ) ;
#23199 = CARTESIAN_POINT ( 'NONE',  ( 11.27618196228310232, 16.67695941232857137, -16.78452903358395076 ) ) ;
#23200 = CARTESIAN_POINT ( 'NONE',  ( 35.54859569580823830, -22.18452385850428499, -18.27063337037174762 ) ) ;
#23201 = ORIENTED_EDGE ( 'NONE', *, *, #23481, .F. ) ;
#23202 = ORIENTED_EDGE ( 'NONE', *, *, #13526, .F. ) ;
#23203 = CARTESIAN_POINT ( 'NONE',  ( 9.916824447075894611, 16.40553392900050156, -16.50439446175997205 ) ) ;
#23204 = ADVANCED_FACE ( 'NONE', ( #20830 ), #22692, .F. ) ;
#23205 = AXIS2_PLACEMENT_3D ( 'NONE', #400, #16722, #7562 ) ;
#23206 = CARTESIAN_POINT ( 'NONE',  ( 9.641350810849047548, 17.66889113945805789, -17.93331994345748370 ) ) ;
#23207 = DIRECTION ( 'NONE',  ( -0.9510565162951536422, -2.566386769018988323E-16, 0.3090169943749475623 ) ) ;
#23208 = DIRECTION ( 'NONE',  ( 0.5877852522924731371, 1.586114251531760728E-16, -0.8090169943749474513 ) ) ;
#23209 = EDGE_CURVE ( 'NONE', #10712, #12856, #4220, .T. ) ;
#23210 = EDGE_CURVE ( 'NONE', #15878, #4416, #13517, .T. ) ;
#23211 = ORIENTED_EDGE ( 'NONE', *, *, #7736, .T. ) ;
#23212 = FACE_OUTER_BOUND ( 'NONE', #5337, .T. ) ;
#23213 = EDGE_LOOP ( 'NONE', ( #28578, #27499, #17825, #27689 ) ) ;
#23214 = CARTESIAN_POINT ( 'NONE',  ( 10.47175433613752027, 16.45341039028688002, -17.33491556667247835 ) ) ;
#23216 = CARTESIAN_POINT ( 'NONE',  ( 34.14034160798153295, -12.36551392957089135, -20.90432844665832590 ) ) ;
#23215 = CIRCLE ( 'NONE', #10037, 5.000000000000000888 ) ;
#23217 = CARTESIAN_POINT ( 'NONE',  ( 26.61709978538234012, -3.831456866606135492, -17.85214630790261836 ) ) ;
#23218 = EDGE_LOOP ( 'NONE', ( #25101, #21007, #586, #20190 ) ) ;
#23219 = CIRCLE ( 'NONE', #4203, 5.000000000000000000 ) ;
#23220 = FACE_OUTER_BOUND ( 'NONE', #12706, .T. ) ;
#23221 = LINE ( 'NONE', #27688, #4981 ) ;
#23222 =( LENGTH_UNIT ( ) NAMED_UNIT ( * ) SI_UNIT ( .MILLI., .METRE. ) );
#23223 = CARTESIAN_POINT ( 'NONE',  ( 18.83884422780463552, 9.149888288241003309, -18.99120665306858768 ) ) ;
#23224 = CARTESIAN_POINT ( 'NONE',  ( 30.43753979984721525, -10.17066761781405937, -14.50402091508011537 ) ) ;
#23225 = ORIENTED_EDGE ( 'NONE', *, *, #28249, .T. ) ;
#23226 = CARTESIAN_POINT ( 'NONE',  ( 159.5152310637604671, -4.999999999999974243, -1.770974823053888726E-14 ) ) ;
#23227 = AXIS2_PLACEMENT_3D ( 'NONE', #7241, #26313, #28626 ) ;
#23228 = ORIENTED_EDGE ( 'NONE', *, *, #2596, .F. ) ;
#23229 = CYLINDRICAL_SURFACE ( 'NONE', #28213, 13.00000000000000178 ) ;
#23230 = DIRECTION ( 'NONE',  ( 0.5877852522924731371, 1.586114251531760728E-16, 0.8090169943749474513 ) ) ;
#23231 = VECTOR ( 'NONE', #9190, 1000.000000000000000 ) ;
#23232 = PLANE ( 'NONE',  #9474 ) ;
#23233 = AXIS2_PLACEMENT_3D ( 'NONE', #11922, #18804, #6920 ) ;
#23234 = UNCERTAINTY_MEASURE_WITH_UNIT (LENGTH_MEASURE( 1.000000000000000082E-05 ), #2237, 'distance_accuracy_value', 'NONE');
#23235 = CARTESIAN_POINT ( 'NONE',  ( 10.68867725192709273, 16.77847523382220984, -15.97313786900300059 ) ) ;
#23236 = PLANE ( 'NONE',  #18735 ) ;
#23237 = ORIENTED_EDGE ( 'NONE', *, *, #25287, .F. ) ;
#23238 = CARTESIAN_POINT ( 'NONE',  ( 2.645508037661891354, 7.710219529346620249, -0.06809871960543666114 ) ) ;
#23239 = VERTEX_POINT ( 'NONE', #27461 ) ;
#23240 = CARTESIAN_POINT ( 'NONE',  ( 9.916775705961365261, 16.40575746196480011, -16.50441451066904364 ) ) ;
#23241 = ORIENTED_EDGE ( 'NONE', *, *, #16099, .T. ) ;
#23242 = EDGE_CURVE ( 'NONE', #14016, #12198, #4518, .T. ) ;
#23243 = EDGE_CURVE ( 'NONE', #10342, #16735, #13806, .T. ) ;
#23244 = CARTESIAN_POINT ( 'NONE',  ( 17.80416238081608071, 8.561068417093343541, -18.87148919878627140 ) ) ;
#23245 = CARTESIAN_POINT ( 'NONE',  ( 152.0152310637604955, -4.999999999999976907, -1.687708096207002301E-14 ) ) ;
#23246 = DIRECTION ( 'NONE',  ( 0.9510565162951536422, 2.566386769018988816E-16, 0.3090169943749472292 ) ) ;
#23247 = EDGE_CURVE ( 'NONE', #21669, #19668, #1948, .T. ) ;
#23249 = VERTEX_POINT ( 'NONE', #15803 ) ;
#23248 = CARTESIAN_POINT ( 'NONE',  ( 28.09718568327657806, -5.958257988085632562, -17.17874431236187149 ) ) ;
#23250 = ORIENTED_EDGE ( 'NONE', *, *, #27617, .F. ) ;
#23251 = DIRECTION ( 'NONE',  ( 0.5877852522924731371, 1.586114251531760728E-16, 0.8090169943749474513 ) ) ;
#23252 = EDGE_CURVE ( 'NONE', #4418, #10720, #23285, .T. ) ;
#23253 = CARTESIAN_POINT ( 'NONE',  ( 11.35716248442908061, 16.30557241515140277, -16.75104082405111683 ) ) ;
#23254 = EDGE_CURVE ( 'NONE', #314, #11816, #16875, .T. ) ;
#23255 = CARTESIAN_POINT ( 'NONE',  ( 35.54859390953723874, -22.18451583373416014, -15.00000000000000000 ) ) ;
#23256 = LINE ( 'NONE', #13780, #5437 ) ;
#23257 = AXIS2_PLACEMENT_3D ( 'NONE', #1260, #3112, #21851 ) ;
#23258 = CARTESIAN_POINT ( 'NONE',  ( 164.5152310637604387, -9.999999999999998224, -4.391296821672111328 ) ) ;
#23259 = CARTESIAN_POINT ( 'NONE',  ( 27.22116495027615812, -8.412805768781604243, -11.93592671293571605 ) ) ;
#23260 = ORIENTED_EDGE ( 'NONE', *, *, #1207, .T. ) ;
#23261 = CARTESIAN_POINT ( 'NONE',  ( 5.000000000000002665, 3.306546357697854226E-16, 2.700000000000001066 ) ) ;
#23262 = ORIENTED_EDGE ( 'NONE', *, *, #6151, .T. ) ;
#23263 = CARTESIAN_POINT ( 'NONE',  ( 16.37314578033188894, 3.237113944496374351, -18.86778596048347723 ) ) ;
#23264 = VECTOR ( 'NONE', #12204, 1000.000000000000000 ) ;
#23265 = CARTESIAN_POINT ( 'NONE',  ( 30.29779709953443501, -9.168887887504279632, -16.05354238668875055 ) ) ;
#23266 = ORIENTED_EDGE ( 'NONE', *, *, #15965, .F. ) ;
#23267 = DIRECTION ( 'NONE',  ( -1.000000000000000000, 0.000000000000000000, 0.000000000000000000 ) ) ;
#23268 = DIRECTION ( 'NONE',  ( 0.000000000000000000, -1.000000000000000000, 0.000000000000000000 ) ) ;
#23269 = CARTESIAN_POINT ( 'NONE',  ( 173.6922820468853388, -9.999999999999994671, -26.58683881228715862 ) ) ;
#23270 = CARTESIAN_POINT ( 'NONE',  ( 169.7287565553229172, -4.999999999999972466, -7.839745962155600267 ) ) ;
#23271 = AXIS2_PLACEMENT_3D ( 'NONE', #5798, #28575, #26415 ) ;
#23272 = CARTESIAN_POINT ( 'NONE',  ( 9.643509238790151983, 17.65899231378470446, -17.74106871770035099 ) ) ;
#23273 = CARTESIAN_POINT ( 'NONE',  ( 22.70908579165946506, -0.2254420654732764706, -12.61778515557981528 ) ) ;
#23274 = CARTESIAN_POINT ( 'NONE',  ( 23.41849298471255381, -3.203224238779429633, -13.27670244232306018 ) ) ;
#23276 = ORIENTED_EDGE ( 'NONE', *, *, #14091, .F. ) ;
#23275 = CARTESIAN_POINT ( 'NONE',  ( 32.00851579392290347, -10.30430276118739918, -18.57203464379605151 ) ) ;
#23277 =( NAMED_UNIT ( * ) SI_UNIT ( $, .STERADIAN. ) SOLID_ANGLE_UNIT ( ) );
#23278 = VECTOR ( 'NONE', #13636, 1000.000000000000000 ) ;
#23279 = CARTESIAN_POINT ( 'NONE',  ( 12.77278825050581013, 8.691252192278360766, -14.91275796197543890 ) ) ;
#23280 = DIRECTION ( 'NONE',  ( -0.5877852522924731371, 0.000000000000000000, 0.8090169943749474513 ) ) ;
#23281 = CARTESIAN_POINT ( 'NONE',  ( 134.5152310637605524, -1.999999999999980460, -30.37205893520530964 ) ) ;
#23282 = ADVANCED_FACE ( 'NONE', ( #29921 ), #18550, .T. ) ;
#23283 = CARTESIAN_POINT ( 'NONE',  ( 17.17204249742301059, 10.23148044644768362, -15.96021614775051667 ) ) ;
#23284 = ORIENTED_EDGE ( 'NONE', *, *, #26974, .F. ) ;
#23285 = LINE ( 'NONE', #8635, #20261 ) ;
#23286 = ADVANCED_FACE ( 'NONE', ( #20382 ), #30213, .T. ) ;
#23287 = CARTESIAN_POINT ( 'NONE',  ( 10.72892505862787971, 16.59389366189031634, -15.95083598634710320 ) ) ;
#23288 = VERTEX_POINT ( 'NONE', #23134 ) ;
#23289 = PLANE ( 'NONE',  #22248 ) ;
#23290 = PLANE ( 'NONE',  #22491 ) ;
#23291 = CARTESIAN_POINT ( 'NONE',  ( 20.23291344124205793, 5.521974472852556381, -14.51730806008046137 ) ) ;
#23292 = VERTEX_POINT ( 'NONE', #27601 ) ;
#23293 = ORIENTED_EDGE ( 'NONE', *, *, #29993, .F. ) ;
#23294 = CARTESIAN_POINT ( 'NONE',  ( 33.10306327339915811, -12.22190834454405106, -20.64716665866461298 ) ) ;
#23295 = CARTESIAN_POINT ( 'NONE',  ( 21.76348650023563636, -1.483442554740824537, -14.70963264896640155 ) ) ;
#23296 = CARTESIAN_POINT ( 'NONE',  ( 31.88113401528661939, -11.03952345999570639, -14.96145667752709585 ) ) ;
#23297 = VECTOR ( 'NONE', #8737, 1000.000000000000000 ) ;
#23298 = CARTESIAN_POINT ( 'NONE',  ( 23.10480167063333212, 0.6704577443818302562, -13.62402792225823944 ) ) ;
#23299 = VECTOR ( 'NONE', #20024, 1000.000000000000000 ) ;
#23300 = ORIENTED_EDGE ( 'NONE', *, *, #14691, .T. ) ;
#23301 = FACE_OUTER_BOUND ( 'NONE', #4930, .T. ) ;
#23302 = ORIENTED_EDGE ( 'NONE', *, *, #5600, .T. ) ;
#23303 = EDGE_CURVE ( 'NONE', #15830, #27224, #9222, .T. ) ;
#23305 = VERTEX_POINT ( 'NONE', #8782 ) ;
#23304 = DIRECTION ( 'NONE',  ( 0.000000000000000000, 0.000000000000000000, 1.000000000000000000 ) ) ;
#23306 = DIRECTION ( 'NONE',  ( -0.5877852522924731371, 0.000000000000000000, 0.8090169943749474513 ) ) ;
#23307 = DIRECTION ( 'NONE',  ( -0.9510565162951536422, -2.566386769018988816E-16, -0.3090169943749472292 ) ) ;
#23308 = CARTESIAN_POINT ( 'NONE',  ( 36.54859390953724585, -21.18451583373416014, -17.64281456791166391 ) ) ;
#23309 = CARTESIAN_POINT ( 'NONE',  ( 9.641350777746193756, 17.66889129127197577, -17.91630266473768884 ) ) ;
#23310 = ORIENTED_EDGE ( 'NONE', *, *, #6057, .F. ) ;
#23311 = AXIS2_PLACEMENT_3D ( 'NONE', #14327, #21969, #28731 ) ;
#23312 = FACE_BOUND ( 'NONE', #20097, .T. ) ;
#23313 = PLANE ( 'NONE',  #8451 ) ;
#23314 = CARTESIAN_POINT ( 'NONE',  ( 10.47008273352651564, 16.46107657294071203, -17.33567129194344858 ) ) ;
#23315 = DIRECTION ( 'NONE',  ( -1.000000000000000000, 0.000000000000000000, 0.000000000000000000 ) ) ;
#23316 = CARTESIAN_POINT ( 'NONE',  ( 137.0152310637605524, -1.999999999999980016, -0.06116980274991495881 ) ) ;
#23317 = ORIENTED_EDGE ( 'NONE', *, *, #25324, .T. ) ;
#23318 = VECTOR ( 'NONE', #1093, 1000.000000000000000 ) ;
#23319 = DIRECTION ( 'NONE',  ( 0.000000000000000000, 0.000000000000000000, 1.000000000000000000 ) ) ;
#23320 = DIRECTION ( 'NONE',  ( 1.000000000000000000, 4.440892098500622217E-16, 0.000000000000000000 ) ) ;
#23321 = EDGE_LOOP ( 'NONE', ( #22484, #320, #19398, #26906 ) ) ;
#23322 = CARTESIAN_POINT ( 'NONE',  ( 147.0152310637605808, -10.00000000000000178, -15.61832212156129707 ) ) ;
#23323 = VERTEX_POINT ( 'NONE', #27311 ) ;
#23324 = CARTESIAN_POINT ( 'NONE',  ( 9.672937757006597081, 16.20412839139380168, -17.88297960302892520 ) ) ;
#23325 = CIRCLE ( 'NONE', #2888, 2.100000000000000977 ) ;
#23326 = CARTESIAN_POINT ( 'NONE',  ( 25.61676826379006400, -5.274948970184475172, -14.00514367894158418 ) ) ;
#23327 = CARTESIAN_POINT ( 'NONE',  ( 21.31799488982693802, -2.441251725956471219, -14.24326171688714204 ) ) ;
#23328 = CARTESIAN_POINT ( 'NONE',  ( 18.32179412900206827, 3.681508181950223335, -14.15692665485406643 ) ) ;
#23329 = DIRECTION ( 'NONE',  ( -2.698458740408365879E-16, 1.000000000000000000, 0.000000000000000000 ) ) ;
#23330 = DIRECTION ( 'NONE',  ( -0.8660254037844377084, -0.5000000000000014433, 0.000000000000000000 ) ) ;
#23331 = CARTESIAN_POINT ( 'NONE',  ( 6.227276357848867683, -5.000000000000015987, 19.16558592799212235 ) ) ;
#23332 = CARTESIAN_POINT ( 'NONE',  ( 24.43075134246613800, -6.859861339260811874, -14.00379227226492951 ) ) ;
#23333 = CARTESIAN_POINT ( 'NONE',  ( 148.6922820468853956, -10.00000000000000178, -6.413161187712876909 ) ) ;
#23334 = EDGE_CURVE ( 'NONE', #14318, #19672, #6638, .T. ) ;
#23335 = DIRECTION ( 'NONE',  ( -1.000000000000000000, 0.000000000000000000, -0.000000000000000000 ) ) ;
#23336 = EDGE_CURVE ( 'NONE', #29174, #16977, #27907, .T. ) ;
#23337 = AXIS2_PLACEMENT_3D ( 'NONE', #22184, #17452, #3293 ) ;
#23338 = FACE_OUTER_BOUND ( 'NONE', #9180, .T. ) ;
#23339 = EDGE_CURVE ( 'NONE', #24460, #21674, #4369, .T. ) ;
#23340 = FACE_OUTER_BOUND ( 'NONE', #14461, .T. ) ;
#23341 = DIRECTION ( 'NONE',  ( -2.698458740408365879E-16, 1.000000000000000000, 0.000000000000000000 ) ) ;
#23342 = VECTOR ( 'NONE', #2903, 999.9999999999998863 ) ;
#23343 = CARTESIAN_POINT ( 'NONE',  ( 10.35867142355733783, 16.97202304209818990, -17.90451223021000260 ) ) ;
#23344 = LINE ( 'NONE', #27517, #14050 ) ;
#23345 = TOROIDAL_SURFACE ( 'NONE', #7278, 3.149999999999996358, 0.8500000000000000888 ) ;
#23346 = CARTESIAN_POINT ( 'NONE',  ( 32.52799721746220740, -11.03300674309804386, -18.03857687357939099 ) ) ;
#23347 = VERTEX_POINT ( 'NONE', #4659 ) ;
#23348 = CARTESIAN_POINT ( 'NONE',  ( 11.25771276049011327, 8.953580691464267716, -17.22628983894280807 ) ) ;
#23349 = ORIENTED_EDGE ( 'NONE', *, *, #18823, .F. ) ;
#23350 = DIRECTION ( 'NONE',  ( -1.000000000000000000, 0.000000000000000000, 0.000000000000000000 ) ) ;
#23351 = CARTESIAN_POINT ( 'NONE',  ( 19.68115760211910725, 3.144890361740488860, -20.29587546762095940 ) ) ;
#23352 = CARTESIAN_POINT ( 'NONE',  ( 11.05818223728759264, 17.67673393965927175, -17.74095938596937572 ) ) ;
#23353 = DIRECTION ( 'NONE',  ( 0.000000000000000000, -0.7071067811865456854, -0.7071067811865493491 ) ) ;
#23354 = EDGE_LOOP ( 'NONE', ( #1653, #214, #10838, #29163 ) ) ;
#23355 = VERTEX_POINT ( 'NONE', #11374 ) ;
#23356 = CARTESIAN_POINT ( 'NONE',  ( 9.641351338355821810, 17.66888872024471624, -17.91303689663363130 ) ) ;
#23357 = CARTESIAN_POINT ( 'NONE',  ( -12.69484042717385464, 39.89788248176327556, 9.999999999999998224 ) ) ;
#23358 = CARTESIAN_POINT ( 'NONE',  ( 10.04637620539468124, 15.81139305134258599, -16.45082025127570091 ) ) ;
#23359 = DIRECTION ( 'NONE',  ( -0.9510565162951536422, -2.566386769018988816E-16, -0.3090169943749472292 ) ) ;
#23360 = DIRECTION ( 'NONE',  ( -2.698458740408365879E-16, 1.000000000000000000, 0.000000000000000000 ) ) ;
#23361 = ORIENTED_EDGE ( 'NONE', *, *, #29248, .T. ) ;
#23362 = LINE ( 'NONE', #4892, #21774 ) ;
#23363 = EDGE_LOOP ( 'NONE', ( #26939, #7800, #25508, #3656, #22407 ) ) ;
#23364 = CARTESIAN_POINT ( 'NONE',  ( 10.47187086816178159, 16.45287595956923354, -17.33486661187913214 ) ) ;
#23365 = ORIENTED_EDGE ( 'NONE', *, *, #3600, .F. ) ;
#23366 = AXIS2_PLACEMENT_3D ( 'NONE', #19546, #15566, #18159 ) ;
#23367 = CARTESIAN_POINT ( 'NONE',  ( 35.97124720801268438, -19.59080293283771823, -20.41544573823858144 ) ) ;
#23368 = CARTESIAN_POINT ( 'NONE',  ( 26.07968421886551980, -9.001936657367064498, -13.61655714643126913 ) ) ;
#23369 = DIRECTION ( 'NONE',  ( 2.207829878515935943E-16, -1.000000000000000000, 0.000000000000000000 ) ) ;
#23370 = VECTOR ( 'NONE', #8653, 1000.000000000000000 ) ;
#23371 = CARTESIAN_POINT ( 'NONE',  ( 33.33685173283005554, -10.38074443705513161, -18.09276096107157628 ) ) ;
#23372 = CARTESIAN_POINT ( 'NONE',  ( 0.000000000000000000, 1.734723475976807094E-15, 28.00000000000000355 ) ) ;
#23373 = CARTESIAN_POINT ( 'NONE',  ( 27.39958189869922123, -12.72506959635235368, -13.65552181841346524 ) ) ;
#23374 = CARTESIAN_POINT ( 'NONE',  ( 25.72483820513325270, -9.972596264566449875, -15.12420980763781664 ) ) ;
#23375 = ORIENTED_EDGE ( 'NONE', *, *, #5295, .T. ) ;
#23376 = FACE_BOUND ( 'NONE', #10504, .T. ) ;
#23377 = EDGE_CURVE ( 'NONE', #23552, #19492, #18401, .T. ) ;
#23378 = EDGE_CURVE ( 'NONE', #30087, #17576, #25428, .T. ) ;
#23379 = EDGE_CURVE ( 'NONE', #6014, #3793, #19007, .T. ) ;
#23380 = EDGE_CURVE ( 'NONE', #26115, #21455, #25888, .T. ) ;
#23381 = EDGE_LOOP ( 'NONE', ( #6611, #7074, #15726, #10474, #20719 ) ) ;
#23382 = VECTOR ( 'NONE', #20446, 1000.000000000000000 ) ;
#23383 = CARTESIAN_POINT ( 'NONE',  ( 141.1922820468854525, -1.999999999999978684, -13.59645775552055902 ) ) ;
#23384 = VECTOR ( 'NONE', #25347, 1000.000000000000000 ) ;
#23385 = DIRECTION ( 'NONE',  ( -2.698458740408365879E-16, 1.000000000000000000, 0.000000000000000000 ) ) ;
#23386 = DIRECTION ( 'NONE',  ( -0.9510565162951536422, -2.566386769018988323E-16, 0.3090169943749475623 ) ) ;
#23387 = VECTOR ( 'NONE', #22790, 1000.000000000000000 ) ;
#23388 = VECTOR ( 'NONE', #28987, 1000.000000000000000 ) ;
#23389 = CARTESIAN_POINT ( 'NONE',  ( 10.33811767156285555, 18.38618615532545064, -17.91197029530843565 ) ) ;
#23390 = DIRECTION ( 'NONE',  ( -0.8090169943749474513, -2.183098979609982436E-16, 0.5877852522924731371 ) ) ;
#23391 = ORIENTED_EDGE ( 'NONE', *, *, #27287, .T. ) ;
#23392 = DIRECTION ( 'NONE',  ( -0.5877852522924731371, -1.586114251531760728E-16, -0.8090169943749474513 ) ) ;
#23393 = ORIENTED_EDGE ( 'NONE', *, *, #2274, .F. ) ;
#23394 = CARTESIAN_POINT ( 'NONE',  ( 11.21346931060482000, 10.45895530107994098, -15.96818619734747458 ) ) ;
#23395 = ORIENTED_EDGE ( 'NONE', *, *, #16304, .F. ) ;
#23396 = CARTESIAN_POINT ( 'NONE',  ( 16.52347908691095668, 7.282719431485021211, -19.45954596032283845 ) ) ;
#23397 = CARTESIAN_POINT ( 'NONE',  ( 169.5152310637604955, -4.999999999999971578, -30.37205893520531319 ) ) ;
#23398 = LINE ( 'NONE', #16818, #842 ) ;
#23399 = CARTESIAN_POINT ( 'NONE',  ( 24.87127057246125972, -9.548149280147088191, -14.79180087847266556 ) ) ;
#23400 = ORIENTED_EDGE ( 'NONE', *, *, #6151, .F. ) ;
#23401 = LINE ( 'NONE', #2518, #6159 ) ;
#23402 = CARTESIAN_POINT ( 'NONE',  ( 11.26682494837019277, 16.71987187087499294, -16.78921452078379062 ) ) ;
#23403 = ORIENTED_EDGE ( 'NONE', *, *, #18099, .F. ) ;
#23404 = CARTESIAN_POINT ( 'NONE',  ( 33.98143228033899987, -14.14408878234146982, -18.84191164812894570 ) ) ;
#23405 = CARTESIAN_POINT ( 'NONE',  ( 17.78594395145776019, 10.14170102421038422, -17.68001733040774681 ) ) ;
#23406 = DIRECTION ( 'NONE',  ( -0.9510565162951536422, 0.000000000000000000, -0.3090169943749472292 ) ) ;
#23407 = CARTESIAN_POINT ( 'NONE',  ( 26.37963984661160310, -4.639223599391875119, -13.30093322687953616 ) ) ;
#23408 = ORIENTED_EDGE ( 'NONE', *, *, #6052, .T. ) ;
#23409 = CARTESIAN_POINT ( 'NONE',  ( 130.7287565553229456, -4.999999999999983125, 0.5000000000000052180 ) ) ;
#23410 = SURFACE_SIDE_STYLE ('',( #16380 ) ) ;
#23411 = VECTOR ( 'NONE', #8927, 1000.000000000000000 ) ;
#23412 = CARTESIAN_POINT ( 'NONE',  ( 17.70500667399921824, 3.403337836861581867, -14.36321643528369663 ) ) ;
#23413 = CARTESIAN_POINT ( 'NONE',  ( 18.80816768961129881, 6.772028514247487863, -18.23967922641782380 ) ) ;
#23414 = VECTOR ( 'NONE', #27734, 1000.000000000000000 ) ;
#23415 = ORIENTED_EDGE ( 'NONE', *, *, #6232, .T. ) ;
#23416 = LINE ( 'NONE', #7246, #5376 ) ;
#23417 = EDGE_CURVE ( 'NONE', #6582, #29656, #21599, .T. ) ;
#23418 = ADVANCED_FACE ( 'NONE', ( #28364 ), #9984, .T. ) ;
#23419 = EDGE_CURVE ( 'NONE', #3706, #2025, #23440, .T. ) ;
#23420 = CARTESIAN_POINT ( 'NONE',  ( 157.2287565553230024, -1.999999999999973133, -29.49038105676660493 ) ) ;
#23421 = ORIENTED_EDGE ( 'NONE', *, *, #1318, .T. ) ;
#23422 = EDGE_CURVE ( 'NONE', #26303, #9856, #16862, .T. ) ;
#23423 = AXIS2_PLACEMENT_3D ( 'NONE', #16602, #28542, #16447 ) ;
#23424 = CARTESIAN_POINT ( 'NONE',  ( 172.2287565553229172, -9.999999999999996447, -20.83012701892220520 ) ) ;
#23425 = CARTESIAN_POINT ( 'NONE',  ( 139.5152310637605808, -4.999999999999980460, -1.548930218128858680E-14 ) ) ;
#23426 = AXIS2_PLACEMENT_3D ( 'NONE', #23549, #361, #2054 ) ;
#23427 = DIRECTION ( 'NONE',  ( 0.9510565162951535312, 2.566386769018988816E-16, -0.3090169943749475623 ) ) ;
#23428 = CARTESIAN_POINT ( 'NONE',  ( 9.916637298967875935, 16.40639221407973380, -16.50447193873893781 ) ) ;
#23429 = CARTESIAN_POINT ( 'NONE',  ( 27.79171034377997884, -3.119812929724471662, -15.83729198868751276 ) ) ;
#23430 = CARTESIAN_POINT ( 'NONE',  ( 19.95076809599375878, -1.008983920988137495, -18.52968236344498720 ) ) ;
#23432 = ORIENTED_EDGE ( 'NONE', *, *, #15030, .T. ) ;
#23431 = CARTESIAN_POINT ( 'NONE',  ( 32.19500574710832552, -10.39459394146955518, -19.06308269698291014 ) ) ;
#23434 = DIRECTION ( 'NONE',  ( 0.000000000000000000, 0.000000000000000000, 1.000000000000000000 ) ) ;
#23433 = AXIS2_PLACEMENT_3D ( 'NONE', #10344, #12326, #8204 ) ;
#23435 = CARTESIAN_POINT ( 'NONE',  ( 12.60945047077962933, 8.619070305187777947, -15.04294105552940231 ) ) ;
#23436 = FACE_OUTER_BOUND ( 'NONE', #20945, .T. ) ;
#23437 = CARTESIAN_POINT ( 'NONE',  ( 173.6922820468852535, -4.999999999999971578, -0.6060766987539614181 ) ) ;
#23438 = CARTESIAN_POINT ( 'NONE',  ( 14.73401617531889229, 6.408058468588501810, -15.60580005407095960 ) ) ;
#23439 = ORIENTED_EDGE ( 'NONE', *, *, #3314, .F. ) ;
#23440 = LINE ( 'NONE', #14256, #11982 ) ;
#23441 = CARTESIAN_POINT ( 'NONE',  ( 10.33811693838771717, 18.38618951776012267, -17.91928203681695564 ) ) ;
#23442 = ORIENTED_EDGE ( 'NONE', *, *, #21790, .F. ) ;
#23443 = DIRECTION ( 'NONE',  ( 0.5877852522924731371, 0.000000000000000000, 0.8090169943749474513 ) ) ;
#23444 = CARTESIAN_POINT ( 'NONE',  ( 178.7287565553229172, -1.999999999999968914, 0.5000000000000029976 ) ) ;
#23445 = CARTESIAN_POINT ( 'NONE',  ( 21.41025690189560748, 5.821651141963339882, -16.00656683556521998 ) ) ;
#23446 = ORIENTED_EDGE ( 'NONE', *, *, #5192, .T. ) ;
#23447 = CARTESIAN_POINT ( 'NONE',  ( 27.89044320811645505, -9.967159925860730851, -19.81290489186636350 ) ) ;
#23448 = ORIENTED_EDGE ( 'NONE', *, *, #10002, .F. ) ;
#23450 = AXIS2_PLACEMENT_3D ( 'NONE', #24373, #7734, #17047 ) ;
#23449 = CARTESIAN_POINT ( 'NONE',  ( 34.74206752880779447, -19.56122003402509080, -21.15647653254228189 ) ) ;
#23451 = CARTESIAN_POINT ( 'NONE',  ( 21.82779397375749753, -0.5565768812632180262, -18.88406021698092729 ) ) ;
#23452 = VECTOR ( 'NONE', #26762, 1000.000000000000000 ) ;
#23453 = B_SPLINE_CURVE_WITH_KNOTS ( 'NONE', 3,
 ( #2115, #10940, #11387, #29936, #20692, #9090, #24699, #15524 ),
 .UNSPECIFIED., .F., .F.,
 ( 4, 2, 2, 4 ),
 ( 0.004673709593152148775, 0.005837709341827642534, 0.007001709090503135426, 0.009329708587854122076 ),
 .UNSPECIFIED. ) ;
#23454 = CARTESIAN_POINT ( 'NONE',  ( 19.48014203372339992, 3.175912578606837844, -18.88683143354647243 ) ) ;
#23455 = CARTESIAN_POINT ( 'NONE',  ( 25.37029659992048281, -10.87484012800900501, -14.78472363349550811 ) ) ;
#23456 = EDGE_CURVE ( 'NONE', #2040, #1623, #5273, .T. ) ;
#23457 = VERTEX_POINT ( 'NONE', #19299 ) ;
#23458 = ADVANCED_FACE ( 'NONE', ( #11969, #14560 ), #21288, .F. ) ;
#23459 = PLANE ( 'NONE',  #27489 ) ;
#23460 = ADVANCED_FACE ( 'NONE', ( #9682 ), #11823, .T. ) ;
#23461 = CARTESIAN_POINT ( 'NONE',  ( 137.0152310637606092, -10.00000000000000533, -24.27857615940569147 ) ) ;
#23462 = DIRECTION ( 'NONE',  ( -0.9510565162951536422, 0.000000000000000000, -0.3090169943749472292 ) ) ;
#23463 = DIRECTION ( 'NONE',  ( 0.000000000000000000, 0.000000000000000000, -1.000000000000000000 ) ) ;
#23464 = CARTESIAN_POINT ( 'NONE',  ( 36.49521523454778560, -20.94471372247522467, -19.05937150832556526 ) ) ;
#23465 = AXIS2_PLACEMENT_3D ( 'NONE', #26969, #22658, #18066 ) ;
#23466 = CARTESIAN_POINT ( 'NONE',  ( 12.77299770905688803, 7.633314995549595139, -14.91259101981587420 ) ) ;
#23467 = VERTEX_POINT ( 'NONE', #25731 ) ;
#23468 = PLANE ( 'NONE',  #6378 ) ;
#23469 = DIRECTION ( 'NONE',  ( 1.110223024625156540E-16, 2.995891024602366092E-32, 1.000000000000000000 ) ) ;
#23470 = CARTESIAN_POINT ( 'NONE',  ( 10.47604570704546845, 16.43372961628045559, -17.33313991065496751 ) ) ;
#23471 = FACE_OUTER_BOUND ( 'NONE', #674, .T. ) ;
#23472 = ORIENTED_EDGE ( 'NONE', *, *, #27005, .T. ) ;
#23473 = CARTESIAN_POINT ( 'NONE',  ( 122.6304986437925209, -4.999999999999984901, -89.09627249521899728 ) ) ;
#23474 = ORIENTED_EDGE ( 'NONE', *, *, #24908, .T. ) ;
#23475 = LINE ( 'NONE', #4413, #17811 ) ;
#23476 = PLANE ( 'NONE',  #16597 ) ;
#23477 = ORIENTED_EDGE ( 'NONE', *, *, #28318, .T. ) ;
#23478 = CARTESIAN_POINT ( 'NONE',  ( 18.54986643893153442, -5.000000000000012434, -57.09061855589936840 ) ) ;
#23479 = EDGE_LOOP ( 'NONE', ( #23317, #23400, #8522, #3143 ) ) ;
#23480 = CARTESIAN_POINT ( 'NONE',  ( 9.992064777962580635, 14.74057119405591543, -17.75100935390776158 ) ) ;
#23481 = EDGE_CURVE ( 'NONE', #24269, #24460, #23748, .T. ) ;
#23482 = ORIENTED_EDGE ( 'NONE', *, *, #6856, .F. ) ;
#23483 = CARTESIAN_POINT ( 'NONE',  ( 25.59007283008577005, -3.201708215360036913, -15.56755918271449168 ) ) ;
#23484 = CARTESIAN_POINT ( 'NONE',  ( 16.03657434348277633, 2.746931742562784162, -16.83325620853174698 ) ) ;
#23485 = CARTESIAN_POINT ( 'NONE',  ( 149.5152310637605240, -10.00000000000000178, -13.05155085951651195 ) ) ;
#23486 = LINE ( 'NONE', #16156, #10154 ) ;
#23487 = CARTESIAN_POINT ( 'NONE',  ( 134.7287565553230024, -4.999999999999981348, -7.839745962155600267 ) ) ;
#23488 = CARTESIAN_POINT ( 'NONE',  ( 26.58455406938135468, -5.910422570377376950, -13.89432871846328688 ) ) ;
#23489 = DIRECTION ( 'NONE',  ( 0.000000000000000000, 0.000000000000000000, -1.000000000000000000 ) ) ;
#23490 = LINE ( 'NONE', #2600, #21408 ) ;
#23491 = VECTOR ( 'NONE', #2985, 1000.000000000000000 ) ;
#23492 = DIRECTION ( 'NONE',  ( 0.3090169943749472292, 8.338696094057992503E-17, -0.9510565162951536422 ) ) ;
#23493 = FACE_OUTER_BOUND ( 'NONE', #236, .T. ) ;
#23494 = CARTESIAN_POINT ( 'NONE',  ( 10.47705880869930084, 16.42908340295556258, -17.33272095748315422 ) ) ;
#23495 = CARTESIAN_POINT ( 'NONE',  ( 35.54859390953724585, -22.18451583373416014, -16.94733705004010460 ) ) ;
#23496 = CARTESIAN_POINT ( 'NONE',  ( 33.68411698100747032, -13.80840863474736935, -19.79436191385186916 ) ) ;
#23497 = EDGE_LOOP ( 'NONE', ( #24736, #29816, #11406, #13826 ) ) ;
#23498 = CARTESIAN_POINT ( 'NONE',  ( 13.37894900189793290, 7.625660844661456217, -15.70840104182326513 ) ) ;
#23499 = ORIENTED_EDGE ( 'NONE', *, *, #25211, .T. ) ;
#23500 = PLANE ( 'NONE',  #22707 ) ;
#23501 = VECTOR ( 'NONE', #4459, 1000.000000000000000 ) ;
#23502 = CARTESIAN_POINT ( 'NONE',  ( 16.89609864265585060, 4.102175112930991574, -14.31125941877678720 ) ) ;
#23503 = CARTESIAN_POINT ( 'NONE',  ( 11.27636807789780171, 16.67610586239533177, -16.78445215232725118 ) ) ;
#23504 = FACE_BOUND ( 'NONE', #12698, .T. ) ;
#23505 = ORIENTED_EDGE ( 'NONE', *, *, #15257, .T. ) ;
#23506 = ORIENTED_EDGE ( 'NONE', *, *, #9021, .T. ) ;
#23507 = CARTESIAN_POINT ( 'NONE',  ( 9.675370519060759733, 17.51287242109451014, -17.23928541814325399 ) ) ;
#23508 = FACE_OUTER_BOUND ( 'NONE', #25841, .T. ) ;
#23509 = CARTESIAN_POINT ( 'NONE',  ( 9.675370519060759733, 17.51287242109451014, -17.23928541814325399 ) ) ;
#23510 = DIRECTION ( 'NONE',  ( 0.000000000000000000, -1.000000000000000000, 0.000000000000000000 ) ) ;
#23511 = CARTESIAN_POINT ( 'NONE',  ( 169.5152310637604387, -9.999999999999996447, -2.627941064794695691 ) ) ;
#23512 = ORIENTED_EDGE ( 'NONE', *, *, #23210, .T. ) ;
#23513 = DIRECTION ( 'NONE',  ( -1.000000000000000000, -0.000000000000000000, -1.387778780781445922E-16 ) ) ;
#23514 = VERTEX_POINT ( 'NONE', #250 ) ;
#23515 = CARTESIAN_POINT ( 'NONE',  ( 10.35865474790814211, 16.97209951875106526, -17.91014213605047445 ) ) ;
#23516 = EDGE_CURVE ( 'NONE', #25495, #18619, #26194, .T. ) ;
#23517 = ORIENTED_EDGE ( 'NONE', *, *, #9202, .T. ) ;
#23518 = CARTESIAN_POINT ( 'NONE',  ( 36.13838427452936486, -20.34166123773320578, -20.43658233646779365 ) ) ;
#23519 = CARTESIAN_POINT ( 'NONE',  ( 31.59793210864275537, -10.01186915388335485, -14.42687813506083039 ) ) ;
#23520 = CARTESIAN_POINT ( 'NONE',  ( 26.18758235895636233, -4.355437658720127558, -18.53605802859044260 ) ) ;
#23521 = ORIENTED_EDGE ( 'NONE', *, *, #20924, .T. ) ;
#23522 = EDGE_CURVE ( 'NONE', #19955, #23305, #3003, .T. ) ;
#23523 = AXIS2_PLACEMENT_3D ( 'NONE', #7803, #19389, #22134 ) ;
#23524 = LINE ( 'NONE', #5205, #22326 ) ;
#23525 = VERTEX_POINT ( 'NONE', #7711 ) ;
#23526 = CARTESIAN_POINT ( 'NONE',  ( 33.78657425947636739, -10.78854458652579495, -19.16640759269550287 ) ) ;
#23527 = DIRECTION ( 'NONE',  ( 0.000000000000000000, 0.000000000000000000, 1.000000000000000000 ) ) ;
#23528 = CARTESIAN_POINT ( 'NONE',  ( 16.80936620776159884, 5.784822248606665163, -14.58992565756060245 ) ) ;
#23529 = CARTESIAN_POINT ( 'NONE',  ( 15.19603151210977821, 9.502094893032342782, -14.87270315361914896 ) ) ;
#23530 = B_SPLINE_CURVE_WITH_KNOTS ( 'NONE', 3,
 ( #5994, #24613, #6293, #22322, #10408, #3270 ),
 .UNSPECIFIED., .F., .F.,
 ( 4, 2, 4 ),
 ( 0.008240550023493525833, 0.01057684187039405893, 0.01291313371729459203 ),
 .UNSPECIFIED. ) ;
#23531 = VECTOR ( 'NONE', #9959, 1000.000000000000000 ) ;
#23532 = VERTEX_POINT ( 'NONE', #17020 ) ;
#23533 = CARTESIAN_POINT ( 'NONE',  ( 153.6922820468853672, -10.00000000000000178, -6.413161187712876909 ) ) ;
#23534 = VERTEX_POINT ( 'NONE', #94 ) ;
#23535 = CARTESIAN_POINT ( 'NONE',  ( 161.1922820468853956, -1.999999999999972689, -30.91696583120936026 ) ) ;
#23536 = LINE ( 'NONE', #7506, #953 ) ;
#23537 = VECTOR ( 'NONE', #19649, 1000.000000000000000 ) ;
#23538 = CARTESIAN_POINT ( 'NONE',  ( 162.2287565553229172, -9.999999999999998224, -12.16987298107780369 ) ) ;
#23539 = PRODUCT_DEFINITION_CONTEXT ( 'detailed design', #15530, 'design' ) ;
#23540 = CARTESIAN_POINT ( 'NONE',  ( 10.33886748782435561, 18.38274740237080351, -17.79416814676874381 ) ) ;
#23541 = PLANE ( 'NONE',  #5857 ) ;
#23542 = CARTESIAN_POINT ( 'NONE',  ( 134.7287565553230024, -1.999999999999980460, 0.8205080756887930260 ) ) ;
#23543 = VERTEX_POINT ( 'NONE', #18849 ) ;
#23544 = CARTESIAN_POINT ( 'NONE',  ( 11.47257016429183452, 9.270685755423764718, -15.86103888016343255 ) ) ;
#23545 = VERTEX_POINT ( 'NONE', #28210 ) ;
#23546 = CARTESIAN_POINT ( 'NONE',  ( 9.662623034719734605, 16.25143302262299372, -17.90105808085208849 ) ) ;
#23547 = VECTOR ( 'NONE', #16767, 1000.000000000000000 ) ;
#23548 = CARTESIAN_POINT ( 'NONE',  ( 17.00905032053054811, 4.985101812230166907, -18.82491780458422781 ) ) ;
#23549 = CARTESIAN_POINT ( 'NONE',  ( -19.99999999999999289, 60.00000000000000711, -25.00000000000000000 ) ) ;
#23550 = DIRECTION ( 'NONE',  ( 0.000000000000000000, 0.000000000000000000, 1.000000000000000000 ) ) ;
#23551 = CARTESIAN_POINT ( 'NONE',  ( 24.68825858685077179, -9.385095155728059524, -16.92495907518576104 ) ) ;
#23552 = VERTEX_POINT ( 'NONE', #26344 ) ;
#23553 = CARTESIAN_POINT ( 'NONE',  ( 171.1922820468853104, -1.999999999999970468, -10.74328820663507678 ) ) ;
#23554 = CARTESIAN_POINT ( 'NONE',  ( 11.05558847800967648, 17.68862925033535660, -17.87192865789842955 ) ) ;
#23555 = ORIENTED_EDGE ( 'NONE', *, *, #18303, .F. ) ;
#23556 = EDGE_CURVE ( 'NONE', #7790, #3713, #19154, .T. ) ;
#23557 = CARTESIAN_POINT ( 'NONE',  ( 35.54859306210901337, -21.18451202668684985, -18.38798429269037271 ) ) ;
#23558 = PLANE ( 'NONE',  #4922 ) ;
#23559 = EDGE_LOOP ( 'NONE', ( #25145, #23021, #11776, #28982, #19372, #14378 ) ) ;
#23560 = ADVANCED_FACE ( 'NONE', ( #557 ), #9841, .T. ) ;
#23561 = LINE ( 'NONE', #12098, #18393 ) ;
#23562 = EDGE_CURVE ( 'NONE', #23077, #10756, #9379, .T. ) ;
#23563 = CARTESIAN_POINT ( 'NONE',  ( 30.62308825650849187, -7.210737555064373083, -14.15269394828060889 ) ) ;
#23564 = ORIENTED_EDGE ( 'NONE', *, *, #17707, .T. ) ;
#23565 = CARTESIAN_POINT ( 'NONE',  ( 89.72970066344139184, -4.999999999999992895, 65.19244355718100792 ) ) ;
#23566 = CARTESIAN_POINT ( 'NONE',  ( 19.30972751531945519, 5.994221256738944348, -19.84686166629000326 ) ) ;
#23567 = CARTESIAN_POINT ( 'NONE',  ( 14.65865118920550714, 8.193166376910747672, -14.78953851775792216 ) ) ;
#23568 = ORIENTED_EDGE ( 'NONE', *, *, #1581, .F. ) ;
#23569 = B_SPLINE_CURVE_WITH_KNOTS ( 'NONE', 3,
 ( #26074, #28240, #7296, #7589, #28395, #25921 ),
 .UNSPECIFIED., .F., .F.,
 ( 4, 2, 4 ),
 ( 0.006456566858647419180, 0.007625406818786685526, 0.008794246778925951871 ),
 .UNSPECIFIED. ) ;
#23570 = DIRECTION ( 'NONE',  ( 1.000000000000000000, 0.000000000000000000, 0.000000000000000000 ) ) ;
#23571 = VECTOR ( 'NONE', #23572, 1000.000000000000000 ) ;
#23572 = DIRECTION ( 'NONE',  ( 0.000000000000000000, 0.000000000000000000, 1.000000000000000000 ) ) ;
#23573 = ORIENTED_EDGE ( 'NONE', *, *, #19383, .T. ) ;
#23574 = CARTESIAN_POINT ( 'NONE',  ( 169.5152310637605240, -1.999999999999970024, -28.60870317832789667 ) ) ;
#23575 = CARTESIAN_POINT ( 'NONE',  ( 147.0152310637605240, -10.00000000000000178, -8.721423840594312082 ) ) ;
#23576 = CARTESIAN_POINT ( 'NONE',  ( -4.000000000000008882, 6.928203230275508773, 0.000000000000000000 ) ) ;
#23577 = CARTESIAN_POINT ( 'NONE',  ( 9.641350810849047548, 17.66889113945805789, -17.91796598306941135 ) ) ;
#23578 = CARTESIAN_POINT ( 'NONE',  ( 18.80130396411469462, -1.975481315223051704, -14.30362724594584378 ) ) ;
#23579 = CARTESIAN_POINT ( 'NONE',  ( 19.39950943988042553, -1.649204456521256246, -16.58530004841527727 ) ) ;
#23581 = ORIENTED_EDGE ( 'NONE', *, *, #26991, .T. ) ;
#23580 = CARTESIAN_POINT ( 'NONE',  ( 36.52535953212831998, -23.08013608362457703, -19.17046861472280028 ) ) ;
#23582 = FACE_OUTER_BOUND ( 'NONE', #25151, .T. ) ;
#23583 = CARTESIAN_POINT ( 'NONE',  ( 138.6922820468854525, -10.00000000000000533, -17.92658477444275533 ) ) ;
#23584 = DIRECTION ( 'NONE',  ( 0.9510565162951535312, 2.566386769018988816E-16, -0.3090169943749475623 ) ) ;
#23585 = DIRECTION ( 'NONE',  ( 1.110223024625156540E-16, 2.995891024602366092E-32, 1.000000000000000000 ) ) ;
#23586 = CARTESIAN_POINT ( 'NONE',  ( 17.12833724908345800, 9.171387755021909172, -19.38714867094073213 ) ) ;
#23587 = ORIENTED_EDGE ( 'NONE', *, *, #1847, .F. ) ;
#23588 = CARTESIAN_POINT ( 'NONE',  ( 172.0152310637604671, -9.999999999999994671, -26.04193191628311155 ) ) ;
#23589 = CARTESIAN_POINT ( 'NONE',  ( 10.33812866905494587, 18.38613571942487113, -17.90056368370468931 ) ) ;
#23590 = ORIENTED_EDGE ( 'NONE', *, *, #17441, .F. ) ;
#23591 = CARTESIAN_POINT ( 'NONE',  ( 138.6922820468854241, -4.999999999999980460, -0.6060766987539614181 ) ) ;
#23592 = CARTESIAN_POINT ( 'NONE',  ( 8.531849494005609102, -5.000000000000015099, 26.25833272935806662 ) ) ;
#23593 = EDGE_CURVE ( 'NONE', #11963, #3548, #10434, .T. ) ;
#23594 = CARTESIAN_POINT ( 'NONE',  ( 19.11618317516819587, 7.271703427217982352, -19.10559232466456692 ) ) ;
#23595 = VECTOR ( 'NONE', #14915, 1000.000000000000000 ) ;
#23596 = ADVANCED_FACE ( 'NONE', ( #17310 ), #26649, .F. ) ;
#23597 = EDGE_CURVE ( 'NONE', #19084, #9938, #2745, .T. ) ;
#23598 = CARTESIAN_POINT ( 'NONE',  ( 32.75486304968715245, -9.956179044816899193, -14.71053347703266212 ) ) ;
#23599 = ORIENTED_EDGE ( 'NONE', *, *, #3281, .T. ) ;
#23600 = EDGE_CURVE ( 'NONE', #7514, #13296, #17815, .T. ) ;
#23601 = CARTESIAN_POINT ( 'NONE',  ( 35.54859569580823830, -22.18452385850428499, -18.27063337037174762 ) ) ;
#23602 = CARTESIAN_POINT ( 'NONE',  ( 23.33733100364600688, 1.020658515592549609, -17.81090727445316446 ) ) ;
#23603 = CARTESIAN_POINT ( 'NONE',  ( 16.84916689134472989, 3.454690908320265041, -17.64892000621457413 ) ) ;
#23604 = VERTEX_POINT ( 'NONE', #5729 ) ;
#23605 = CARTESIAN_POINT ( 'NONE',  ( 28.24905293252005123, -11.45655955306129314, -17.88756844200554141 ) ) ;
#23606 = ORIENTED_EDGE ( 'NONE', *, *, #14236, .T. ) ;
#23607 = ORIENTED_EDGE ( 'NONE', *, *, #26927, .F. ) ;
#23608 = LINE ( 'NONE', #10153, #6977 ) ;
#23610 = ORIENTED_EDGE ( 'NONE', *, *, #25412, .F. ) ;
#23609 = LINE ( 'NONE', #25585, #27318 ) ;
#23611 = DIRECTION ( 'NONE',  ( 0.000000000000000000, 0.000000000000000000, 1.000000000000000000 ) ) ;
#23612 = AXIS2_PLACEMENT_3D ( 'NONE', #26369, #574, #12152 ) ;
#23613 = LINE ( 'NONE', #25753, #14603 ) ;
#23614 = CARTESIAN_POINT ( 'NONE',  ( 36.54517214193456454, -21.16914364445853280, -18.53042016804813841 ) ) ;
#23615 = CARTESIAN_POINT ( 'NONE',  ( 12.75629879507850717, 7.625935294889710114, -14.92590036059129943 ) ) ;
#23616 = ORIENTED_EDGE ( 'NONE', *, *, #14093, .T. ) ;
#23617 = CARTESIAN_POINT ( 'NONE',  ( 0.000000000000000000, 60.00000000000000711, 0.000000000000000000 ) ) ;
#23618 = LINE ( 'NONE', #19034, #5655 ) ;
#23619 = CARTESIAN_POINT ( 'NONE',  ( 11.94706930840425407, 9.687427868553587729, -16.72481990518296158 ) ) ;
#23620 = DIRECTION ( 'NONE',  ( 0.000000000000000000, -0.4999999999999992784, 0.8660254037844389297 ) ) ;
#23621 = ORIENTED_EDGE ( 'NONE', *, *, #22317, .T. ) ;
#23622 = DIRECTION ( 'NONE',  ( 0.000000000000000000, 2.775557561562890735E-17, -1.000000000000000000 ) ) ;
#23623 = ORIENTED_EDGE ( 'NONE', *, *, #20544, .F. ) ;
#23624 = ORIENTED_EDGE ( 'NONE', *, *, #178, .T. ) ;
#23625 = DIRECTION ( 'NONE',  ( -0.5877852522924731371, -1.586114251531760235E-16, 0.8090169943749474513 ) ) ;
#23626 = EDGE_CURVE ( 'NONE', #7033, #6062, #29430, .T. ) ;
#23627 = CARTESIAN_POINT ( 'NONE',  ( 167.0152310637605240, -1.999999999999970912, -24.27857615940569502 ) ) ;
#23628 = ORIENTED_EDGE ( 'NONE', *, *, #15235, .F. ) ;
#23629 = EDGE_CURVE ( 'NONE', #21885, #705, #30092, .T. ) ;
#23630 = DIRECTION ( 'NONE',  ( 0.000000000000000000, 0.000000000000000000, 1.000000000000000000 ) ) ;
#23631 = EDGE_LOOP ( 'NONE', ( #28974, #28543, #2923, #18137 ) ) ;
#23632 = EDGE_CURVE ( 'NONE', #19861, #10906, #6026, .T. ) ;
#23633 = CARTESIAN_POINT ( 'NONE',  ( 9.668505437271095460, 16.22445557469016464, -17.88481252315560965 ) ) ;
#23634 = CARTESIAN_POINT ( 'NONE',  ( 24.61983070264756890, -3.485318192270607351, -14.59657465048590907 ) ) ;
#23635 = ORIENTED_EDGE ( 'NONE', *, *, #138, .T. ) ;
#23636 = CARTESIAN_POINT ( 'NONE',  ( 20.75491211191951635, -1.144232541536293946, -14.27023797479654554 ) ) ;
#23637 = CARTESIAN_POINT ( 'NONE',  ( 169.7287565553228603, -9.999999999999998224, 0.8205080756887930260 ) ) ;
#23638 = LINE ( 'NONE', #7010, #5289 ) ;
#23639 = VECTOR ( 'NONE', #6916, 1000.000000000000000 ) ;
#23640 = DIRECTION ( 'NONE',  ( -0.9510565162951536422, -2.566386769018988323E-16, 0.3090169943749475623 ) ) ;
#23641 = CARTESIAN_POINT ( 'NONE',  ( 26.61709978538234012, -3.831456866606135492, -17.85214630790261836 ) ) ;
#23642 = VERTEX_POINT ( 'NONE', #17609 ) ;
#23643 = FILL_AREA_STYLE_COLOUR ( '', #24212 ) ;
#23644 = CARTESIAN_POINT ( 'NONE',  ( 131.1922820468854241, -10.00000000000000888, -19.40354224447947473 ) ) ;
#23645 = CARTESIAN_POINT ( 'NONE',  ( 169.5152310637604955, -9.999999999999994671, -30.37205893520531319 ) ) ;
#23646 = CARTESIAN_POINT ( 'NONE',  ( 156.1922820468853672, -1.999999999999974909, -13.59645775552055902 ) ) ;
#23647 = LINE ( 'NONE', #9591, #199 ) ;
#23648 = CARTESIAN_POINT ( 'NONE',  ( 11.98759337455738816, 9.501579335558542283, -16.70806177831036976 ) ) ;
#23649 = DIRECTION ( 'NONE',  ( -2.698458740408365879E-16, 1.000000000000000000, 0.000000000000000000 ) ) ;
#23650 = CARTESIAN_POINT ( 'NONE',  ( 34.75406370242679799, -18.61511248754081294, -20.11778113987843852 ) ) ;
#23651 = ORIENTED_EDGE ( 'NONE', *, *, #4059, .F. ) ;
#23652 = CARTESIAN_POINT ( 'NONE',  ( 8.944605280299260386, 16.95149830073946617, -17.90242062344065843 ) ) ;
#23653 = ORIENTED_EDGE ( 'NONE', *, *, #11481, .T. ) ;
#23654 = CARTESIAN_POINT ( 'NONE',  ( 137.0152310637606092, -1.999999999999979572, -6.958068083716895558 ) ) ;
#23655 = VECTOR ( 'NONE', #16319, 1000.000000000000000 ) ;
#23656 = CARTESIAN_POINT ( 'NONE',  ( 23.66601916330066402, 2.199037240492611733, -18.57254039386976885 ) ) ;
#23657 = CARTESIAN_POINT ( 'NONE',  ( 12.83257874964047929, 9.539242390270068483, -16.14089537112711525 ) ) ;
#23658 = FACE_BOUND ( 'NONE', #7663, .T. ) ;
#23659 = ORIENTED_EDGE ( 'NONE', *, *, #12338, .F. ) ;
#23660 = VERTEX_POINT ( 'NONE', #20056 ) ;
#23661 = CARTESIAN_POINT ( 'NONE',  ( 9.870716668364401869, 16.61699007954640805, -16.53972800451630931 ) ) ;
#23662 = DIRECTION ( 'NONE',  ( -2.698458740408365879E-16, 1.000000000000000000, 0.000000000000000000 ) ) ;
#23663 = CARTESIAN_POINT ( 'NONE',  ( 9.997747326010761881, 16.03441129093729245, -16.47093000352221637 ) ) ;
#23664 = DIRECTION ( 'NONE',  ( 0.8191520442889924647, 4.640937770007144753E-16, -0.5735764363510452712 ) ) ;
#23665 = EDGE_LOOP ( 'NONE', ( #29259, #14639, #15058, #21786 ) ) ;
#23666 = DIRECTION ( 'NONE',  ( 0.000000000000000000, 0.000000000000000000, 1.000000000000000000 ) ) ;
#23667 = EDGE_LOOP ( 'NONE', ( #25758, #4546, #20577, #263 ) ) ;
#23668 = EDGE_CURVE ( 'NONE', #3067, #15263, #12576, .T. ) ;
#23669 = CARTESIAN_POINT ( 'NONE',  ( 10.60167031212029443, 15.85759916399494607, -17.28118971735050735 ) ) ;
#23670 = VECTOR ( 'NONE', #15799, 1000.000000000000000 ) ;
#23671 = ORIENTED_EDGE ( 'NONE', *, *, #5398, .F. ) ;
#23672 = CARTESIAN_POINT ( 'NONE',  ( 36.18478257229246964, -20.55010421171508028, -20.40673782175607442 ) ) ;
#23673 = CARTESIAN_POINT ( 'NONE',  ( 29.46565128511723586, -7.689737916804423534, -14.82739468409561567 ) ) ;
#23674 = CARTESIAN_POINT ( 'NONE',  ( 14.45328171724474231, 7.053988074037379263, -14.59236433646538522 ) ) ;
#23675 = EDGE_LOOP ( 'NONE', ( #3253, #5968, #21206, #15841 ) ) ;
#23676 = CARTESIAN_POINT ( 'NONE',  ( 0.000000000000000000, 0.000000000000000000, 9.999999999999998224 ) ) ;
#23677 = CARTESIAN_POINT ( 'NONE',  ( 34.91913293194685508, -14.86421081092256280, -20.09741683264573808 ) ) ;
#23678 =( NAMED_UNIT ( * ) SI_UNIT ( $, .STERADIAN. ) SOLID_ANGLE_UNIT ( ) );
#23679 = CARTESIAN_POINT ( 'NONE',  ( 17.54325408622900184, 7.715740848240963068, -20.30207397218512000 ) ) ;
#23680 = AXIS2_PLACEMENT_3D ( 'NONE', #9563, #881, #21321 ) ;
#23681 = CARTESIAN_POINT ( 'NONE',  ( 27.63516133065608926, -10.68623331565014034, -17.71408682504818088 ) ) ;
#23682 = VECTOR ( 'NONE', #24985, 1000.000000000000000 ) ;
#23683 = ORIENTED_EDGE ( 'NONE', *, *, #7605, .F. ) ;
#23684 = ORIENTED_EDGE ( 'NONE', *, *, #22460, .F. ) ;
#23685 = PLANE ( 'NONE',  #13760 ) ;
#23686 = EDGE_CURVE ( 'NONE', #14621, #23525, #22053, .T. ) ;
#23687 = LINE ( 'NONE', #642, #7721 ) ;
#23688 = DIRECTION ( 'NONE',  ( 0.5877852522924731371, 1.586114251531760728E-16, -0.8090169943749474513 ) ) ;
#23689 = CARTESIAN_POINT ( 'NONE',  ( 130.7287565553229172, -4.999999999999983125, -36.50000000000000711 ) ) ;
#23690 = LINE ( 'NONE', #23538, #1732 ) ;
#23691 = VECTOR ( 'NONE', #29473, 1000.000000000000000 ) ;
#23692 = CARTESIAN_POINT ( 'NONE',  ( 10.33830461362823883, 18.38532881518400686, -17.85494544563047370 ) ) ;
#23693 = DIRECTION ( 'NONE',  ( 0.9510565162951535312, 2.566386769018988816E-16, -0.3090169943749475623 ) ) ;
#23694 = PLANE ( 'NONE',  #9081 ) ;
#23695 = VERTEX_POINT ( 'NONE', #1155 ) ;
#23696 = VECTOR ( 'NONE', #5115, 1000.000000000000000 ) ;
#23697 = CARTESIAN_POINT ( 'NONE',  ( 9.918725397012197575, 16.39681593027784956, -16.50360835092378409 ) ) ;
#23698 = ORIENTED_EDGE ( 'NONE', *, *, #28910, .F. ) ;
#23699 = CARTESIAN_POINT ( 'NONE',  ( 9.667845848563926481, 16.22748053257927126, -17.88508528815513543 ) ) ;
#23700 = AXIS2_PLACEMENT_3D ( 'NONE', #27512, #1548, #20439 ) ;
#23701 = CARTESIAN_POINT ( 'NONE',  ( 23.16309603597909472, 3.730466837354933674, -16.34659541137592598 ) ) ;
#23702 = CARTESIAN_POINT ( 'NONE',  ( 133.6922820468854241, -1.999999999999981348, -35.24709285013155835 ) ) ;
#23703 = CARTESIAN_POINT ( 'NONE',  ( 83.60744220746381927, -4.999999999999994671, 60.74436242147287146 ) ) ;
#23705 = ORIENTED_EDGE ( 'NONE', *, *, #13073, .T. ) ;
#23704 = CARTESIAN_POINT ( 'NONE',  ( 24.78692427941192733, -9.284778175067517125, -17.23615439686343720 ) ) ;
#23706 = VERTEX_POINT ( 'NONE', #22192 ) ;
#23707 = CARTESIAN_POINT ( 'NONE',  ( 118.0894766101636719, -4.999999999999985789, -85.79702686717824633 ) ) ;
#23708 = CARTESIAN_POINT ( 'NONE',  ( 11.05584814685795081, 17.68743837589741830, -17.84564518929906285 ) ) ;
#23709 = VERTEX_POINT ( 'NONE', #15309 ) ;
#23710 = CARTESIAN_POINT ( 'NONE',  ( 34.33808118748100924, -15.74632339993765484, -18.94971805680347998 ) ) ;
#23711 = CARTESIAN_POINT ( 'NONE',  ( 16.09764958744793262, 8.143416238145906760, -19.84970969296679044 ) ) ;
#23712 = CARTESIAN_POINT ( 'NONE',  ( 153.6922820468854525, -10.00000000000000000, -35.24709285013155835 ) ) ;
#23713 = CARTESIAN_POINT ( 'NONE',  ( 9.026809008904539411, 16.57450152281700184, -17.18797639273109112 ) ) ;
#23714 = CARTESIAN_POINT ( 'NONE',  ( 31.07149168920019733, -7.992644923617350905, -17.88177209202816087 ) ) ;
#23715 = VERTEX_POINT ( 'NONE', #8152 ) ;
#23716 = DIRECTION ( 'NONE',  ( 2.908569913943825554E-16, -1.000000000000000000, 0.000000000000000000 ) ) ;
#23717 = SHAPE_REPRESENTATION_RELATIONSHIP ( 'NONE' , 'NONE' ,  #29092, #21 ) ;
#23718 = CARTESIAN_POINT ( 'NONE',  ( 17.40782953567980229, 3.270613820851801190, -14.52895612053623609 ) ) ;
#23719 = CARTESIAN_POINT ( 'NONE',  ( 15.96855819401819865, 6.783166013289068985, -19.29613786212107840 ) ) ;
#23720 = CONICAL_SURFACE ( 'NONE', #21264, 4.000000000000003553, 1.047197551196597853 ) ;
#23721 = ORIENTED_EDGE ( 'NONE', *, *, #20037, .T. ) ;
#23722 = DIRECTION ( 'NONE',  ( -2.698458740408365879E-16, 1.000000000000000000, 0.000000000000000000 ) ) ;
#23723 = ORIENTED_EDGE ( 'NONE', *, *, #21856, .F. ) ;
#23724 = ORIENTED_EDGE ( 'NONE', *, *, #446, .F. ) ;
#23725 = FACE_OUTER_BOUND ( 'NONE', #23665, .T. ) ;
#23726 = VECTOR ( 'NONE', #6327, 1000.000000000000000 ) ;
#23727 = VECTOR ( 'NONE', #11182, 1000.000000000000000 ) ;
#23728 = CARTESIAN_POINT ( 'NONE',  ( 167.0152310637604103, -1.999999999999972244, -0.06116980274991495881 ) ) ;
#23729 = EDGE_CURVE ( 'NONE', #29571, #25565, #1010, .T. ) ;
#23730 = EDGE_CURVE ( 'NONE', #17680, #7231, #3301, .T. ) ;
#23731 = CARTESIAN_POINT ( 'NONE',  ( 1.318516776095786991, 3.857556137907067750, -2.450000000000006395 ) ) ;
#23732 = LINE ( 'NONE', #28350, #22370 ) ;
#23733 = EDGE_CURVE ( 'NONE', #25583, #10712, #19743, .T. ) ;
#23734 = LINE ( 'NONE', #23894, #19241 ) ;
#23735 = ADVANCED_FACE ( 'NONE', ( #13035 ), #5880, .T. ) ;
#23736 = CARTESIAN_POINT ( 'NONE',  ( 9.916775705961365261, 16.40575746196480011, -16.50441451066904364 ) ) ;
#23737 = CARTESIAN_POINT ( 'NONE',  ( 25.65469514739125856, -9.762610920096198797, -17.09127189072687614 ) ) ;
#23738 = CARTESIAN_POINT ( 'NONE',  ( 20.49605984403359216, -1.259233478192978373, -14.44550164344372511 ) ) ;
#23740 = ORIENTED_EDGE ( 'NONE', *, *, #18897, .T. ) ;
#23739 = CARTESIAN_POINT ( 'NONE',  ( 33.52946124453396237, -14.11362233419136381, -20.78993474304632372 ) ) ;
#23741 = DIRECTION ( 'NONE',  ( 0.5877852522924731371, 1.586114251531760728E-16, 0.8090169943749474513 ) ) ;
#23742 = CARTESIAN_POINT ( 'NONE',  ( 132.2287565553230024, -1.999999999999981348, -12.16987298107780013 ) ) ;
#23743 = AXIS2_PLACEMENT_3D ( 'NONE', #27725, #29895, #9046 ) ;
#23744 = LINE ( 'NONE', #2841, #13653 ) ;
#23745 = FACE_OUTER_BOUND ( 'NONE', #24379, .T. ) ;
#23746 = CARTESIAN_POINT ( 'NONE',  ( 16.77165338796101324, 10.12286561294300569, -15.51291369241808304 ) ) ;
#23747 = ORIENTED_EDGE ( 'NONE', *, *, #17787, .T. ) ;
#23748 = LINE ( 'NONE', #16720, #18806 ) ;
#23749 = CARTESIAN_POINT ( 'NONE',  ( 10.33811723165831786, 18.38618817278374706, -17.91339614244408907 ) ) ;
#23750 = DIRECTION ( 'NONE',  ( -2.698458740408365879E-16, 1.000000000000000000, 0.000000000000000000 ) ) ;
#23751 = CARTESIAN_POINT ( 'NONE',  ( 158.6922820468853388, -10.00000000000000000, -9.266330736598359152 ) ) ;
#23752 = VECTOR ( 'NONE', #8487, 1000.000000000000000 ) ;
#23753 = CARTESIAN_POINT ( 'NONE',  ( 17.63704213852533442, 9.806822523219006271, -18.50018230520716145 ) ) ;
#23754 = CARTESIAN_POINT ( 'NONE',  ( 30.27995308908331751, -6.828448725465094959, -15.78586218199752622 ) ) ;
#23755 = VERTEX_POINT ( 'NONE', #24497 ) ;
#23756 = CARTESIAN_POINT ( 'NONE',  ( 34.54007435814109783, -17.65377171698271752, -20.05309729467257540 ) ) ;
#23757 = CARTESIAN_POINT ( 'NONE',  ( 20.82085833995528290, -1.902372073343062908, -15.34044165217533617 ) ) ;
#23758 = CARTESIAN_POINT ( 'NONE',  ( 20.30290135898079384, 0.5855005908018823257, -19.57000235946889433 ) ) ;
#23759 = VERTEX_POINT ( 'NONE', #10748 ) ;
#23760 = CARTESIAN_POINT ( 'NONE',  ( 29.03550452591436937, -6.934775515252377787, -18.27713033076000215 ) ) ;
#23761 = CIRCLE ( 'NONE', #10587, 8.000000000000005329 ) ;
#23762 = ORIENTED_EDGE ( 'NONE', *, *, #13651, .F. ) ;
#23763 = VERTEX_POINT ( 'NONE', #1302 ) ;
#23764 = FACE_OUTER_BOUND ( 'NONE', #10953, .T. ) ;
#23765 = EDGE_CURVE ( 'NONE', #6425, #29853, #2256, .T. ) ;
#23767 = ORIENTED_EDGE ( 'NONE', *, *, #21331, .T. ) ;
#23766 = CARTESIAN_POINT ( 'NONE',  ( 0.000000000000000000, 0.000000000000000000, -18.00000000000000000 ) ) ;
#23768 = VECTOR ( 'NONE', #5888, 1000.000000000000000 ) ;
#23769 = EDGE_CURVE ( 'NONE', #3794, #10636, #8302, .T. ) ;
#23770 = ADVANCED_FACE ( 'NONE', ( #10137 ), #12427, .T. ) ;
#23771 = CARTESIAN_POINT ( 'NONE',  ( 158.6922820468853104, -10.00000000000000000, 2.247092850131519715 ) ) ;
#23772 = EDGE_CURVE ( 'NONE', #17665, #29503, #18360, .T. ) ;
#23773 = DIRECTION ( 'NONE',  ( -2.698458740408365879E-16, 1.000000000000000000, 0.000000000000000000 ) ) ;
#23774 = CARTESIAN_POINT ( 'NONE',  ( 36.00107582698698394, -18.72480711723410352, -19.38214066600889751 ) ) ;
#23775 = VECTOR ( 'NONE', #14051, 1000.000000000000000 ) ;
#23776 = CARTESIAN_POINT ( 'NONE',  ( 9.644802874473198173, 17.65305953564175567, -17.69767226479352118 ) ) ;
#23777 = ORIENTED_EDGE ( 'NONE', *, *, #3074, .F. ) ;
#23778 = CARTESIAN_POINT ( 'NONE',  ( 136.1922820468854241, -10.00000000000000533, -30.91696583120935671 ) ) ;
#23779 = LINE ( 'NONE', #21472, #2245 ) ;
#23780 = CARTESIAN_POINT ( 'NONE',  ( 12.02871927673971619, 9.312984558958580905, -16.69105371450780595 ) ) ;
#23781 = DIRECTION ( 'NONE',  ( 0.000000000000000000, 0.000000000000000000, 1.000000000000000000 ) ) ;
#23782 = DIRECTION ( 'NONE',  ( -1.110223024625156540E-16, 0.000000000000000000, -1.000000000000000000 ) ) ;
#23783 = EDGE_LOOP ( 'NONE', ( #28956, #18506, #27495, #24150 ) ) ;
#23784 = FACE_OUTER_BOUND ( 'NONE', #21677, .T. ) ;
#23785 = VECTOR ( 'NONE', #22215, 1000.000000000000000 ) ;
#23786 = DIRECTION ( 'NONE',  ( 0.5877852522924731371, 1.586114251531760728E-16, 0.8090169943749474513 ) ) ;
#23787 = ORIENTED_EDGE ( 'NONE', *, *, #7058, .T. ) ;
#23788 = CARTESIAN_POINT ( 'NONE',  ( 153.6922820468853388, -10.00000000000000178, -0.6060766987539614181 ) ) ;
#23789 = VERTEX_POINT ( 'NONE', #29737 ) ;
#23790 = CARTESIAN_POINT ( 'NONE',  ( 13.37597118643279970, 7.624349635725309327, -15.71077405172158947 ) ) ;
#23791 = AXIS2_PLACEMENT_3D ( 'NONE', #28588, #7641, #7350 ) ;
#23792 = CARTESIAN_POINT ( 'NONE',  ( 22.79055345825320344, -4.301464833599455417, -14.90020420563294046 ) ) ;
#23793 = CARTESIAN_POINT ( 'NONE',  ( 19.79269262995316936, -1.159804626089355084, -18.29502107036499581 ) ) ;
#23794 = DIRECTION ( 'NONE',  ( -2.698458740408365879E-16, 1.000000000000000000, 0.000000000000000000 ) ) ;
#23795 = LINE ( 'NONE', #3195, #24797 ) ;
#23796 = DIRECTION ( 'NONE',  ( -2.698458740408366372E-16, 1.000000000000000000, 0.000000000000000000 ) ) ;
#23797 = VECTOR ( 'NONE', #20629, 999.9999999999998863 ) ;
#23798 = SHAPE_REPRESENTATION ( 'hex thin nut chamfered gradeab_iso_ISO - 4035 - M10 - N', ( #13190 ), #496 ) ;
#23799 = DIRECTION ( 'NONE',  ( -0.9510565162951536422, -2.566386769018988816E-16, -0.3090169943749472292 ) ) ;
#23800 = CYLINDRICAL_SURFACE ( 'NONE', #11323, 5.000000000000000888 ) ;
#23801 = FACE_OUTER_BOUND ( 'NONE', #22067, .T. ) ;
#23802 = EDGE_CURVE ( 'NONE', #6477, #17665, #16068, .T. ) ;
#23803 = ADVANCED_FACE ( 'NONE', ( #22655 ), #24799, .T. ) ;
#23804 = VECTOR ( 'NONE', #1780, 1000.000000000000000 ) ;
#23805 = CARTESIAN_POINT ( 'NONE',  ( -3.345653888883675542, 2.687187980154690514, -0.1391502195351382032 ) ) ;
#23806 = LINE ( 'NONE', #2905, #14307 ) ;
#23807 = EDGE_CURVE ( 'NONE', #10786, #23763, #4037, .T. ) ;
#23808 = EDGE_CURVE ( 'NONE', #11673, #19955, #797, .T. ) ;
#23809 = CARTESIAN_POINT ( 'NONE',  ( 10.47139596700049147, 16.45505391683073526, -17.33506929010674114 ) ) ;
#23810 = DIRECTION ( 'NONE',  ( 0.5877852522924731371, 0.000000000000000000, 0.8090169943749474513 ) ) ;
#23811 = CARTESIAN_POINT ( 'NONE',  ( 32.36240160181304759, -11.00785621467150044, -17.57054915585148436 ) ) ;
#23812 = VECTOR ( 'NONE', #18602, 1000.000000000000000 ) ;
#23813 = ORIENTED_EDGE ( 'NONE', *, *, #7201, .F. ) ;
#23814 = CARTESIAN_POINT ( 'NONE',  ( 8.944617638130560877, 16.95144162614991501, -17.89908301402565982 ) ) ;
#23815 = CARTESIAN_POINT ( 'NONE',  ( 18.04049687913209610, 0.8262538513465327306, -14.27019888128743297 ) ) ;
#23816 = CARTESIAN_POINT ( 'NONE',  ( 12.83625023806442655, 9.529724225483313660, -16.13881881377442795 ) ) ;
#23817 = FACE_BOUND ( 'NONE', #22237, .T. ) ;
#23818 = VECTOR ( 'NONE', #14902, 1000.000000000000000 ) ;
#23819 = ORIENTED_EDGE ( 'NONE', *, *, #21864, .F. ) ;
#23820 = CARTESIAN_POINT ( 'NONE',  ( 10.04637620539468124, 15.81139305134258599, -16.45082025127570091 ) ) ;
#23821 = CARTESIAN_POINT ( 'NONE',  ( 20.00000000000017053, 41.64101615137744972, 10.00000000000000178 ) ) ;
#23822 = CARTESIAN_POINT ( 'NONE',  ( 11.40798482813988635, 9.566882342703072695, -15.88774718835883348 ) ) ;
#23823 = CARTESIAN_POINT ( 'NONE',  ( 88.46122111574997859, -4.999999999999992895, 64.27083921987819792 ) ) ;
#23824 = ORIENTED_EDGE ( 'NONE', *, *, #6022, .F. ) ;
#23825 = ORIENTED_EDGE ( 'NONE', *, *, #10730, .T. ) ;
#23826 = CARTESIAN_POINT ( 'NONE',  ( 162.0152310637604671, -1.999999999999972689, -17.38167787843871182 ) ) ;
#23827 = ORIENTED_EDGE ( 'NONE', *, *, #8240, .F. ) ;
#23828 = CARTESIAN_POINT ( 'NONE',  ( 12.01190781424926435, 9.390070215761314287, -16.69800690218674788 ) ) ;
#23829 = ORIENTED_EDGE ( 'NONE', *, *, #24109, .T. ) ;
#23830 = CARTESIAN_POINT ( 'NONE',  ( 36.54859390953724585, -22.18451583373416014, -18.06010107863414405 ) ) ;
#23831 = CARTESIAN_POINT ( 'NONE',  ( 25.97851742199650005, -11.98992670343847244, -16.97112261376066655 ) ) ;
#23832 = CARTESIAN_POINT ( 'NONE',  ( 29.72799312938100513, -7.689056491358781997, -15.42978383025728384 ) ) ;
#23833 = ORIENTED_EDGE ( 'NONE', *, *, #28701, .F. ) ;
#23834 = CARTESIAN_POINT ( 'NONE',  ( 133.6922820468854241, -1.999999999999981348, -35.24709285013155835 ) ) ;
#23835 = CARTESIAN_POINT ( 'NONE',  ( 33.01527616964045109, -10.33189599206409959, -17.18388710919138873 ) ) ;
#23836 = APPLICATION_PROTOCOL_DEFINITION ( 'draft international standard', 'automotive_design', 1998, #28058 ) ;
#23837 = EDGE_CURVE ( 'NONE', #21323, #12653, #23104, .T. ) ;
#23838 = CARTESIAN_POINT ( 'NONE',  ( 19.97593658988278165, 3.663230212540239616, -18.70116431613266883 ) ) ;
#23839 = AXIS2_PLACEMENT_3D ( 'NONE', #11807, #17002, #383 ) ;
#23840 = CARTESIAN_POINT ( 'NONE',  ( 28.54819463643023880, -8.737303380947411213, -14.37855314081258307 ) ) ;
#23841 = STYLED_ITEM ( 'NONE', ( #151 ), #979 ) ;
#23842 = DIRECTION ( 'NONE',  ( 1.000000000000000000, 4.440892098500622217E-16, 0.000000000000000000 ) ) ;
#23843 = FACE_BOUND ( 'NONE', #7126, .T. ) ;
#23844 = AXIS2_PLACEMENT_3D ( 'NONE', #1326, #457, #19063 ) ;
#23845 = EDGE_CURVE ( 'NONE', #14013, #16928, #1913, .T. ) ;
#23846 = EDGE_CURVE ( 'NONE', #2926, #13701, #13476, .T. ) ;
#23847 = EDGE_CURVE ( 'NONE', #29946, #9369, #6478, .T. ) ;
#23848 = CARTESIAN_POINT ( 'NONE',  ( 131.1922820468854241, -1.999999999999981792, -10.74328820663507322 ) ) ;
#23849 = DIRECTION ( 'NONE',  ( -1.000000000000000000, -4.440892098500622217E-16, 0.000000000000000000 ) ) ;
#23850 = LINE ( 'NONE', #14209, #25814 ) ;
#23851 = CARTESIAN_POINT ( 'NONE',  ( 133.6922820468854241, -4.999999999999982236, -17.92658477444275533 ) ) ;
#23852 = PRODUCT_DEFINITION_CONTEXT ( 'detailed design', #17667, 'design' ) ;
#23853 = CARTESIAN_POINT ( 'NONE',  ( 12.24912255266251293, 9.517392596235749735, -15.33016477413064393 ) ) ;
#23854 = CARTESIAN_POINT ( 'NONE',  ( 147.0152310637605808, -10.00000000000000178, -26.04193191628311155 ) ) ;
#23855 = ORIENTED_EDGE ( 'NONE', *, *, #20817, .F. ) ;
#23856 = VECTOR ( 'NONE', #22140, 1000.000000000000000 ) ;
#23857 = DIRECTION ( 'NONE',  ( 0.9510565162951535312, 2.566386769018988816E-16, -0.3090169943749475623 ) ) ;
#23858 = VERTEX_POINT ( 'NONE', #15768 ) ;
#23859 = CARTESIAN_POINT ( 'NONE',  ( 11.47338783222600789, 9.266948822715743717, -15.86069975447064806 ) ) ;
#23860 = EDGE_LOOP ( 'NONE', ( #15894, #5071, #27413, #4733 ) ) ;
#23861 = CARTESIAN_POINT ( 'NONE',  ( 19.75347561433959953, 2.650395817966514578, -13.58229691592852184 ) ) ;
#23862 = CYLINDRICAL_SURFACE ( 'NONE', #18537, 129.8897274573438381 ) ;
#23863 = LINE ( 'NONE', #21557, #19342 ) ;
#23864 = DIRECTION ( 'NONE',  ( 0.5877852522924731371, 0.000000000000000000, 0.8090169943749474513 ) ) ;
#23865 = VECTOR ( 'NONE', #9396, 1000.000000000000000 ) ;
#23866 = CARTESIAN_POINT ( 'NONE',  ( 164.7287565553229456, -1.999999999999971356, -25.16025403784440329 ) ) ;
#23867 = CARTESIAN_POINT ( 'NONE',  ( 11.05544237569323762, 17.68929929418238700, -17.89823164173536441 ) ) ;
#23868 = ORIENTED_EDGE ( 'NONE', *, *, #10733, .T. ) ;
#23869 = CARTESIAN_POINT ( 'NONE',  ( 35.54859390953724585, -21.18451583373416014, -17.99055332684694974 ) ) ;
#23870 = CARTESIAN_POINT ( 'NONE',  ( 17.95327243003904982, 7.812726124483462264, -14.88485059575767266 ) ) ;
#23871 = ORIENTED_EDGE ( 'NONE', *, *, #8034, .F. ) ;
#23872 = PLANE ( 'NONE',  #5731 ) ;
#23873 = CARTESIAN_POINT ( 'NONE',  ( 9.111161770198492604, 16.18764900704733378, -17.05531488649033633 ) ) ;
#23874 = CARTESIAN_POINT ( 'NONE',  ( 30.37590262355644910, -7.260401249342992358, -13.74898149931492775 ) ) ;
#23875 = ORIENTED_EDGE ( 'NONE', *, *, #28282, .T. ) ;
#23876 = CARTESIAN_POINT ( 'NONE',  ( 2.500000000000000444, 0.000000000000000000, 0.000000000000000000 ) ) ;
#23877 = EDGE_CURVE ( 'NONE', #1409, #5536, #2060, .T. ) ;
#23878 =( NAMED_UNIT ( * ) PLANE_ANGLE_UNIT ( ) SI_UNIT ( $, .RADIAN. ) );
#23879 = EDGE_CURVE ( 'NONE', #600, #2712, #18515, .T. ) ;
#23880 = CARTESIAN_POINT ( 'NONE',  ( 21.19231167106929803, 0.1271100694386541607, -19.24388053421374778 ) ) ;
#23881 = CARTESIAN_POINT ( 'NONE',  ( 15.19333023161420648, 6.044621996704095501, -18.15278115226310263 ) ) ;
#23882 = ORIENTED_EDGE ( 'NONE', *, *, #15060, .F. ) ;
#23883 = CARTESIAN_POINT ( 'NONE',  ( 5.000000000000000000, 6.123233995736766282E-16, 23.00000000000000000 ) ) ;
#23884 = EDGE_LOOP ( 'NONE', ( #20870, #19875, #2799, #24745 ) ) ;
#23885 = ORIENTED_EDGE ( 'NONE', *, *, #8582, .T. ) ;
#23886 = LINE ( 'NONE', #11803, #23491 ) ;
#23887 = VECTOR ( 'NONE', #6402, 1000.000000000000000 ) ;
#23888 = ORIENTED_EDGE ( 'NONE', *, *, #20615, .F. ) ;
#23889 = EDGE_CURVE ( 'NONE', #6921, #28553, #4997, .T. ) ;
#23890 = DIRECTION ( 'NONE',  ( -0.8090169943749474513, -2.183098979609982436E-16, 0.5877852522924731371 ) ) ;
#23891 = VECTOR ( 'NONE', #24821, 1000.000000000000000 ) ;
#23892 = PLANE ( 'NONE',  #21736 ) ;
#23893 = DIRECTION ( 'NONE',  ( 1.000000000000000000, 2.698458740408365879E-16, -1.110223024625156540E-16 ) ) ;
#23894 = CARTESIAN_POINT ( 'NONE',  ( 169.5152310637604387, -4.999999999999971578, -1.881997125516404065E-14 ) ) ;
#23895 = CARTESIAN_POINT ( 'NONE',  ( 11.47395765415086188, 9.264374527449886543, -15.86046114005151075 ) ) ;
#23896 = CARTESIAN_POINT ( 'NONE',  ( 27.04128250769109698, -11.23896722199365961, -17.17396923023889244 ) ) ;
#23897 = CARTESIAN_POINT ( 'NONE',  ( 22.96196402503608169, -2.069733343145511828, -19.51364111617685992 ) ) ;
#23899 = ORIENTED_EDGE ( 'NONE', *, *, #6300, .T. ) ;
#23898 = CARTESIAN_POINT ( 'NONE',  ( 35.46335518829674527, -22.80158341140986167, -19.83799967047498924 ) ) ;
#23900 = LINE ( 'NONE', #26488, #7095 ) ;
#23901 = DIRECTION ( 'NONE',  ( 0.5877852522924731371, 1.586114251531760728E-16, 0.8090169943749474513 ) ) ;
#23902 = CARTESIAN_POINT ( 'NONE',  ( 12.50226005284522657, 8.571700941790735939, -15.12837371066060221 ) ) ;
#23903 = DIRECTION ( 'NONE',  ( -2.698458740408365879E-16, 1.000000000000000000, 0.000000000000000000 ) ) ;
#23904 = DIRECTION ( 'NONE',  ( 1.000000000000000000, 0.000000000000000000, 0.000000000000000000 ) ) ;
#23905 = CARTESIAN_POINT ( 'NONE',  ( 23.66272512268759343, 2.894330346666426745, -16.12005855839824520 ) ) ;
#23907 = ORIENTED_EDGE ( 'NONE', *, *, #18939, .T. ) ;
#23906 = PRODUCT_DEFINITION_FORMATION_WITH_SPECIFIED_SOURCE ( 'ANY', '', #1074, .NOT_KNOWN. ) ;
#23908 = DIRECTION ( 'NONE',  ( -2.698458740408365879E-16, 1.000000000000000000, 0.000000000000000000 ) ) ;
#23909 = CARTESIAN_POINT ( 'NONE',  ( 10.65690970294255280, 16.92416526288626955, -16.00322527524160066 ) ) ;
#23910 = VECTOR ( 'NONE', #10167, 1000.000000000000000 ) ;
#23911 = CARTESIAN_POINT ( 'NONE',  ( 175.7287565553229456, -9.999999999999994671, -2.233642730705309720 ) ) ;
#23912 = LINE ( 'NONE', #14715, #2536 ) ;
#23913 = CARTESIAN_POINT ( 'NONE',  ( 23.61827771231835982, -0.6465389018800060672, -13.57143891608981612 ) ) ;
#23914 = AXIS2_PLACEMENT_3D ( 'NONE', #18613, #25491, #6722 ) ;
#23915 = CARTESIAN_POINT ( 'NONE',  ( 17.99586569009407455, 10.99629947005995767, -19.18704736271931210 ) ) ;
#23916 = ORIENTED_EDGE ( 'NONE', *, *, #24026, .T. ) ;
#23917 = CARTESIAN_POINT ( 'NONE',  ( 33.44337896868773186, -12.72690026786775341, -19.72159258799634074 ) ) ;
#23918 = EDGE_CURVE ( 'NONE', #2712, #14597, #3889, .T. ) ;
#23919 = CARTESIAN_POINT ( 'NONE',  ( 21.64008331710702038, -0.7226702609205537531, -18.85644019536628946 ) ) ;
#23920 = ADVANCED_FACE ( 'NONE', ( #1611 ), #27567, .T. ) ;
#23921 = CARTESIAN_POINT ( 'NONE',  ( 16.81761937449845234, 3.371063479271922514, -17.17107737352595720 ) ) ;
#23922 = VERTEX_POINT ( 'NONE', #13628 ) ;
#23923 = CARTESIAN_POINT ( 'NONE',  ( 26.92475197568164802, -10.17130474311345800, -13.43658410890694732 ) ) ;
#23924 = VECTOR ( 'NONE', #26802, 1000.000000000000000 ) ;
#23925 = VECTOR ( 'NONE', #4927, 1000.000000000000000 ) ;
#23926 = ORIENTED_EDGE ( 'NONE', *, *, #19314, .F. ) ;
#23927 = DIRECTION ( 'NONE',  ( 0.5877852522924731371, 1.586114251531760728E-16, -0.8090169943749474513 ) ) ;
#23928 = CIRCLE ( 'NONE', #27851, 4.188000000000025480 ) ;
#23930 = ORIENTED_EDGE ( 'NONE', *, *, #24279, .T. ) ;
#23929 = DIRECTION ( 'NONE',  ( 0.5877852522924731371, 1.586114251531760728E-16, -0.8090169943749474513 ) ) ;
#23931 = LINE ( 'NONE', #19027, #20673 ) ;
#23932 = PLANE ( 'NONE',  #14611 ) ;
#23933 = CARTESIAN_POINT ( 'NONE',  ( 36.09161981528372110, -20.13157329416283048, -20.44814669990763889 ) ) ;
#23934 = CARTESIAN_POINT ( 'NONE',  ( 12.89209817343266984, 7.685947621549766851, -14.81766584744191739 ) ) ;
#23935 =( REPRESENTATION_RELATIONSHIP ('NONE','NONE', #5250, #23798 ) REPRESENTATION_RELATIONSHIP_WITH_TRANSFORMATION ( #13118 )SHAPE_REPRESENTATION_RELATIONSHIP( ) );
#23936 = CARTESIAN_POINT ( 'NONE',  ( -19.99999999999998934, 55.00000000000000711, 24.99999999999998934 ) ) ;
#23937 = DIRECTION ( 'NONE',  ( -2.698458740408365879E-16, 1.000000000000000000, 0.000000000000000000 ) ) ;
#23938 = CARTESIAN_POINT ( 'NONE',  ( 12.22285885739602662, 8.868278133530205665, -16.57678160000113721 ) ) ;
#23939 = CARTESIAN_POINT ( 'NONE',  ( 8.000000000000001776, 4.336808689942017736E-15, -5.000000000000000888 ) ) ;
#23940 = PLANE ( 'NONE',  #26611 ) ;
#23941 = CONICAL_SURFACE ( 'NONE', #4902, 8.000000000000007105, 1.047197551196596077 ) ;
#23942 = EDGE_LOOP ( 'NONE', ( #12938, #17527, #17542, #27014 ) ) ;
#23943 = EDGE_LOOP ( 'NONE', ( #23111, #12465, #3682, #24440, #1541 ) ) ;
#23944 = AXIS2_PLACEMENT_3D ( 'NONE', #27003, #23510, #24535 ) ;
#23945 = CARTESIAN_POINT ( 'NONE',  ( 137.0152310637606092, -4.999999999999980460, -24.27857615940569147 ) ) ;
#23946 = CARTESIAN_POINT ( 'NONE',  ( 10.91913706431875930, -5.000000000000015099, 33.60564838301395696 ) ) ;
#23947 = ORIENTED_EDGE ( 'NONE', *, *, #26436, .T. ) ;
#23948 = ORIENTED_EDGE ( 'NONE', *, *, #17818, .T. ) ;
#23949 = ORIENTED_EDGE ( 'NONE', *, *, #10478, .F. ) ;
#23950 = CARTESIAN_POINT ( 'NONE',  ( 11.22589550380084411, 9.082134330754477958, -17.24077175062176082 ) ) ;
#23951 = ORIENTED_EDGE ( 'NONE', *, *, #5331, .T. ) ;
#23952 = EDGE_CURVE ( 'NONE', #17919, #1754, #11045, .T. ) ;
#23953 = CARTESIAN_POINT ( 'NONE',  ( 24.97936687747968776, -7.804033356035183999, -18.74018705570338028 ) ) ;
#23954 = EDGE_CURVE ( 'NONE', #17680, #4823, #20198, .T. ) ;
#23955 = CARTESIAN_POINT ( 'NONE',  ( 22.68884594494833706, -6.762261587817247843, -18.56982216542981234 ) ) ;
#23956 = FACE_OUTER_BOUND ( 'NONE', #29757, .T. ) ;
#23957 = LINE ( 'NONE', #3491, #2386 ) ;
#23958 = EDGE_CURVE ( 'NONE', #27211, #13095, #4332, .T. ) ;
#23959 = LINE ( 'NONE', #16765, #19096 ) ;
#23960 = VERTEX_POINT ( 'NONE', #15623 ) ;
#23961 = CARTESIAN_POINT ( 'NONE',  ( 20.00000000000000355, 60.00000000000000711, -30.00000000000000000 ) ) ;
#23962 = DIRECTION ( 'NONE',  ( -0.5877852522924731371, -1.586114251531760728E-16, -0.8090169943749474513 ) ) ;
#23963 = LINE ( 'NONE', #12029, #14070 ) ;
#23964 = VECTOR ( 'NONE', #7423, 1000.000000000000000 ) ;
#23965 = CARTESIAN_POINT ( 'NONE',  ( 0.000000000000000000, 0.000000000000000000, -5.000000000000000888 ) ) ;
#23966 = CARTESIAN_POINT ( 'NONE',  ( 172.2287565553229172, -4.999999999999971578, -12.16987298107781434 ) ) ;
#23967 = CARTESIAN_POINT ( 'NONE',  ( 12.02835731808789355, 9.314632867394664117, -16.69120428796748357 ) ) ;
#23968 = DIRECTION ( 'NONE',  ( -0.5877852522924731371, -1.586114251531760728E-16, -0.8090169943749474513 ) ) ;
#23969 = CARTESIAN_POINT ( 'NONE',  ( 32.96569147872224903, -11.36116021242123608, -19.12347989294568151 ) ) ;
#23970 = ORIENTED_EDGE ( 'NONE', *, *, #9718, .T. ) ;
#23971 = CARTESIAN_POINT ( 'NONE',  ( 13.37268442792299261, 7.622911828202562745, -15.71339253741762221 ) ) ;
#23972 = DIRECTION ( 'NONE',  ( -2.698458740408365879E-16, 1.000000000000000000, 0.000000000000000000 ) ) ;
#23973 = CARTESIAN_POINT ( 'NONE',  ( 24.14317479683219858, -6.286850201977149055, -18.60698471650063723 ) ) ;
#23974 = CARTESIAN_POINT ( 'NONE',  ( 12.82717298413408358, 9.563916880749394167, -16.14313977175105919 ) ) ;
#23975 = DIRECTION ( 'NONE',  ( 0.000000000000000000, 0.000000000000000000, 1.000000000000000000 ) ) ;
#23976 = EDGE_LOOP ( 'NONE', ( #3514, #17588, #29102, #24893, #17123 ) ) ;
#23977 = ORIENTED_EDGE ( 'NONE', *, *, #17817, .T. ) ;
#23978 = CARTESIAN_POINT ( 'NONE',  ( 11.47652547240386944, 9.253065934422213701, -15.85936358228339316 ) ) ;
#23979 = FACE_OUTER_BOUND ( 'NONE', #15674, .T. ) ;
#23980 = CARTESIAN_POINT ( 'NONE',  ( 9.917712295358372288, 16.40146214360271770, -16.50402730409559027 ) ) ;
#23981 = LINE ( 'NONE', #28733, #7207 ) ;
#23982 = ORIENTED_EDGE ( 'NONE', *, *, #897, .F. ) ;
#23983 = CARTESIAN_POINT ( 'NONE',  ( 4.000000000000019540, 6.928203230275512325, 0.000000000000000000 ) ) ;
#23984 = ORIENTED_EDGE ( 'NONE', *, *, #25110, .T. ) ;
#23985 = CARTESIAN_POINT ( 'NONE',  ( 12.02823749386838514, 9.315180647891255106, -16.69125397286443047 ) ) ;
#23986 = VERTEX_POINT ( 'NONE', #24956 ) ;
#23987 = CARTESIAN_POINT ( 'NONE',  ( 36.45689639539443050, -22.77256747621617095, -19.95163700058902734 ) ) ;
#23988 = CARTESIAN_POINT ( 'NONE',  ( 15.23264752967198099, 8.612683518626374379, -20.21708921969009154 ) ) ;
#23989 = CARTESIAN_POINT ( 'NONE',  ( 16.60417661732421735, 9.954854064686266213, -19.72231676211552909 ) ) ;
#23990 = ORIENTED_EDGE ( 'NONE', *, *, #12976, .T. ) ;
#23991 = EDGE_CURVE ( 'NONE', #18805, #11448, #364, .T. ) ;
#23992 = CARTESIAN_POINT ( 'NONE',  ( 0.000000000000000000, 0.000000000000000000, 0.000000000000000000 ) ) ;
#23993 = EDGE_CURVE ( 'NONE', #26875, #2818, #60, .T. ) ;
#23994 = ADVANCED_FACE ( 'NONE', ( #9344 ), #2655, .T. ) ;
#23995 = ADVANCED_FACE ( 'NONE', ( #12243 ), #18671, .T. ) ;
#23996 = CARTESIAN_POINT ( 'NONE',  ( 20.00000000000017053, 41.64101615137744972, 14.00000000000000178 ) ) ;
#23997 = CONTEXT_DEPENDENT_SHAPE_REPRESENTATION ( #931, #17370 ) ;
#23998 = CARTESIAN_POINT ( 'NONE',  ( 16.84916689134472989, 3.454690908320265041, -17.64892000621457413 ) ) ;
#23999 = CARTESIAN_POINT ( 'NONE',  ( 18.88762249820254624, 5.002188274287570735, -13.90571046850145542 ) ) ;
#24000 = DIRECTION ( 'NONE',  ( 0.9510565162951535312, 2.566386769018988816E-16, -0.3090169943749475623 ) ) ;
#24001 = FACE_BOUND ( 'NONE', #22423, .T. ) ;
#24002 = VECTOR ( 'NONE', #22625, 999.9999999999998863 ) ;
#24003 = DIRECTION ( 'NONE',  ( 0.5877852522924731371, 1.586114251531760728E-16, 0.8090169943749474513 ) ) ;
#24004 = CARTESIAN_POINT ( 'NONE',  ( 171.1922820468853104, -1.999999999999970912, -13.59645775552055902 ) ) ;
#24005 = CARTESIAN_POINT ( 'NONE',  ( 8.000000000000000000, 9.797174393178825657E-16, 18.00000000000000000 ) ) ;
#24006 = PLANE ( 'NONE',  #24636 ) ;
#24007 = CARTESIAN_POINT ( 'NONE',  ( 12.27491818236995691, 9.503772128122387031, -15.31151344616081822 ) ) ;
#24008 = PLANE ( 'NONE',  #21165 ) ;
#24009 = CARTESIAN_POINT ( 'NONE',  ( 151.1922820468854525, -1.999999999999975353, -30.91696583120936026 ) ) ;
#24010 = ORIENTED_EDGE ( 'NONE', *, *, #409, .T. ) ;
#24011 = CARTESIAN_POINT ( 'NONE',  ( 12.07641845611955489, 8.540206757827041528, -15.45582622123028216 ) ) ;
#24012 = EDGE_LOOP ( 'NONE', ( #19651, #23599, #6587, #5440, #12463, #23096 ) ) ;
#24013 = AXIS2_PLACEMENT_3D ( 'NONE', #9888, #4716, #23489 ) ;
#24014 = CARTESIAN_POINT ( 'NONE',  ( 20.52698940127687877, 5.222567878441341627, -18.38034891569893503 ) ) ;
#24015 = FACE_OUTER_BOUND ( 'NONE', #7279, .T. ) ;
#24016 = DIRECTION ( 'NONE',  ( -1.000000000000000000, -2.891205793294689173E-16, 0.000000000000000000 ) ) ;
#24017 = CARTESIAN_POINT ( 'NONE',  ( 161.1922820468853104, -1.999999999999973577, -2.083034168790677043 ) ) ;
#24018 = CARTESIAN_POINT ( 'NONE',  ( 12.82970573826865390, 9.552301347437191836, -16.14209238882153130 ) ) ;
#24019 = ORIENTED_EDGE ( 'NONE', *, *, #8951, .F. ) ;
#24020 = CARTESIAN_POINT ( 'NONE',  ( 35.15837367389831769, -19.43146302041509443, -19.19767279675701488 ) ) ;
#24021 = CARTESIAN_POINT ( 'NONE',  ( 20.99533150354982070, 4.487273811465053441, -19.54336078777620500 ) ) ;
#24022 = ADVANCED_FACE ( 'NONE', ( #28614 ), #2364, .T. ) ;
#24023 = DIRECTION ( 'NONE',  ( 1.000000000000000000, 0.000000000000000000, 0.000000000000000000 ) ) ;
#24024 = VECTOR ( 'NONE', #16840, 1000.000000000000000 ) ;
#24025 = CARTESIAN_POINT ( 'NONE',  ( 17.46151185945609186, 6.859213057953727599, -13.86392132274949418 ) ) ;
#24026 = EDGE_CURVE ( 'NONE', #20158, #12496, #16223, .T. ) ;
#24027 = ORIENTED_EDGE ( 'NONE', *, *, #951, .F. ) ;
#24028 = ADVANCED_FACE ( 'NONE', ( #212 ), #14369, .T. ) ;
#24029 = CARTESIAN_POINT ( 'NONE',  ( -8.000000000000001776, -4.336808689942017736E-15, -5.000000000000000888 ) ) ;
#24030 = CARTESIAN_POINT ( 'NONE',  ( 21.56383972367567736, -3.323709001909281202, -18.92284382192250192 ) ) ;
#24031 = CARTESIAN_POINT ( 'NONE',  ( 16.25879716139461095, 4.256374150336979412, -17.55500201710977137 ) ) ;
#24032 = CARTESIAN_POINT ( 'NONE',  ( 5.200000000000002842, 3.061616997868384127E-16, -2.500000000000000888 ) ) ;
#24033 = ORIENTED_EDGE ( 'NONE', *, *, #13930, .F. ) ;
#24034 = FACE_OUTER_BOUND ( 'NONE', #27275, .T. ) ;
#24035 = DIRECTION ( 'NONE',  ( 0.9510565162951536422, 0.000000000000000000, -0.3090169943749475623 ) ) ;
#24036 = LINE ( 'NONE', #10120, #28640 ) ;
#24037 = LINE ( 'NONE', #3137, #431 ) ;
#24038 = DIRECTION ( 'NONE',  ( 0.000000000000000000, 2.775557561562890735E-17, -1.000000000000000000 ) ) ;
#24039 = AXIS2_PLACEMENT_3D ( 'NONE', #29939, #30083, #266 ) ;
#24040 = CARTESIAN_POINT ( 'NONE',  ( 9.981537699549546616, 16.10875070413535681, -16.47763325427154868 ) ) ;
#24041 = CARTESIAN_POINT ( 'NONE',  ( 28.32023557703361405, -7.180604414193060059, -17.61256657898508138 ) ) ;
#24042 = CARTESIAN_POINT ( 'NONE',  ( 26.42570577731286718, -9.588051360687080305, -12.79080846482418643 ) ) ;
#24043 = EDGE_CURVE ( 'NONE', #10839, #28371, #20949, .T. ) ;
#24045 = VERTEX_POINT ( 'NONE', #9490 ) ;
#24044 = CARTESIAN_POINT ( 'NONE',  ( 32.12153525177792091, -10.97127362787143312, -16.88978156643115724 ) ) ;
#24046 = DIRECTION ( 'NONE',  ( -0.000000000000000000, -0.000000000000000000, -1.000000000000000000 ) ) ;
#24047 = CARTESIAN_POINT ( 'NONE',  ( 164.5152310637604387, -1.999999999999972689, -4.391296821672111328 ) ) ;
#24048 = FACE_OUTER_BOUND ( 'NONE', #2996, .T. ) ;
#24049 = CARTESIAN_POINT ( 'NONE',  ( -1.318516776095826071, -3.857556137907095284, -1.931970283426452982E-14 ) ) ;
#24050 = DIRECTION ( 'NONE',  ( -0.8090169943749474513, -2.183098979609982436E-16, -0.5877852522924731371 ) ) ;
#24051 = LINE ( 'NONE', #9837, #766 ) ;
#24052 = CARTESIAN_POINT ( 'NONE',  ( 21.64656857049893901, 5.639188926465734220, -17.17864421186117951 ) ) ;
#24053 = ORIENTED_EDGE ( 'NONE', *, *, #23668, .F. ) ;
#24054 = DIRECTION ( 'NONE',  ( 0.3090169943749475623, 8.338696094058001131E-17, 0.9510565162951536422 ) ) ;
#24055 = CARTESIAN_POINT ( 'NONE',  ( 12.26606010314042017, 9.512972848517913249, -15.31757320754432605 ) ) ;
#24056 = PLANE ( 'NONE',  #8095 ) ;
#24057 = FACE_OUTER_BOUND ( 'NONE', #16058, .T. ) ;
#24058 = CARTESIAN_POINT ( 'NONE',  ( 18.04049687913209610, 0.8262538513465327306, -14.27019888128743297 ) ) ;
#24059 = CARTESIAN_POINT ( 'NONE',  ( 22.63682584648026008, 4.680144189823682410, -16.86151017930854223 ) ) ;
#24060 = VERTEX_POINT ( 'NONE', #5230 ) ;
#24061 = EDGE_CURVE ( 'NONE', #14415, #25233, #18814, .T. ) ;
#24062 = CARTESIAN_POINT ( 'NONE',  ( 35.52583876341286384, -22.08228901593173177, -18.97221062538168113 ) ) ;
#24063 = CARTESIAN_POINT ( 'NONE',  ( 24.27832910178602788, -5.559203070376852018, -13.12236226054620047 ) ) ;
#24064 = CARTESIAN_POINT ( 'NONE',  ( 20.25556019283287768, 3.967930604842117681, -18.44304694949289569 ) ) ;
#24065 = VECTOR ( 'NONE', #2986, 1000.000000000000000 ) ;
#24066 = ORIENTED_EDGE ( 'NONE', *, *, #27482, .T. ) ;
#24067 = CARTESIAN_POINT ( 'NONE',  ( 176.1922820468853104, -1.999999999999968914, -19.40354224447947828 ) ) ;
#24068 = ORIENTED_EDGE ( 'NONE', *, *, #2644, .F. ) ;
#24069 = PLANE ( 'NONE',  #963 ) ;
#24070 = FACE_OUTER_BOUND ( 'NONE', #2409, .T. ) ;
#24071 = CARTESIAN_POINT ( 'NONE',  ( 146.1922820468853956, -1.999999999999978018, -2.083034168790677043 ) ) ;
#24072 = CARTESIAN_POINT ( 'NONE',  ( 173.6922820468852819, -9.999999999999996447, -9.266330736598359152 ) ) ;
#24073 = ADVANCED_FACE ( 'NONE', ( #28172 ), #2965, .T. ) ;
#24074 = CARTESIAN_POINT ( 'NONE',  ( 36.44920892064849482, -21.73803172434679354, -19.68085951391205057 ) ) ;
#24075 = CARTESIAN_POINT ( 'NONE',  ( 9.910898653440767703, 16.43271037397421708, -16.50709950392603531 ) ) ;
#24076 = EDGE_CURVE ( 'NONE', #18221, #506, #21253, .T. ) ;
#24077 = VECTOR ( 'NONE', #25910, 1000.000000000000000 ) ;
#24078 = FACE_OUTER_BOUND ( 'NONE', #1795, .T. ) ;
#24079 = LINE ( 'NONE', #7586, #14868 ) ;
#24080 = CARTESIAN_POINT ( 'NONE',  ( 12.02908293258818517, 9.311337566433326884, -16.69090174519279657 ) ) ;
#24081 = CARTESIAN_POINT ( 'NONE',  ( 137.0152310637606092, -4.999999999999980460, -15.61832212156129351 ) ) ;
#24082 = DIRECTION ( 'NONE',  ( -0.9510565162951536422, -2.566386769018988816E-16, -0.3090169943749472292 ) ) ;
#24083 = VERTEX_POINT ( 'NONE', #13921 ) ;
#24084 = CARTESIAN_POINT ( 'NONE',  ( -4.000000000000010658, -2.309401076758525573, -2.450000000000000178 ) ) ;
#24085 = FACE_OUTER_BOUND ( 'NONE', #6546, .T. ) ;
#24086 = ORIENTED_EDGE ( 'NONE', *, *, #28151, .F. ) ;
#24087 = DIRECTION ( 'NONE',  ( -0.7071067811865306973, 8.659560562355138702E-17, -0.7071067811865643371 ) ) ;
#24088 = ORIENTED_EDGE ( 'NONE', *, *, #19270, .F. ) ;
#24089 = ORIENTED_EDGE ( 'NONE', *, *, #17484, .F. ) ;
#24090 = CARTESIAN_POINT ( 'NONE',  ( 11.22336320048417591, 9.093679674329528950, -17.24182414271593800 ) ) ;
#24091 = CARTESIAN_POINT ( 'NONE',  ( 25.18430082464795916, -12.47910854170484818, -17.34997305645471855 ) ) ;
#24092 = CARTESIAN_POINT ( 'NONE',  ( 23.76385019584477831, -1.264968635605209446, -19.12809044524397351 ) ) ;
#24093 = CARTESIAN_POINT ( 'NONE',  ( 149.7287565553230309, -1.999999999999975353, -25.16025403784440329 ) ) ;
#24094 = CARTESIAN_POINT ( 'NONE',  ( 63.44486372867152824, -29.99999999999998934, -17.99999999999998934 ) ) ;
#24095 = DIRECTION ( 'NONE',  ( -0.8090169943749474513, -2.183098979609982436E-16, 0.5877852522924731371 ) ) ;
#24096 = VECTOR ( 'NONE', #20080, 1000.000000000000000 ) ;
#24097 = DIRECTION ( 'NONE',  ( 0.5877852522924731371, 0.000000000000000000, 0.8090169943749474513 ) ) ;
#24098 = CARTESIAN_POINT ( 'NONE',  ( 142.0152310637606092, -1.999999999999978018, -24.27857615940569147 ) ) ;
#24099 = CARTESIAN_POINT ( 'NONE',  ( 130.7287565553229456, -4.999999999999983125, 3.500000000000003109 ) ) ;
#24100 = CARTESIAN_POINT ( 'NONE',  ( 134.5152310637605808, -10.00000000000000533, -2.627941064794695691 ) ) ;
#24101 = CARTESIAN_POINT ( 'NONE',  ( 177.2287565553229172, -9.999999999999994671, -29.49038105676660493 ) ) ;
#24102 = VECTOR ( 'NONE', #23693, 1000.000000000000000 ) ;
#24103 = CARTESIAN_POINT ( 'NONE',  ( 11.76876341733043141, 10.50516141373230106, -16.79855566342228101 ) ) ;
#24104 = EDGE_CURVE ( 'NONE', #29971, #20355, #513, .T. ) ;
#24105 = EDGE_CURVE ( 'NONE', #18619, #16899, #9650, .T. ) ;
#24106 = CARTESIAN_POINT ( 'NONE',  ( 35.54859390953724585, -22.18451583373416014, -18.06010107863414405 ) ) ;
#24107 = ORIENTED_EDGE ( 'NONE', *, *, #28212, .T. ) ;
#24108 = CARTESIAN_POINT ( 'NONE',  ( 8.944584683310379702, 16.95159276115599667, -17.92454625180715411 ) ) ;
#24109 = EDGE_CURVE ( 'NONE', #19416, #14794, #9945, .T. ) ;
#24110 = ADVANCED_FACE ( 'NONE', ( #26002 ), #6186, .T. ) ;
#24111 = CARTESIAN_POINT ( 'NONE',  ( 23.22413189157496305, -7.367447486509826504, -15.63851824576001981 ) ) ;
#24112 = CARTESIAN_POINT ( 'NONE',  ( 12.83220575256047802, 9.540835953717470730, -16.14105854569320542 ) ) ;
#24113 = FACE_BOUND ( 'NONE', #19970, .T. ) ;
#24114 = ORIENTED_EDGE ( 'NONE', *, *, #18036, .F. ) ;
#24115 = EDGE_LOOP ( 'NONE', ( #22529, #7208, #3237 ) ) ;
#24116 = CARTESIAN_POINT ( 'NONE',  ( 11.48890098693651396, 9.204103201752445784, -15.85365151319587440 ) ) ;
#24117 = DIRECTION ( 'NONE',  ( 1.000000000000000000, 2.698458740408365879E-16, -1.110223024625156540E-16 ) ) ;
#24118 = VECTOR ( 'NONE', #28499, 1000.000000000000000 ) ;
#24119 = CARTESIAN_POINT ( 'NONE',  ( 11.48890098693651396, 9.204103201752445784, -15.85365151319587440 ) ) ;
#24120 = LINE ( 'NONE', #24419, #27216 ) ;
#24121 = ORIENTED_EDGE ( 'NONE', *, *, #15206, .T. ) ;
#24122 = LINE ( 'NONE', #763, #30138 ) ;
#24123 = ORIENTED_EDGE ( 'NONE', *, *, #12216, .T. ) ;
#24124 = CARTESIAN_POINT ( 'NONE',  ( 12.02761088988360783, 9.318053909225662679, -16.69151312802368636 ) ) ;
#24125 = ORIENTED_EDGE ( 'NONE', *, *, #13892, .T. ) ;
#24126 = CARTESIAN_POINT ( 'NONE',  ( 36.54859390953724585, -23.18451583373416014, -18.06010107863414405 ) ) ;
#24127 = CARTESIAN_POINT ( 'NONE',  ( 29.88803641097454999, -7.968445601786871002, -16.75847372370488131 ) ) ;
#24128 = CARTESIAN_POINT ( 'NONE',  ( 13.51959648670337444, 7.024181567627514333, -18.72314150793285492 ) ) ;
#24129 = CARTESIAN_POINT ( 'NONE',  ( 132.0152310637605524, -10.00000000000000711, -34.70218595412750773 ) ) ;
#24130 = VERTEX_POINT ( 'NONE', #4781 ) ;
#24131 = VERTEX_POINT ( 'NONE', #14072 ) ;
#24132 = DIRECTION ( 'NONE',  ( 2.207829878515935943E-16, 1.000000000000000000, 0.000000000000000000 ) ) ;
#24133 = APPLICATION_PROTOCOL_DEFINITION ( 'draft international standard', 'automotive_design', 1998, #6759 ) ;
#24134 = CARTESIAN_POINT ( 'NONE',  ( 20.55682936838109498, 0.8107970201405315658, -19.60370085144657182 ) ) ;
#24135 = CARTESIAN_POINT ( 'NONE',  ( 15.93484470893836935, 6.939319753835953009, -14.67888072223970752 ) ) ;
#24136 = LINE ( 'NONE', #28758, #21247 ) ;
#24137 = FACE_BOUND ( 'NONE', #26815, .T. ) ;
#24138 = VECTOR ( 'NONE', #18955, 1000.000000000000000 ) ;
#24139 = DIRECTION ( 'NONE',  ( 0.5877852522924731371, 0.000000000000000000, 0.8090169943749474513 ) ) ;
#24140 = DIRECTION ( 'NONE',  ( -2.698458740408365879E-16, 1.000000000000000000, 0.000000000000000000 ) ) ;
#24141 = CARTESIAN_POINT ( 'NONE',  ( -4.000000000000010658, -2.309401076758525573, -2.450000000000000178 ) ) ;
#24142 = EDGE_CURVE ( 'NONE', #14128, #22275, #23401, .T. ) ;
#24143 = LINE ( 'NONE', #9932, #26585 ) ;
#24144 = EDGE_CURVE ( 'NONE', #28630, #23789, #28137, .T. ) ;
#24145 = CARTESIAN_POINT ( 'NONE',  ( 12.27670864112623583, 9.495496515443743846, -15.31077793565516565 ) ) ;
#24146 = DIRECTION ( 'NONE',  ( -0.9510565162951536422, 0.000000000000000000, -0.3090169943749472292 ) ) ;
#24147 = ORIENTED_EDGE ( 'NONE', *, *, #913, .F. ) ;
#24148 = SHAPE_REPRESENTATION ( 'base plate', ( #13190 ), #3942 ) ;
#24149 = DIRECTION ( 'NONE',  ( -0.9510565162951536422, 0.000000000000000000, -0.3090169943749472292 ) ) ;
#24150 = ORIENTED_EDGE ( 'NONE', *, *, #13557, .F. ) ;
#24151 = CARTESIAN_POINT ( 'NONE',  ( 11.49350937636955372, 9.187954247928445284, -15.85136552863131421 ) ) ;
#24152 = EDGE_LOOP ( 'NONE', ( #6811, #11843 ) ) ;
#24153 = CARTESIAN_POINT ( 'NONE',  ( 17.21229802721762780, 1.518872817929493912, -15.34595729721386448 ) ) ;
#24154 = DIRECTION ( 'NONE',  ( 1.000000000000000000, 2.698458740408365879E-16, -1.110223024625156540E-16 ) ) ;
#24155 = DIRECTION ( 'NONE',  ( -0.8090169943749474513, -2.183098979609982436E-16, 0.5877852522924731371 ) ) ;
#24156 = ORIENTED_EDGE ( 'NONE', *, *, #5259, .T. ) ;
#24157 = DIRECTION ( 'NONE',  ( 2.908569913943825061E-16, -1.000000000000000000, -6.826925868028081731E-18 ) ) ;
#24158 = VERTEX_POINT ( 'NONE', #10095 ) ;
#24159 = CARTESIAN_POINT ( 'NONE',  ( 12.84980237226573863, 9.516412629723424388, -16.12948954962132575 ) ) ;
#24160 = CARTESIAN_POINT ( 'NONE',  ( 35.71575670127456448, -17.44301942315582110, -19.29589553906783905 ) ) ;
#24161 = CARTESIAN_POINT ( 'NONE',  ( 15.41431293496917121, 3.575304669039410133, -17.09800041271234150 ) ) ;
#24162 = ORIENTED_EDGE ( 'NONE', *, *, #25412, .T. ) ;
#24163 = EDGE_LOOP ( 'NONE', ( #8963, #7088, #7067, #5961, #13475 ) ) ;
#24164 = VERTEX_POINT ( 'NONE', #12997 ) ;
#24165 = CIRCLE ( 'NONE', #11472, 3.000000000000002665 ) ;
#24166 = DIRECTION ( 'NONE',  ( -0.8090169943749474513, -2.183098979609982436E-16, 0.5877852522924731371 ) ) ;
#24167 = CARTESIAN_POINT ( 'NONE',  ( 14.59671049609067950, 6.266606045730605423, -20.00302036566705155 ) ) ;
#24168 = ORIENTED_EDGE ( 'NONE', *, *, #5777, .F. ) ;
#24169 = CARTESIAN_POINT ( 'NONE',  ( 164.5152310637604671, -9.999999999999998224, -21.71180489736091346 ) ) ;
#24170 = CARTESIAN_POINT ( 'NONE',  ( 20.75491211191951635, -1.144232541536293946, -14.27023797479654554 ) ) ;
#24171 = CARTESIAN_POINT ( 'NONE',  ( 20.59810038911313157, 5.339108984243529754, -18.13170489685289510 ) ) ;
#24172 = ORIENTED_EDGE ( 'NONE', *, *, #27170, .F. ) ;
#24173 = ORIENTED_EDGE ( 'NONE', *, *, #8690, .F. ) ;
#24174 = DIRECTION ( 'NONE',  ( -0.5877852522924731371, 0.000000000000000000, 0.8090169943749474513 ) ) ;
#24175 = VECTOR ( 'NONE', #11710, 1000.000000000000000 ) ;
#24176 = DIRECTION ( 'NONE',  ( 0.3090169943749475623, 8.338696094058001131E-17, 0.9510565162951536422 ) ) ;
#24177 = CARTESIAN_POINT ( 'NONE',  ( -4.681481898397004571, 6.534749472788154101, -5.000000000000000000 ) ) ;
#24178 = CARTESIAN_POINT ( 'NONE',  ( 161.1922820468853956, -4.999999999999974243, -30.91696583120936026 ) ) ;
#24179 = AXIS2_PLACEMENT_3D ( 'NONE', #6622, #20796, #18209 ) ;
#24180 = EDGE_CURVE ( 'NONE', #25256, #20403, #23215, .T. ) ;
#24181 = EDGE_CURVE ( 'NONE', #2025, #7643, #805, .T. ) ;
#24182 = LINE ( 'NONE', #21878, #24118 ) ;
#24183 = CIRCLE ( 'NONE', #25161, 13.00000000000000178 ) ;
#24184 = EDGE_CURVE ( 'NONE', #21114, #29571, #8260, .T. ) ;
#24185 = CARTESIAN_POINT ( 'NONE',  ( 11.77869587587188249, 8.711114196793760200, -15.67004689359726299 ) ) ;
#24186 = EDGE_CURVE ( 'NONE', #28478, #10393, #19409, .T. ) ;
#24187 = CARTESIAN_POINT ( 'NONE',  ( 25.90061519764796572, -9.523157571424881951, -17.57609359838447816 ) ) ;
#24188 = CARTESIAN_POINT ( 'NONE',  ( 25.05301747714807448, -9.477991407908255894, -18.78921932654604632 ) ) ;
#24190 = ORIENTED_EDGE ( 'NONE', *, *, #19821, .F. ) ;
#24189 = CARTESIAN_POINT ( 'NONE',  ( 32.52799721746220740, -11.03300674309804386, -18.03857687357939099 ) ) ;
#24191 = PLANE ( 'NONE',  #20762 ) ;
#24192 = CARTESIAN_POINT ( 'NONE',  ( 147.2287565553230309, -10.00000000000000178, -29.49038105676660138 ) ) ;
#24193 = CARTESIAN_POINT ( 'NONE',  ( 95.00630608762466522, -4.999999999999991118, 69.02612180135393771 ) ) ;
#24194 = CARTESIAN_POINT ( 'NONE',  ( -7.347286611336976136, -4.995646404165301036, -4.503039949738237624 ) ) ;
#24195 = DIRECTION ( 'NONE',  ( -0.000000000000000000, 0.000000000000000000, 1.000000000000000000 ) ) ;
#24196 = SURFACE_SIDE_STYLE ('',( #17606 ) ) ;
#24197 = CARTESIAN_POINT ( 'NONE',  ( 19.71807001554888217, -1.708786246101231532, -19.21472004699903380 ) ) ;
#24198 = EDGE_LOOP ( 'NONE', ( #14942, #26334, #16161, #12440 ) ) ;
#24199 = DIRECTION ( 'NONE',  ( 1.000000000000000000, 0.000000000000000000, 0.000000000000000000 ) ) ;
#24200 = CARTESIAN_POINT ( 'NONE',  ( 10.74108227847380448, 16.53813910199176007, -15.94580854828543437 ) ) ;
#24201 = CARTESIAN_POINT ( 'NONE',  ( 32.96569147872224903, -11.36116021242123608, -19.12347989294568151 ) ) ;
#24202 = CARTESIAN_POINT ( 'NONE',  ( 164.5152310637604671, -9.999999999999998224, -21.71180489736091346 ) ) ;
#24203 = VECTOR ( 'NONE', #28823, 1000.000000000000000 ) ;
#24204 = CARTESIAN_POINT ( 'NONE',  ( 25.36810815240369621, -0.9165050883202133791, -18.11329069065276443 ) ) ;
#24205 = CARTESIAN_POINT ( 'NONE',  ( 18.57670912428364574, -0.2836015139962214660, -15.28694485256269608 ) ) ;
#24206 = ORIENTED_EDGE ( 'NONE', *, *, #4361, .F. ) ;
#24207 = CARTESIAN_POINT ( 'NONE',  ( 35.18065281855160720, -20.53155141575438591, -20.22037173032050461 ) ) ;
#24208 =( NAMED_UNIT ( * ) SI_UNIT ( $, .STERADIAN. ) SOLID_ANGLE_UNIT ( ) );
#24209 = CARTESIAN_POINT ( 'NONE',  ( 23.29143545295710638, -10.05536756138072718, -15.72373794962660831 ) ) ;
#24210 = VECTOR ( 'NONE', #15877, 1000.000000000000000 ) ;
#24211 = CARTESIAN_POINT ( 'NONE',  ( 26.15289264771154620, -4.614421047071551207, -20.21764904625508663 ) ) ;
#24212 = COLOUR_RGB ( '', 0.40784314, 0.44705882, 0.49803922) ;
#24213 = ORIENTED_EDGE ( 'NONE', *, *, #8281, .F. ) ;
#24214 = CARTESIAN_POINT ( 'NONE',  ( 23.29338531092689735, -7.078548041224526521, -17.51562821661096336 ) ) ;
#24215 = PRODUCT_DEFINITION_SHAPE ( 'NONE', 'NONE',  #4667 ) ;
#24216 = ORIENTED_EDGE ( 'NONE', *, *, #5333, .F. ) ;
#24217 = CARTESIAN_POINT ( 'NONE',  ( 36.04859390953723874, -22.18451583373416014, -15.00000000000000000 ) ) ;
#24218 = ORIENTED_EDGE ( 'NONE', *, *, #23210, .F. ) ;
#24219 = DIRECTION ( 'NONE',  ( 0.000000000000000000, -1.000000000000000000, 0.000000000000000000 ) ) ;
#24220 = DIRECTION ( 'NONE',  ( 8.163404592832029035E-16, 2.202861047501738386E-31, 1.000000000000000000 ) ) ;
#24221 = FACE_OUTER_BOUND ( 'NONE', #1082, .T. ) ;
#24222 = AXIS2_PLACEMENT_3D ( 'NONE', #975, #29400, #19715 ) ;
#24223 = EDGE_CURVE ( 'NONE', #12383, #590, #17569, .T. ) ;
#24224 = CARTESIAN_POINT ( 'NONE',  ( 18.04976943019953239, 10.79320383120880145, -15.74583687248850161 ) ) ;
#24225 = CARTESIAN_POINT ( 'NONE',  ( 36.13838427452936486, -20.34166123773320578, -20.43658233646779365 ) ) ;
#24226 = VECTOR ( 'NONE', #25810, 1000.000000000000000 ) ;
#24227 = CARTESIAN_POINT ( 'NONE',  ( 9.916118674515717046, 16.40877069192658055, -16.50468880802031890 ) ) ;
#24228 = LINE ( 'NONE', #1036, #27887 ) ;
#24229 = FACE_OUTER_BOUND ( 'NONE', #27173, .T. ) ;
#24230 = CARTESIAN_POINT ( 'NONE',  ( 12.02305193244137449, 9.338961869187645704, -16.69339841729684437 ) ) ;
#24231 = CARTESIAN_POINT ( 'NONE',  ( 6.505213034913026604E-15, 9.237604307034033013, -5.000000000000000888 ) ) ;
#24232 = CARTESIAN_POINT ( 'NONE',  ( 129.5152310637605524, -1.999999999999982236, -30.37205893520530964 ) ) ;
#24233 = ORIENTED_EDGE ( 'NONE', *, *, #21229, .T. ) ;
#24234 = CARTESIAN_POINT ( 'NONE',  ( -28.20515957282649921, 30.94299554780361206, 4.999999999999998224 ) ) ;
#24235 = DIRECTION ( 'NONE',  ( -2.698458740408365879E-16, 1.000000000000000000, 0.000000000000000000 ) ) ;
#24236 = FACE_OUTER_BOUND ( 'NONE', #5495, .T. ) ;
#24237 = ORIENTED_EDGE ( 'NONE', *, *, #8693, .F. ) ;
#24238 = EDGE_LOOP ( 'NONE', ( #5431, #24634, #25030, #22888 ) ) ;
#24239 = CARTESIAN_POINT ( 'NONE',  ( 11.22458689634746776, 9.088074461393535586, -17.24131758186684138 ) ) ;
#24240 = CARTESIAN_POINT ( 'NONE',  ( 29.81560109580191664, -6.784977964013398477, -14.56477501241906403 ) ) ;
#24241 = CARTESIAN_POINT ( 'NONE',  ( 24.14852421541024441, 0.2028892341458684023, -15.23052705399570428 ) ) ;
#24242 = STYLED_ITEM ( 'NONE', ( #4625 ), #11686 ) ;
#24243 = FACE_OUTER_BOUND ( 'NONE', #3229, .T. ) ;
#24244 = DIRECTION ( 'NONE',  ( 0.000000000000000000, 0.000000000000000000, -1.000000000000000000 ) ) ;
#24245 = CARTESIAN_POINT ( 'NONE',  ( 159.7287565553229456, -4.999999999999974243, -16.50000000000000000 ) ) ;
#24246 = EDGE_CURVE ( 'NONE', #2635, #26570, #22309, .T. ) ;
#24247 = VECTOR ( 'NONE', #29436, 1000.000000000000000 ) ;
#24248 = PRODUCT_RELATED_PRODUCT_CATEGORY ( 'part', '', ( #22019 ) ) ;
#24249 = ORIENTED_EDGE ( 'NONE', *, *, #16387, .F. ) ;
#24250 = LINE ( 'NONE', #19199, #9875 ) ;
#24251 = DIRECTION ( 'NONE',  ( -2.698458740408365879E-16, 1.000000000000000000, 0.000000000000000000 ) ) ;
#24253 = VERTEX_POINT ( 'NONE', #1263 ) ;
#24252 = CARTESIAN_POINT ( 'NONE',  ( 137.0152310637606092, -10.00000000000000533, -32.93883019725009120 ) ) ;
#24254 = LINE ( 'NONE', #21954, #20502 ) ;
#24255 = CARTESIAN_POINT ( 'NONE',  ( 141.1922820468854525, -10.00000000000000533, -30.91696583120935671 ) ) ;
#24256 = CARTESIAN_POINT ( 'NONE',  ( 12.02908293258818517, 9.311337566433326884, -16.69090174519279657 ) ) ;
#24257 = CARTESIAN_POINT ( 'NONE',  ( 33.23402178976249388, -11.79005478413273522, -18.03234444571244666 ) ) ;
#24258 = VERTEX_POINT ( 'NONE', #7964 ) ;
#24259 = CARTESIAN_POINT ( 'NONE',  ( 8.952973202525470242, 16.91312194274802749, -17.65238394630757313 ) ) ;
#24260 = AXIS2_PLACEMENT_3D ( 'NONE', #23511, #9454, #12202 ) ;
#24261 = CARTESIAN_POINT ( 'NONE',  ( 26.84970692451943819, -5.812874930055231815, -14.04107299160273037 ) ) ;
#24262 = CARTESIAN_POINT ( 'NONE',  ( 12.85536779349230052, 9.514564043964993445, -16.12538237964846388 ) ) ;
#24263 = FACE_BOUND ( 'NONE', #26100, .T. ) ;
#24264 = VERTEX_POINT ( 'NONE', #1416 ) ;
#24265 = AXIS2_PLACEMENT_3D ( 'NONE', #25969, #25660, #4750 ) ;
#24266 = DIRECTION ( 'NONE',  ( -0.8090169943749474513, -2.183098979609982436E-16, -0.5877852522924731371 ) ) ;
#24267 = CARTESIAN_POINT ( 'NONE',  ( 11.47029057985033340, 9.281140223223081520, -15.86198156829250117 ) ) ;
#24268 = CARTESIAN_POINT ( 'NONE',  ( 132.0152310637605524, -4.999999999999982236, -17.38167787843870826 ) ) ;
#24269 = VERTEX_POINT ( 'NONE', #5690 ) ;
#24270 = CARTESIAN_POINT ( 'NONE',  ( -1.310841663519413114, 7.511012776518211958E-16, -5.000000000000000000 ) ) ;
#24271 = ORIENTED_EDGE ( 'NONE', *, *, #1414, .F. ) ;
#24272 = CARTESIAN_POINT ( 'NONE',  ( 11.96327893486549776, 9.613088455355432771, -16.71811665443363992 ) ) ;
#24273 = EDGE_LOOP ( 'NONE', ( #477, #15278, #17872, #12433 ) ) ;
#24274 = CARTESIAN_POINT ( 'NONE',  ( 18.68383238644686273, 8.832144196210188980, -14.76942027321762119 ) ) ;
#24275 = CARTESIAN_POINT ( 'NONE',  ( 31.81434894052502571, -10.04473835610349575, -15.03854332269495764 ) ) ;
#24276 = CARTESIAN_POINT ( 'NONE',  ( 169.5152310637604955, -1.999999999999970024, -30.37205893520531319 ) ) ;
#24277 = ORIENTED_EDGE ( 'NONE', *, *, #3570, .F. ) ;
#24278 = PLANE ( 'NONE',  #16175 ) ;
#24279 = EDGE_CURVE ( 'NONE', #23249, #5618, #12479, .T. ) ;
#24280 = EDGE_CURVE ( 'NONE', #28906, #18615, #26923, .T. ) ;
#24281 = ORIENTED_EDGE ( 'NONE', *, *, #25110, .F. ) ;
#24282 = CARTESIAN_POINT ( 'NONE',  ( 20.63695664501197413, 4.642632487595073520, -17.05591670970450124 ) ) ;
#24283 = ADVANCED_FACE ( 'NONE', ( #28928 ), #24604, .F. ) ;
#24284 = CARTESIAN_POINT ( 'NONE',  ( 17.69365662292968366, 10.27476822432933545, -17.01437286930526227 ) ) ;
#24285 = AXIS2_PLACEMENT_3D ( 'NONE', #15330, #17189, #8171 ) ;
#24286 = CARTESIAN_POINT ( 'NONE',  ( 130.7287565553229456, -4.999999999999983125, -10.89389676854976408 ) ) ;
#24287 = AXIS2_PLACEMENT_3D ( 'NONE', #23637, #16155, #4565 ) ;
#24288 = DIRECTION ( 'NONE',  ( 0.5877852522924731371, 0.000000000000000000, 0.8090169943749474513 ) ) ;
#24289 = LINE ( 'NONE', #5671, #5291 ) ;
#24290 = LINE ( 'NONE', #15108, #6794 ) ;
#24291 = CARTESIAN_POINT ( 'NONE',  ( 10.00000000000008527, 17.32050807568872486, -23.00000000000000000 ) ) ;
#24292 = CARTESIAN_POINT ( 'NONE',  ( 12.27662779141079596, 9.495931643136637845, -15.31080646268338974 ) ) ;
#24293 = CARTESIAN_POINT ( 'NONE',  ( 2.500000000000000444, -1.178949249685215417, 2.042000000000002036 ) ) ;
#24294 = DIRECTION ( 'NONE',  ( -2.698458740408365879E-16, 1.000000000000000000, 0.000000000000000000 ) ) ;
#24295 = ORIENTED_EDGE ( 'NONE', *, *, #19958, .F. ) ;
#24296 = CARTESIAN_POINT ( 'NONE',  ( 11.47511325496290624, 9.259230714725578792, -15.85997136665693041 ) ) ;
#24297 = VERTEX_POINT ( 'NONE', #12692 ) ;
#24298 = AXIS2_PLACEMENT_3D ( 'NONE', #10205, #7626, #14632 ) ;
#24299 = CARTESIAN_POINT ( 'NONE',  ( 10.66893569228806271, 9.043500038842159583, -16.41109624600252559 ) ) ;
#24300 = CARTESIAN_POINT ( 'NONE',  ( 63.44486372867152824, 109.8897274573438096, -186.4312945166758482 ) ) ;
#24301 = DIRECTION ( 'NONE',  ( 0.000000000000000000, 0.000000000000000000, 1.000000000000000000 ) ) ;
#24302 = CARTESIAN_POINT ( 'NONE',  ( 169.5152310637604671, -4.999999999999971578, -21.71180489736091346 ) ) ;
#24303 = EDGE_LOOP ( 'NONE', ( #6, #5986, #23300, #13397, #24496 ) ) ;
#24304 = DIRECTION ( 'NONE',  ( 0.5877852522924731371, 1.586114251531760728E-16, -0.8090169943749474513 ) ) ;
#24305 = VERTEX_POINT ( 'NONE', #24017 ) ;
#24306 = CARTESIAN_POINT ( 'NONE',  ( 12.83230269852989203, 9.540395929213350001, -16.14101810565610151 ) ) ;
#24307 = VECTOR ( 'NONE', #233, 1000.000000000000000 ) ;
#24308 = CARTESIAN_POINT ( 'NONE',  ( 34.04598001273328833, -11.17175086900407166, -18.07582794505754364 ) ) ;
#24309 = CARTESIAN_POINT ( 'NONE',  ( 15.70491959545049987, 3.570626008024105680, -15.63470537622339229 ) ) ;
#24310 = VERTEX_POINT ( 'NONE', #22013 ) ;
#24311 = ORIENTED_EDGE ( 'NONE', *, *, #4124, .F. ) ;
#24312 = CARTESIAN_POINT ( 'NONE',  ( 174.5152310637604955, -4.999999999999969802, -28.60870317832789667 ) ) ;
#24313 = CARTESIAN_POINT ( 'NONE',  ( 20.37871551743239351, 7.600776799596193456, -17.08157252577618479 ) ) ;
#24314 = CARTESIAN_POINT ( 'NONE',  ( -4.000000000000003553, -6.938893903907228378E-15, 8.673617379884035472E-16 ) ) ;
#24315 = AXIS2_PLACEMENT_3D ( 'NONE', #10938, #15521, #27018 ) ;
#24316 = DIRECTION ( 'NONE',  ( 1.000000000000000000, 2.698458740408365879E-16, -1.110223024625156540E-16 ) ) ;
#24317 = SURFACE_STYLE_USAGE ( .BOTH. , #19716 ) ;
#24318 = EDGE_CURVE ( 'NONE', #28540, #29884, #10399, .T. ) ;
#24319 = CARTESIAN_POINT ( 'NONE',  ( 23.39789874936200320, -0.01207823811560896493, -14.43595595811700782 ) ) ;
#24320 = ADVANCED_FACE ( 'NONE', ( #26304 ), #19706, .T. ) ;
#24321 = CARTESIAN_POINT ( 'NONE',  ( 18.80130396411469462, -1.975481315223051704, -14.30362724594584378 ) ) ;
#24322 = EDGE_LOOP ( 'NONE', ( #16228, #3410, #958, #10152 ) ) ;
#24323 = ADVANCED_FACE ( 'NONE', ( #12389 ), #3261, .T. ) ;
#24324 = ORIENTED_EDGE ( 'NONE', *, *, #5368, .T. ) ;
#24325 = CARTESIAN_POINT ( 'NONE',  ( 138.6922820468854525, -10.00000000000000533, -23.73366926340167282 ) ) ;
#24326 = CARTESIAN_POINT ( 'NONE',  ( 178.7287565553229172, -1.999999999999968914, -33.50000000000000000 ) ) ;
#24327 = CARTESIAN_POINT ( 'NONE',  ( 3.660532965668829686, -7.124194613927648412, -1.188556631587234551E-14 ) ) ;
#24328 = VECTOR ( 'NONE', #6606, 1000.000000000000000 ) ;
#24329 = CARTESIAN_POINT ( 'NONE',  ( 148.6922820468853956, -10.00000000000000178, -9.266330736598359152 ) ) ;
#24330 = LINE ( 'NONE', #3423, #14348 ) ;
#24331 = CARTESIAN_POINT ( 'NONE',  ( 9.932908820165812003, 16.33176894372950727, -16.49774300651844072 ) ) ;
#24332 = COLOUR_RGB ( '', 0.09019608, 0.27058824, 0.51372549) ;
#24333 = CARTESIAN_POINT ( 'NONE',  ( 29.36168402625536444, -8.616725751243539122, -15.73432514746931155 ) ) ;
#24334 = CARTESIAN_POINT ( 'NONE',  ( 29.00434111665888182, -5.389956126880047549, -17.18324766788818181 ) ) ;
#24335 = LINE ( 'NONE', #7993, #800 ) ;
#24336 = LINE ( 'NONE', #26336, #6764 ) ;
#24337 = DIRECTION ( 'NONE',  ( 1.000000000000000000, 0.000000000000000000, 0.000000000000000000 ) ) ;
#24338 = LINE ( 'NONE', #26491, #21460 ) ;
#24339 = CARTESIAN_POINT ( 'NONE',  ( 133.7287565553229172, -4.999999999999982236, -33.50000000000000000 ) ) ;
#24340 = CARTESIAN_POINT ( 'NONE',  ( 23.16390915794477223, 2.882539813099532555, -14.99485278278146438 ) ) ;
#24341 = ORIENTED_EDGE ( 'NONE', *, *, #27136, .F. ) ;
#24342 = DIRECTION ( 'NONE',  ( -0.000000000000000000, -0.000000000000000000, -1.000000000000000000 ) ) ;
#24343 = CARTESIAN_POINT ( 'NONE',  ( 12.27662779141079596, 9.495931643136637845, -15.31080646268338974 ) ) ;
#24344 = CARTESIAN_POINT ( 'NONE',  ( 31.39893620166130717, -10.86152586746012183, -14.84747879817187943 ) ) ;
#24345 = DIRECTION ( 'NONE',  ( 1.000000000000000000, 2.908569913943825554E-16, -6.938893903907227392E-16 ) ) ;
#24346 = VECTOR ( 'NONE', #27564, 999.9999999999998863 ) ;
#24347 = CARTESIAN_POINT ( 'NONE',  ( 19.18841159021359033, -2.222386543571284179, -18.22349448661670834 ) ) ;
#24348 = DIRECTION ( 'NONE',  ( 1.000000000000000000, 0.000000000000000000, 0.000000000000000000 ) ) ;
#24349 = CARTESIAN_POINT ( 'NONE',  ( 22.38244025736702625, 4.876565640102752397, -15.59977576251379539 ) ) ;
#24350 = ORIENTED_EDGE ( 'NONE', *, *, #25484, .T. ) ;
#24351 = CARTESIAN_POINT ( 'NONE',  ( 132.0152310637605808, -1.999999999999981348, -15.61832212156129351 ) ) ;
#24352 = SURFACE_SIDE_STYLE ('',( #19914 ) ) ;
#24353 = CIRCLE ( 'NONE', #27333, 3.000000000000002665 ) ;
#24354 = CARTESIAN_POINT ( 'NONE',  ( 27.13218800474287207, -6.260320175479137106, -19.66075965151719984 ) ) ;
#24355 = CARTESIAN_POINT ( 'NONE',  ( 24.97326132480219485, 0.3353791038140019887, -18.64228740943764961 ) ) ;
#24356 = ADVANCED_FACE ( 'NONE', ( #26456 ), #24454, .T. ) ;
#24357 = EDGE_CURVE ( 'NONE', #4081, #28996, #14821, .T. ) ;
#24358 = EDGE_CURVE ( 'NONE', #26561, #1053, #10246, .T. ) ;
#24359 = CIRCLE ( 'NONE', #3877, 8.000000000000005329 ) ;
#24360 = EDGE_CURVE ( 'NONE', #30087, #11783, #23072, .T. ) ;
#24361 = ORIENTED_EDGE ( 'NONE', *, *, #11864, .F. ) ;
#24362 = CARTESIAN_POINT ( 'NONE',  ( 27.26129135193747999, -10.77754955263135095, -18.64424489656416739 ) ) ;
#24363 = FACE_OUTER_BOUND ( 'NONE', #22967, .T. ) ;
#24364 = EDGE_LOOP ( 'NONE', ( #7289, #12084, #21787, #24190 ) ) ;
#24365 = CARTESIAN_POINT ( 'NONE',  ( 127.7287565553229740, -1.999999999999982681, 0.5000000000000397460 ) ) ;
#24366 = CARTESIAN_POINT ( 'NONE',  ( 176.1922820468853388, -9.999999999999994671, -28.06379628232387802 ) ) ;
#24367 = DIRECTION ( 'NONE',  ( -0.8090169943749474513, -2.183098979609982436E-16, -0.5877852522924731371 ) ) ;
#24368 = CARTESIAN_POINT ( 'NONE',  ( 13.93491968177131923, 5.624373287173536795, -18.66784319378200863 ) ) ;
#24369 = CARTESIAN_POINT ( 'NONE',  ( 36.35800453371076202, -21.32829872614925648, -20.07395605779921155 ) ) ;
#24370 = CONICAL_SURFACE ( 'NONE', #28822, 5.999999999999983125, 0.7853981633974496113 ) ;
#24371 = CARTESIAN_POINT ( 'NONE',  ( 11.45661370752365116, 9.343864103108954211, -15.86763743611193789 ) ) ;
#24372 = VECTOR ( 'NONE', #29722, 1000.000000000000000 ) ;
#24373 = CARTESIAN_POINT ( 'NONE',  ( 0.000000000000000000, 0.000000000000000000, -2.450000000000000178 ) ) ;
#24374 = CARTESIAN_POINT ( 'NONE',  ( 13.00000000000000178, -2.870178842070716726E-15, 18.00000000000000000 ) ) ;
#24375 = CARTESIAN_POINT ( 'NONE',  ( 13.12723341905928898, 8.572452836447732594, -15.90902281579132449 ) ) ;
#24376 = LINE ( 'NONE', #24231, #6836 ) ;
#24377 = ORIENTED_EDGE ( 'NONE', *, *, #16690, .T. ) ;
#24378 = CARTESIAN_POINT ( 'NONE',  ( 17.51600279482502742, -5.000000000000013323, -53.90871343874875521 ) ) ;
#24379 = EDGE_LOOP ( 'NONE', ( #27579, #13553 ) ) ;
#24380 = CARTESIAN_POINT ( 'NONE',  ( 133.6922820468853956, -1.999999999999980904, -23.73366926340167282 ) ) ;
#24381 = LINE ( 'NONE', #1191, #3457 ) ;
#24382 = CARTESIAN_POINT ( 'NONE',  ( 147.0152310637605808, -4.999999999999977796, -34.70218595412750773 ) ) ;
#24383 = ORIENTED_EDGE ( 'NONE', *, *, #27824, .T. ) ;
#24384 = ORIENTED_EDGE ( 'NONE', *, *, #25877, .F. ) ;
#24385 = CARTESIAN_POINT ( 'NONE',  ( 11.22390034614927856, 9.091215689738174177, -17.24160205726399653 ) ) ;
#24386 = AXIS2_PLACEMENT_3D ( 'NONE', #22610, #12989, #2020 ) ;
#24387 = CARTESIAN_POINT ( 'NONE',  ( 30.75621536574076487, -10.42133643238263829, -12.14063830390948517 ) ) ;
#24388 = AXIS2_PLACEMENT_3D ( 'NONE', #3884, #29731, #8739 ) ;
#24389 = EDGE_CURVE ( 'NONE', #28330, #2176, #2026, .T. ) ;
#24390 = CARTESIAN_POINT ( 'NONE',  ( 22.75855789899217640, -7.280205122891536540, -14.30210469086359915 ) ) ;
#24391 = DIRECTION ( 'NONE',  ( -0.000000000000000000, -0.000000000000000000, -1.000000000000000000 ) ) ;
#24392 = FACE_OUTER_BOUND ( 'NONE', #29851, .T. ) ;
#24393 = DIRECTION ( 'NONE',  ( -1.110223024625156540E-16, 0.000000000000000000, -1.000000000000000000 ) ) ;
#24394 = LINE ( 'NONE', #733, #133 ) ;
#24395 = EDGE_CURVE ( 'NONE', #23922, #19336, #22771, .T. ) ;
#24396 = VECTOR ( 'NONE', #4998, 1000.000000000000000 ) ;
#24397 = ORIENTED_EDGE ( 'NONE', *, *, #12763, .F. ) ;
#24398 = CARTESIAN_POINT ( 'NONE',  ( 142.0152310637606092, -4.999999999999978684, -15.61832212156129707 ) ) ;
#24400 = EDGE_LOOP ( 'NONE', ( #28092, #8546, #3540 ) ) ;
#24399 = DIRECTION ( 'NONE',  ( 0.000000000000000000, 1.000000000000000000, 0.000000000000000000 ) ) ;
#24401 = VERTEX_POINT ( 'NONE', #8558 ) ;
#24402 = DIRECTION ( 'NONE',  ( -0.000000000000000000, -0.000000000000000000, -1.000000000000000000 ) ) ;
#24403 = DIRECTION ( 'NONE',  ( -2.698458740408365879E-16, 1.000000000000000000, 0.000000000000000000 ) ) ;
#24404 = B_SPLINE_CURVE_WITH_KNOTS ( 'NONE', 3,
 ( #22186, #21593, #24049, #10586 ),
 .UNSPECIFIED., .F., .F.,
 ( 4, 4 ),
 ( 2.380737582341110265E-07, 0.002336974151641603697 ),
 .UNSPECIFIED. ) ;
#24405 = VECTOR ( 'NONE', #6217, 1000.000000000000000 ) ;
#24406 = CARTESIAN_POINT ( 'NONE',  ( 12.50603416232391929, 8.608717614871036261, -16.38042650914619358 ) ) ;
#24407 = CARTESIAN_POINT ( 'NONE',  ( 33.20927704557755789, -11.78629111679139996, -17.96241082601573424 ) ) ;
#24408 = VERTEX_POINT ( 'NONE', #8858 ) ;
#24409 = VECTOR ( 'NONE', #13139, 1000.000000000000000 ) ;
#24410 = CARTESIAN_POINT ( 'NONE',  ( 9.101278670497288559, 16.23297416207913813, -17.06093009358445300 ) ) ;
#24411 = CARTESIAN_POINT ( 'NONE',  ( 25.04068920418659161, -5.475481712173364990, -18.92835678451453774 ) ) ;
#24412 = CARTESIAN_POINT ( 'NONE',  ( 10.35864953657871190, 16.97212341857210660, -17.91436492910080247 ) ) ;
#24413 = FACE_BOUND ( 'NONE', #29790, .T. ) ;
#24414 = EDGE_CURVE ( 'NONE', #17911, #10566, #25208, .T. ) ;
#24415 =( GEOMETRIC_REPRESENTATION_CONTEXT ( 3 ) GLOBAL_UNCERTAINTY_ASSIGNED_CONTEXT ( ( #22640 ) ) GLOBAL_UNIT_ASSIGNED_CONTEXT ( ( #18116, #27024, #15531 ) ) REPRESENTATION_CONTEXT ( 'NONE', 'WORKASPACE' ) );
#24416 = ORIENTED_EDGE ( 'NONE', *, *, #24527, .T. ) ;
#24417 = DIRECTION ( 'NONE',  ( 0.000000000000000000, 0.000000000000000000, -1.000000000000000000 ) ) ;
#24418 = CARTESIAN_POINT ( 'NONE',  ( 12.49957999542663600, 8.570517509188613658, -15.13050969259218981 ) ) ;
#24419 = CARTESIAN_POINT ( 'NONE',  ( 177.2287565553228319, -9.999999999999994671, -3.509618943233403510 ) ) ;
#24420 = ORIENTED_EDGE ( 'NONE', *, *, #819, .T. ) ;
#24421 = FACE_OUTER_BOUND ( 'NONE', #18650, .T. ) ;
#24422 = VERTEX_POINT ( 'NONE', #11306 ) ;
#24423 = CARTESIAN_POINT ( 'NONE',  ( 13.01452397926061089, 8.532813591658360508, -15.99807864679971026 ) ) ;
#24424 = ORIENTED_EDGE ( 'NONE', *, *, #23877, .F. ) ;
#24425 = CARTESIAN_POINT ( 'NONE',  ( 22.44359388949645151, 4.989503210053415572, -18.93028356096972686 ) ) ;
#24426 = CARTESIAN_POINT ( 'NONE',  ( 20.05201200715256249, 8.675301412908657639, -18.33989206490851842 ) ) ;
#24427 = CARTESIAN_POINT ( 'NONE',  ( 132.0152310637605808, -1.999999999999981348, 1.702185954127501066 ) ) ;
#24428 = ORIENTED_EDGE ( 'NONE', *, *, #29650, .T. ) ;
#24429 = CARTESIAN_POINT ( 'NONE',  ( 35.70376052765831787, -18.38912696963886617, -20.33459093173238941 ) ) ;
#24430 = CIRCLE ( 'NONE', #19054, 4.250000000000003553 ) ;
#24431 = PRODUCT_CONTEXT ( 'NONE', #16112, 'mechanical' ) ;
#24432 = EDGE_LOOP ( 'NONE', ( #19849, #20234, #16536, #26767 ) ) ;
#24433 = VECTOR ( 'NONE', #4078, 1000.000000000000000 ) ;
#24434 = CARTESIAN_POINT ( 'NONE',  ( 19.51440197245297270, 8.071880087464508691, -17.28625796899888201 ) ) ;
#24435 = PLANE ( 'NONE',  #3723 ) ;
#24436 = FACE_BOUND ( 'NONE', #18670, .T. ) ;
#24437 = CARTESIAN_POINT ( 'NONE',  ( 171.1922820468853104, -9.999999999999996447, -13.59645775552055902 ) ) ;
#24438 = CARTESIAN_POINT ( 'NONE',  ( 34.11209566957792561, -15.73109017586260272, -19.92372960426217787 ) ) ;
#24439 = DIRECTION ( 'NONE',  ( 1.000000000000000000, 0.000000000000000000, -0.000000000000000000 ) ) ;
#24440 = ORIENTED_EDGE ( 'NONE', *, *, #7498, .F. ) ;
#24441 = DIRECTION ( 'NONE',  ( -2.698458740408365879E-16, 1.000000000000000000, 0.000000000000000000 ) ) ;
#24442 = CARTESIAN_POINT ( 'NONE',  ( 12.23642031952448406, 9.680328234467932447, -15.32743366668982432 ) ) ;
#24443 = DIRECTION ( 'NONE',  ( 0.3090169943749472292, 8.338696094057992503E-17, -0.9510565162951536422 ) ) ;
#24444 = ADVANCED_FACE ( 'NONE', ( #27679 ), #11023, .F. ) ;
#24445 = PLANE ( 'NONE',  #22766 ) ;
#24446 = ORIENTED_EDGE ( 'NONE', *, *, #28068, .F. ) ;
#24447 = AXIS2_PLACEMENT_3D ( 'NONE', #10283, #1003, #5724 ) ;
#24448 = CARTESIAN_POINT ( 'NONE',  ( 12.46899830068120352, 8.557956911948249257, -15.15481108270911825 ) ) ;
#24449 = EDGE_LOOP ( 'NONE', ( #6291, #5932, #28819, #10553 ) ) ;
#24450 = CARTESIAN_POINT ( 'NONE',  ( 12.72406076201818870, 7.612173793771704666, -14.95155764689848965 ) ) ;
#24451 = DIRECTION ( 'NONE',  ( 1.000000000000000000, 4.440892098500622217E-16, 0.000000000000000000 ) ) ;
#24452 = LINE ( 'NONE', #29220, #2313 ) ;
#24453 = ORIENTED_EDGE ( 'NONE', *, *, #5894, .F. ) ;
#24454 = PLANE ( 'NONE',  #26662 ) ;
#24455 = ORIENTED_EDGE ( 'NONE', *, *, #24663, .T. ) ;
#24456 = CARTESIAN_POINT ( 'NONE',  ( 12.79171442625009547, 9.726534347120292523, -16.15780313276466273 ) ) ;
#24457 = CARTESIAN_POINT ( 'NONE',  ( 33.63214571818804188, -11.07540017893869866, -16.92567501773416794 ) ) ;
#24458 = CARTESIAN_POINT ( 'NONE',  ( 21.54098841764929873, -5.100688324319140321, -15.19385678519978633 ) ) ;
#24459 = EDGE_LOOP ( 'NONE', ( #20947, #23194, #1153, #30158 ) ) ;
#24460 = VERTEX_POINT ( 'NONE', #22471 ) ;
#24461 = CARTESIAN_POINT ( 'NONE',  ( 139.7287565553230309, -1.999999999999978684, -16.50000000000000000 ) ) ;
#24462 = CARTESIAN_POINT ( 'NONE',  ( 25.88562516208081021, -13.15641406947225889, -17.87304489109560990 ) ) ;
#24463 = VERTEX_POINT ( 'NONE', #4299 ) ;
#24464 = LINE ( 'NONE', #26938, #26169 ) ;
#24465 =( LENGTH_UNIT ( ) NAMED_UNIT ( * ) SI_UNIT ( .MILLI., .METRE. ) );
#24466 = EDGE_CURVE ( 'NONE', #1114, #9138, #10848, .T. ) ;
#24467 = CARTESIAN_POINT ( 'NONE',  ( 20.97044927184332508, -4.289323992320570156, -15.06659861376252429 ) ) ;
#24468 = CARTESIAN_POINT ( 'NONE',  ( 17.21229802721762780, 1.518872817929493912, -15.34595729721386448 ) ) ;
#24469 = ORIENTED_EDGE ( 'NONE', *, *, #15853, .T. ) ;
#24470 = ORIENTED_EDGE ( 'NONE', *, *, #4408, .F. ) ;
#24471 = VECTOR ( 'NONE', #4481, 1000.000000000000000 ) ;
#24472 = CARTESIAN_POINT ( 'NONE',  ( -20.00000000000017053, 34.64101615137744972, 4.999999999999998224 ) ) ;
#24473 = DIRECTION ( 'NONE',  ( 0.5877852522924731371, 1.586114251531760728E-16, 0.8090169943749474513 ) ) ;
#24474 = DIRECTION ( 'NONE',  ( -0.5000000000000051070, 0.000000000000000000, 0.8660254037844355990 ) ) ;
#24475 = LINE ( 'NONE', #3572, #7648 ) ;
#24476 = CARTESIAN_POINT ( 'NONE',  ( -8.000000000000001776, -4.336808689942017736E-15, -5.000000000000000888 ) ) ;
#24477 = CYLINDRICAL_SURFACE ( 'NONE', #18750, 13.00000000000000178 ) ;
#24478 = ORIENTED_EDGE ( 'NONE', *, *, #16137, .F. ) ;
#24479 = CARTESIAN_POINT ( 'NONE',  ( 11.34314632229486364, 9.864239995495806212, -15.91456019135469013 ) ) ;
#24480 = CARTESIAN_POINT ( 'NONE',  ( 15.73644607668725826, 9.740111719757674535, -14.94734896276200153 ) ) ;
#24481 = CARTESIAN_POINT ( 'NONE',  ( 27.03959252790357581, -7.665547941290169476, -19.57376043866218041 ) ) ;
#24482 = ADVANCED_FACE ( 'NONE', ( #20157 ), #20609, .T. ) ;
#24483 = ADVANCED_FACE ( 'NONE', ( #22616 ), #6588, .T. ) ;
#24484 = VERTEX_POINT ( 'NONE', #29996 ) ;
#24485 = PLANE ( 'NONE',  #20285 ) ;
#24486 = DIRECTION ( 'NONE',  ( 0.5877852522924731371, 1.586114251531760728E-16, -0.8090169943749474513 ) ) ;
#24487 = CARTESIAN_POINT ( 'NONE',  ( 10.55189716074911921, 7.593251366112849787, 4.999999999999998224 ) ) ;
#24488 = LINE ( 'NONE', #19444, #12261 ) ;
#24489 = EDGE_CURVE ( 'NONE', #27390, #24692, #8101, .T. ) ;
#24490 = VECTOR ( 'NONE', #9319, 1000.000000000000000 ) ;
#24491 = CARTESIAN_POINT ( 'NONE',  ( 157.0152310637604671, -1.999999999999974909, 1.702185954127501066 ) ) ;
#24492 = LINE ( 'NONE', #8447, #9314 ) ;
#24493 = EDGE_CURVE ( 'NONE', #21438, #436, #13440, .T. ) ;
#24495 = ORIENTED_EDGE ( 'NONE', *, *, #9998, .T. ) ;
#24494 = CARTESIAN_POINT ( 'NONE',  ( 19.23836061553175369, 5.151828676608854352, -13.99136221198299168 ) ) ;
#24496 = ORIENTED_EDGE ( 'NONE', *, *, #14435, .T. ) ;
#24497 = CARTESIAN_POINT ( 'NONE',  ( 141.1922820468854525, -4.999999999999980460, -13.59645775552055902 ) ) ;
#24498 = CARTESIAN_POINT ( 'NONE',  ( 12.27693553943969818, 9.494520259125854622, -15.31067919898749352 ) ) ;
#24499 = ORIENTED_EDGE ( 'NONE', *, *, #409, .F. ) ;
#24500 = PLANE ( 'NONE',  #17357 ) ;
#24501 = FACE_OUTER_BOUND ( 'NONE', #4483, .T. ) ;
#24502 = ORIENTED_EDGE ( 'NONE', *, *, #22536, .F. ) ;
#24503 = CARTESIAN_POINT ( 'NONE',  ( 22.39939798857497877, 2.694615832958070722, -14.02792042734668065 ) ) ;
#24504 = CARTESIAN_POINT ( 'NONE',  ( 171.1922820468852819, -4.999999999999971578, -4.936203717676158398 ) ) ;
#24505 = CARTESIAN_POINT ( 'NONE',  ( 15.19363621961471722, 2.181190162186355419, -17.24139079752846015 ) ) ;
#24506 = ORIENTED_EDGE ( 'NONE', *, *, #20963, .T. ) ;
#24507 = DIRECTION ( 'NONE',  ( -1.000000000000000000, 0.000000000000000000, 0.000000000000000000 ) ) ;
#24508 = CARTESIAN_POINT ( 'NONE',  ( 24.09482019364002880, -4.431952660107454811, -19.05667854325333721 ) ) ;
#24509 = CIRCLE ( 'NONE', #2102, 5.000000000000000000 ) ;
#24510 = CARTESIAN_POINT ( 'NONE',  ( 20.25494212361869728, -4.857969563408182090, -14.64469595162225701 ) ) ;
#24511 = CARTESIAN_POINT ( 'NONE',  ( 139.5152310637606092, -1.999999999999978684, -11.28819510263909542 ) ) ;
#24512 = VECTOR ( 'NONE', #4088, 1000.000000000000000 ) ;
#24513 = CARTESIAN_POINT ( 'NONE',  ( 132.2287565553230024, -10.00000000000000888, -12.16987298107780013 ) ) ;
#24514 = ORIENTED_EDGE ( 'NONE', *, *, #3135, .F. ) ;
#24515 = DIRECTION ( 'NONE',  ( 0.000000000000000000, 2.775557561562890735E-17, -1.000000000000000000 ) ) ;
#24516 = DIRECTION ( 'NONE',  ( -0.8191520442889943521, -2.634593911900098464E-16, 0.5735764363510424957 ) ) ;
#24517 = DIRECTION ( 'NONE',  ( -0.8090169943749474513, -2.183098979609982436E-16, -0.5877852522924731371 ) ) ;
#24518 = CARTESIAN_POINT ( 'NONE',  ( 8.000000000000015987, -1.555946510856143883, -0.06708870216336296211 ) ) ;
#24519 = CARTESIAN_POINT ( 'NONE',  ( 26.91914097958202845, -7.808663323052361882, -12.67700453112951209 ) ) ;
#24520 = LINE ( 'NONE', #21772, #23388 ) ;
#24521 = CARTESIAN_POINT ( 'NONE',  ( 34.91913293194685508, -14.86421081092256280, -20.09741683264573808 ) ) ;
#24522 = PLANE ( 'NONE',  #25142 ) ;
#24523 = CARTESIAN_POINT ( 'NONE',  ( 11.46269231744662420, 9.315986823159681407, -15.86512371708112212 ) ) ;
#24524 = EDGE_CURVE ( 'NONE', #5689, #7473, #25357, .T. ) ;
#24525 = CARTESIAN_POINT ( 'NONE',  ( 146.1922820468854241, -1.999999999999978018, -19.40354224447947828 ) ) ;
#24526 = LINE ( 'NONE', #29302, #30065 ) ;
#24527 = EDGE_CURVE ( 'NONE', #16899, #1878, #11001, .T. ) ;
#24528 = EDGE_CURVE ( 'NONE', #3207, #17958, #8708, .T. ) ;
#24529 = CARTESIAN_POINT ( 'NONE',  ( 9.661883061612440926, 16.25482663361732705, -17.92454625180715411 ) ) ;
#24530 = LINE ( 'NONE', #3621, #23910 ) ;
#24531 = EDGE_CURVE ( 'NONE', #23037, #15699, #13744, .T. ) ;
#24532 = DIRECTION ( 'NONE',  ( -2.698458740408365879E-16, 1.000000000000000000, 0.000000000000000000 ) ) ;
#24533 = ORIENTED_EDGE ( 'NONE', *, *, #24142, .F. ) ;
#24534 = DIRECTION ( 'NONE',  ( -1.110223024625156540E-16, 0.000000000000000000, -1.000000000000000000 ) ) ;
#24535 = DIRECTION ( 'NONE',  ( 0.000000000000000000, 0.000000000000000000, -1.000000000000000000 ) ) ;
#24536 = CARTESIAN_POINT ( 'NONE',  ( 0.000000000000000000, 0.000000000000000000, -5.000000000000000888 ) ) ;
#24538 = VERTEX_POINT ( 'NONE', #1715 ) ;
#24537 = VECTOR ( 'NONE', #12149, 1000.000000000000000 ) ;
#24539 = ORIENTED_EDGE ( 'NONE', *, *, #15916, .T. ) ;
#24540 = ORIENTED_EDGE ( 'NONE', *, *, #6407, .F. ) ;
#24541 = CARTESIAN_POINT ( 'NONE',  ( 8.944584683310379702, 16.95159276115599667, -17.92454625180715411 ) ) ;
#24542 = ORIENTED_EDGE ( 'NONE', *, *, #2314, .F. ) ;
#24543 = CARTESIAN_POINT ( 'NONE',  ( 17.55932102202221046, 11.64018535857498193, -15.95102284318303276 ) ) ;
#24544 = CARTESIAN_POINT ( 'NONE',  ( 23.87675077653036126, -6.787291307973906562, -13.16608595595566733 ) ) ;
#24545 = DIRECTION ( 'NONE',  ( 1.110223024625156540E-16, 2.995891024602366092E-32, 1.000000000000000000 ) ) ;
#24546 = CARTESIAN_POINT ( 'NONE',  ( 173.6922820468853104, -4.999999999999969802, -17.92658477444275889 ) ) ;
#24547 = DIRECTION ( 'NONE',  ( -0.8090169943749474513, -2.183098979609982436E-16, 0.5877852522924731371 ) ) ;
#24548 = VERTEX_POINT ( 'NONE', #11447 ) ;
#24549 = CARTESIAN_POINT ( 'NONE',  ( 6.783682487892742863, -5.000000000000015987, 20.87802791441155037 ) ) ;
#24551 = ORIENTED_EDGE ( 'NONE', *, *, #17003, .T. ) ;
#24550 = FACE_OUTER_BOUND ( 'NONE', #4540, .T. ) ;
#24552 = DIRECTION ( 'NONE',  ( -0.9510565162951536422, 0.000000000000000000, -0.3090169943749472292 ) ) ;
#24553 = FACE_OUTER_BOUND ( 'NONE', #11618, .T. ) ;
#24554 = CIRCLE ( 'NONE', #16746, 4.000000000000000000 ) ;
#24555 = CARTESIAN_POINT ( 'NONE',  ( 13.06976498004312326, 8.549601185932660385, -15.95463209657921055 ) ) ;
#24556 = CARTESIAN_POINT ( 'NONE',  ( 35.53434814243864537, -22.12051714835155281, -18.84852710552948096 ) ) ;
#24557 = EDGE_LOOP ( 'NONE', ( #25260, #19169, #8463, #27127 ) ) ;
#24558 = CARTESIAN_POINT ( 'NONE',  ( 10.58765414998594245, 9.416266744339480965, -16.44470908465386572 ) ) ;
#24559 = ORIENTED_EDGE ( 'NONE', *, *, #17484, .T. ) ;
#24560 = EDGE_CURVE ( 'NONE', #22451, #21981, #29386, .T. ) ;
#24561 = EDGE_CURVE ( 'NONE', #4559, #19382, #29695, .T. ) ;
#24562 = CARTESIAN_POINT ( 'NONE',  ( 22.51149892830068211, -1.106640851078940502, -13.23823320067571885 ) ) ;
#24563 = EDGE_CURVE ( 'NONE', #1679, #26232, #19175, .T. ) ;
#24564 = CARTESIAN_POINT ( 'NONE',  ( 12.87180867969543385, 9.517605834602926862, -16.11260084161717998 ) ) ;
#24565 = FACE_BOUND ( 'NONE', #12794, .T. ) ;
#24566 = ADVANCED_FACE ( 'NONE', ( #27835 ), #7342, .T. ) ;
#24567 = VERTEX_POINT ( 'NONE', #16641 ) ;
#24568 = EDGE_LOOP ( 'NONE', ( #6599, #24384, #11889, #9137 ) ) ;
#24569 = EDGE_LOOP ( 'NONE', ( #15527, #26410, #2469, #1722, #10094 ) ) ;
#24570 = DIRECTION ( 'NONE',  ( 1.000000000000000000, 2.891205793294675861E-16, 0.000000000000000000 ) ) ;
#24571 = CARTESIAN_POINT ( 'NONE',  ( 11.45256130090833935, 9.362448956408465861, -15.86931324879919991 ) ) ;
#24572 = DIRECTION ( 'NONE',  ( -2.698458740408365879E-16, 1.000000000000000000, 0.000000000000000000 ) ) ;
#24573 = ORIENTED_EDGE ( 'NONE', *, *, #13725, .T. ) ;
#24574 = LINE ( 'NONE', #28896, #23264 ) ;
#24575 = ORIENTED_EDGE ( 'NONE', *, *, #9051, .T. ) ;
#24576 = CARTESIAN_POINT ( 'NONE',  ( 9.661883062155979474, 16.25482663112457971, -17.91578995581314260 ) ) ;
#24577 = ORIENTED_EDGE ( 'NONE', *, *, #18422, .T. ) ;
#24578 = CARTESIAN_POINT ( 'NONE',  ( 13.44640266258695327, 6.638963897028184569, -16.15403403936744198 ) ) ;
#24579 = CARTESIAN_POINT ( 'NONE',  ( 21.84805831652669283, 4.237162156985878170, -20.00989837289113282 ) ) ;
#24580 = DIRECTION ( 'NONE',  ( -1.000000000000000000, 0.000000000000000000, 0.000000000000000000 ) ) ;
#24581 = VECTOR ( 'NONE', #27813, 1000.000000000000000 ) ;
#24582 = CARTESIAN_POINT ( 'NONE',  ( 36.54859390953724585, -22.18451583373416014, -18.06010107863414405 ) ) ;
#24583 = CARTESIAN_POINT ( 'NONE',  ( 15.39489021548154568, 6.697694061803245447, -14.95590323207311734 ) ) ;
#24584 = DIRECTION ( 'NONE',  ( 1.000000000000000000, 0.000000000000000000, 0.000000000000000000 ) ) ;
#24585 = CARTESIAN_POINT ( 'NONE',  ( 1.244173783436457737E-15, -5.000000000000017764, 0.000000000000000000 ) ) ;
#24586 = ORIENTED_EDGE ( 'NONE', *, *, #27585, .T. ) ;
#24587 = LINE ( 'NONE', #3679, #22924 ) ;
#24588 = CARTESIAN_POINT ( 'NONE',  ( 33.48796008207983022, -12.92717959506727965, -19.73506838908087246 ) ) ;
#24589 = LINE ( 'NONE', #3681, #19460 ) ;
#24590 = ORIENTED_EDGE ( 'NONE', *, *, #20622, .T. ) ;
#24591 = CARTESIAN_POINT ( 'NONE',  ( 164.5152310637604955, -9.999999999999996447, -30.37205893520531319 ) ) ;
#24592 = AXIS2_PLACEMENT_3D ( 'NONE', #24978, #5903, #4060 ) ;
#24593 = CARTESIAN_POINT ( 'NONE',  ( 11.05541599318665469, 17.68942028772053376, -17.91303167831651422 ) ) ;
#24594 = EDGE_CURVE ( 'NONE', #3702, #9337, #14819, .T. ) ;
#24595 = ORIENTED_EDGE ( 'NONE', *, *, #26560, .F. ) ;
#24596 = DIRECTION ( 'NONE',  ( -0.9510565162951536422, 0.000000000000000000, -0.3090169943749472292 ) ) ;
#24597 = ORIENTED_EDGE ( 'NONE', *, *, #24104, .F. ) ;
#24598 = FACE_OUTER_BOUND ( 'NONE', #13873, .T. ) ;
#24599 = VERTEX_POINT ( 'NONE', #6898 ) ;
#24600 = CARTESIAN_POINT ( 'NONE',  ( 12.74802704355670535, 7.622310320333636646, -14.93249076938322162 ) ) ;
#24601 = DIRECTION ( 'NONE',  ( -2.698458740408365879E-16, 1.000000000000000000, 0.000000000000000000 ) ) ;
#24602 = LINE ( 'NONE', #12689, #17871 ) ;
#24603 = ORIENTED_EDGE ( 'NONE', *, *, #22760, .T. ) ;
#24604 = PLANE ( 'NONE',  #17838 ) ;
#24605 = ORIENTED_EDGE ( 'NONE', *, *, #19745, .F. ) ;
#24606 = CARTESIAN_POINT ( 'NONE',  ( 12.83388176712078810, 9.535019011556107316, -16.14022287234750408 ) ) ;
#24607 = CARTESIAN_POINT ( 'NONE',  ( 33.96051107771264554, -11.12695408846492739, -17.85276550113785277 ) ) ;
#24608 = CARTESIAN_POINT ( 'NONE',  ( 18.34549112274340033, 0.9605221043122941227, -13.99314825615798341 ) ) ;
#24609 = VERTEX_POINT ( 'NONE', #11752 ) ;
#24610 = ORIENTED_EDGE ( 'NONE', *, *, #25974, .F. ) ;
#24611 = DIRECTION ( 'NONE',  ( 1.110223024625156540E-16, 2.995891024602366092E-32, 1.000000000000000000 ) ) ;
#24612 = CARTESIAN_POINT ( 'NONE',  ( 14.06424326207706699, 5.752694757912038881, -19.02294901845717945 ) ) ;
#24613 = CARTESIAN_POINT ( 'NONE',  ( 8.000000000000014211, -3.867591403079186030, -4.502324684675405031 ) ) ;
#24614 = DIRECTION ( 'NONE',  ( 1.000000000000000000, 0.000000000000000000, 0.000000000000000000 ) ) ;
#24615 = CARTESIAN_POINT ( 'NONE',  ( 27.50962693642323131, -9.092369620780022643, -12.61635453147917474 ) ) ;
#24616 = CARTESIAN_POINT ( 'NONE',  ( 19.45720675144774603, -0.6714082060231494342, -20.03460252700725519 ) ) ;
#24617 = VECTOR ( 'NONE', #28352, 1000.000000000000000 ) ;
#24618 = ORIENTED_EDGE ( 'NONE', *, *, #9842, .T. ) ;
#24619 = VERTEX_POINT ( 'NONE', #20910 ) ;
#24620 = ADVANCED_FACE ( 'NONE', ( #16486 ), #21070, .T. ) ;
#24621 = PLANE ( 'NONE',  #21553 ) ;
#24622 = LINE ( 'NONE', #8432, #12146 ) ;
#24623 = PLANE ( 'NONE',  #12328 ) ;
#24624 = VECTOR ( 'NONE', #23937, 1000.000000000000000 ) ;
#24625 = DIRECTION ( 'NONE',  ( 0.3090169943749472292, 8.338696094057992503E-17, -0.9510565162951536422 ) ) ;
#24626 = DIRECTION ( 'NONE',  ( -0.5877852522924731371, 0.000000000000000000, 0.8090169943749474513 ) ) ;
#24627 = CARTESIAN_POINT ( 'NONE',  ( 137.2287565553230309, -10.00000000000000533, -20.83012701892220164 ) ) ;
#24628 = CARTESIAN_POINT ( 'NONE',  ( 13.34629304935920757, 7.611730149031187054, -15.73439023580873730 ) ) ;
#24629 = CARTESIAN_POINT ( 'NONE',  ( 10.33811693838771717, 18.38618951776012267, -17.94384837343789130 ) ) ;
#24630 = CARTESIAN_POINT ( 'NONE',  ( 28.02603357813017482, -6.678172375388682802, -19.11289830413424440 ) ) ;
#24631 = ORIENTED_EDGE ( 'NONE', *, *, #1723, .T. ) ;
#24632 = CARTESIAN_POINT ( 'NONE',  ( 162.0152310637605240, -4.999999999999974243, -34.70218595412750773 ) ) ;
#24633 = PLANE ( 'NONE',  #10170 ) ;
#24634 = ORIENTED_EDGE ( 'NONE', *, *, #14855, .F. ) ;
#24635 = CARTESIAN_POINT ( 'NONE',  ( -6.689127551062014732, -5.375634714784644608, -4.682649155111332284 ) ) ;
#24636 = AXIS2_PLACEMENT_3D ( 'NONE', #12523, #947, #28600 ) ;
#24637 = PLANE ( 'NONE',  #24388 ) ;
#24638 = LINE ( 'NONE', #7855, #29317 ) ;
#24640 = VERTEX_POINT ( 'NONE', #2771 ) ;
#24639 = CARTESIAN_POINT ( 'NONE',  ( 26.58455406938135468, -5.910422570377376950, -13.89432871846328688 ) ) ;
#24641 = ORIENTED_EDGE ( 'NONE', *, *, #12336, .F. ) ;
#24642 = CARTESIAN_POINT ( 'NONE',  ( 0.000000000000000000, 0.000000000000000000, 15.00000000000000000 ) ) ;
#24643 = CARTESIAN_POINT ( 'NONE',  ( 10.98017426877725811, 15.44163275732038443, -15.84693559973663035 ) ) ;
#24644 = CARTESIAN_POINT ( 'NONE',  ( 32.63711423693117553, -11.05166607373017484, -18.34576405707344549 ) ) ;
#24645 = CARTESIAN_POINT ( 'NONE',  ( 133.6922820468854241, -10.00000000000000711, -0.6060766987539614181 ) ) ;
#24646 = ORIENTED_EDGE ( 'NONE', *, *, #6440, .F. ) ;
#24647 = CARTESIAN_POINT ( 'NONE',  ( 27.21278356834291756, -7.014839303453253905, -18.45691071023835761 ) ) ;
#24648 = FACE_OUTER_BOUND ( 'NONE', #8996, .T. ) ;
#24649 = CARTESIAN_POINT ( 'NONE',  ( 20.32371149932726695, 7.300285753667301591, -19.85501735805741319 ) ) ;
#24650 = VERTEX_POINT ( 'NONE', #16789 ) ;
#24651 = CARTESIAN_POINT ( 'NONE',  ( 35.54859390953724585, -22.18451583373416014, -17.99055332684694974 ) ) ;
#24652 = VECTOR ( 'NONE', #2842, 1000.000000000000000 ) ;
#24653 = FILL_AREA_STYLE ('',( #26817 ) ) ;
#24654 = CARTESIAN_POINT ( 'NONE',  ( 27.46460276834485370, -5.912627539431687396, -19.42860466253708296 ) ) ;
#24655 = CARTESIAN_POINT ( 'NONE',  ( 26.13670795350922660, -6.813068953109826076, -12.41955265015470999 ) ) ;
#24656 = VECTOR ( 'NONE', #18279, 1000.000000000000000 ) ;
#24657 = VERTEX_POINT ( 'NONE', #28433 ) ;
#24658 = ORIENTED_EDGE ( 'NONE', *, *, #775, .T. ) ;
#24659 = EDGE_CURVE ( 'NONE', #24756, #13323, #10451, .T. ) ;
#24660 = ADVANCED_FACE ( 'NONE', ( #23212 ), #9764, .T. ) ;
#24661 = CARTESIAN_POINT ( 'NONE',  ( 163.6922820468853956, -9.999999999999998224, -32.39392330124607611 ) ) ;
#24662 = VECTOR ( 'NONE', #2281, 1000.000000000000000 ) ;
#24663 = EDGE_CURVE ( 'NONE', #25233, #28576, #26196, .T. ) ;
#24664 = CONICAL_SURFACE ( 'NONE', #14872, 5.000000000000000888, 0.2131563744996338439 ) ;
#24665 = EDGE_CURVE ( 'NONE', #28903, #30129, #18780, .T. ) ;
#24666 = CARTESIAN_POINT ( 'NONE',  ( 138.6922820468854525, -10.00000000000000533, -26.58683881228715506 ) ) ;
#24667 = ORIENTED_EDGE ( 'NONE', *, *, #17215, .F. ) ;
#24668 = DIRECTION ( 'NONE',  ( -0.9510565162951536422, -2.566386769018988323E-16, 0.3090169943749475623 ) ) ;
#24669 = AXIS2_PLACEMENT_3D ( 'NONE', #5101, #20970, #27891 ) ;
#24670 = DIRECTION ( 'NONE',  ( 0.000000000000000000, 0.000000000000000000, 1.000000000000000000 ) ) ;
#24671 = CARTESIAN_POINT ( 'NONE',  ( 167.0152310637604103, -1.999999999999972244, -0.06116980274991495881 ) ) ;
#24672 = FACE_BOUND ( 'NONE', #2662, .T. ) ;
#24673 = CARTESIAN_POINT ( 'NONE',  ( 26.12748305362656254, -5.066878407431925524, -14.17679521427828071 ) ) ;
#24674 = FACE_OUTER_BOUND ( 'NONE', #6572, .T. ) ;
#24675 = CARTESIAN_POINT ( 'NONE',  ( 31.25429145842602452, -9.414624517878500853, -14.20845315089566441 ) ) ;
#24676 = DIRECTION ( 'NONE',  ( -0.5877852522924731371, -1.586114251531760235E-16, 0.8090169943749474513 ) ) ;
#24677 = CARTESIAN_POINT ( 'NONE',  ( 9.913797604922770290, 16.41941541294738727, -16.50570979788118464 ) ) ;
#24678 = VECTOR ( 'NONE', #21602, 1000.000000000000000 ) ;
#24679 = CARTESIAN_POINT ( 'NONE',  ( 134.5152310637605524, -10.00000000000000533, -4.391296821672111328 ) ) ;
#24680 = DIRECTION ( 'NONE',  ( 0.5877852522924731371, 1.586114251531760728E-16, -0.8090169943749474513 ) ) ;
#24681 = CARTESIAN_POINT ( 'NONE',  ( 9.661883061612440926, 16.25482663361732705, -17.91752729848688830 ) ) ;
#24682 = CARTESIAN_POINT ( 'NONE',  ( 168.6922820468853388, -4.999999999999971578, -15.07341522555727664 ) ) ;
#24683 = CARTESIAN_POINT ( 'NONE',  ( 137.0152310637605808, -1.999999999999979572, -26.04193191628310800 ) ) ;
#24684 = CARTESIAN_POINT ( 'NONE',  ( 11.47372892693763902, 9.265404009280679531, -15.86055721330185619 ) ) ;
#24685 = ORIENTED_EDGE ( 'NONE', *, *, #19958, .T. ) ;
#24686 = VECTOR ( 'NONE', #26496, 1000.000000000000000 ) ;
#24687 = CARTESIAN_POINT ( 'NONE',  ( 147.0152310637605808, -10.00000000000000178, -34.70218595412750773 ) ) ;
#24688 = CARTESIAN_POINT ( 'NONE',  ( 173.6922820468852535, -1.999999999999970912, -0.6060766987539614181 ) ) ;
#24689 = ORIENTED_EDGE ( 'NONE', *, *, #19814, .F. ) ;
#24690 = VECTOR ( 'NONE', #17107, 1000.000000000000000 ) ;
#24691 = CARTESIAN_POINT ( 'NONE',  ( 163.6922820468853104, -9.999999999999998224, -6.413161187712876909 ) ) ;
#24692 = VERTEX_POINT ( 'NONE', #4743 ) ;
#24693 = CARTESIAN_POINT ( 'NONE',  ( 8.944584683310379702, 16.95159276115599667, -17.92015940598198753 ) ) ;
#24694 = CARTESIAN_POINT ( 'NONE',  ( 36.26977878907645447, -21.93194718998534753, -20.87741241889870736 ) ) ;
#24695 = CARTESIAN_POINT ( 'NONE',  ( 16.48605814428184857, 11.34583003460130435, -14.75612992736757256 ) ) ;
#24696 = CARTESIAN_POINT ( 'NONE',  ( 29.49448338005720416, -10.05855281841770221, -18.88094824714235642 ) ) ;
#24697 = DIRECTION ( 'NONE',  ( -0.5877852522924731371, -1.586114251531760728E-16, -0.8090169943749474513 ) ) ;
#24698 = DIRECTION ( 'NONE',  ( -0.5877852522924731371, -1.586114251531760728E-16, -0.8090169943749474513 ) ) ;
#24699 = CARTESIAN_POINT ( 'NONE',  ( -0.6527133886630255288, 8.860760056385759142, -4.503039949738237624 ) ) ;
#24700 = ADVANCED_FACE ( 'NONE', ( #19081 ), #10064, .F. ) ;
#24701 = EDGE_CURVE ( 'NONE', #2206, #11734, #26116, .T. ) ;
#24702 = EDGE_CURVE ( 'NONE', #16032, #4875, #7042, .T. ) ;
#24703 = AXIS2_PLACEMENT_3D ( 'NONE', #10409, #15135, #24614 ) ;
#24704 = EDGE_LOOP ( 'NONE', ( #6066, #23621, #30061, #16273, #573 ) ) ;
#24705 = EDGE_CURVE ( 'NONE', #29509, #9780, #23362, .T. ) ;
#24706 = LINE ( 'NONE', #6233, #17204 ) ;
#24707 = LINE ( 'NONE', #12788, #22902 ) ;
#24708 = AXIS2_PLACEMENT_3D ( 'NONE', #2809, #14222, #25852 ) ;
#24709 = DIRECTION ( 'NONE',  ( -0.5877852522924731371, 0.000000000000000000, 0.8090169943749474513 ) ) ;
#24711 = CARTESIAN_POINT ( 'NONE',  ( 0.000000000000000000, 0.000000000000000000, -4.974599999999998801 ) ) ;
#24710 = VECTOR ( 'NONE', #16513, 1000.000000000000000 ) ;
#24712 = CARTESIAN_POINT ( 'NONE',  ( 13.17827647522021906, 8.595009676161804890, -15.86834059905992511 ) ) ;
#24713 = CARTESIAN_POINT ( 'NONE',  ( 35.54859390953724585, -21.18451583373416014, -18.19919658220850422 ) ) ;
#24714 = ORIENTED_EDGE ( 'NONE', *, *, #14740, .F. ) ;
#24715 = CARTESIAN_POINT ( 'NONE',  ( 9.112530393872706469, 16.18137232441842954, -17.05472470070859714 ) ) ;
#24716 = PRODUCT_DEFINITION_SHAPE ( 'NONE', 'NONE',  #6153 ) ;
#24717 = ORIENTED_EDGE ( 'NONE', *, *, #9581, .T. ) ;
#24718 = CARTESIAN_POINT ( 'NONE',  ( 28.47856004806874353, -11.16640101040803401, -12.66155532224275149 ) ) ;
#24719 = CARTESIAN_POINT ( 'NONE',  ( 10.35864918915110877, 16.97212501191939538, -17.94384837343789485 ) ) ;
#24720 = FACE_BOUND ( 'NONE', #27843, .T. ) ;
#24721 = EDGE_LOOP ( 'NONE', ( #26193, #7537, #7836, #10570, #11543 ) ) ;
#24722 = VERTEX_POINT ( 'NONE', #21214 ) ;
#24723 = CARTESIAN_POINT ( 'NONE',  ( 158.6922820468854241, -9.999999999999998224, -32.39392330124607611 ) ) ;
#24724 = AXIS2_PLACEMENT_3D ( 'NONE', #26763, #10092, #15271 ) ;
#24725 = CARTESIAN_POINT ( 'NONE',  ( 11.47257016429183452, 9.270685755423764718, -15.86103888016343255 ) ) ;
#24726 = PLANE ( 'NONE',  #26717 ) ;
#24727 = CARTESIAN_POINT ( 'NONE',  ( 156.1922820468854241, -10.00000000000000000, -30.91696583120936026 ) ) ;
#24728 = ORIENTED_EDGE ( 'NONE', *, *, #3856, .F. ) ;
#24729 = CARTESIAN_POINT ( 'NONE',  ( 13.34161425493533315, 8.667191563245470576, -15.73815750552000381 ) ) ;
#24730 = EDGE_LOOP ( 'NONE', ( #11849, #15113, #17278, #15567 ) ) ;
#24731 = CARTESIAN_POINT ( 'NONE',  ( 17.13759149762038803, 5.494404601539362609, -21.09448147619161418 ) ) ;
#24732 = CARTESIAN_POINT ( 'NONE',  ( 14.60232135752762517, 2.980368010496468933, -17.13315712471359475 ) ) ;
#24733 = DIRECTION ( 'NONE',  ( -0.8090169943749474513, -2.183098979609982436E-16, -0.5877852522924731371 ) ) ;
#24734 = ORIENTED_EDGE ( 'NONE', *, *, #308, .T. ) ;
#24735 = CARTESIAN_POINT ( 'NONE',  ( 36.53271160917758209, -22.11316507130252873, -18.90714217169671230 ) ) ;
#24736 = ORIENTED_EDGE ( 'NONE', *, *, #775, .F. ) ;
#24737 = CARTESIAN_POINT ( 'NONE',  ( 24.79644250101478065, -1.608028467720058918, -19.02763285027648976 ) ) ;
#24738 = EDGE_CURVE ( 'NONE', #9138, #2080, #28287, .T. ) ;
#24739 = ADVANCED_FACE ( 'NONE', ( #5652 ), #14636, .T. ) ;
#24740 = EDGE_CURVE ( 'NONE', #19636, #3882, #12654, .T. ) ;
#24741 = DIRECTION ( 'NONE',  ( 1.110223024625156540E-16, 2.995891024602366092E-32, 1.000000000000000000 ) ) ;
#24742 = EDGE_CURVE ( 'NONE', #19798, #20836, #12809, .T. ) ;
#24743 = FACE_OUTER_BOUND ( 'NONE', #28022, .T. ) ;
#24744 = AXIS2_PLACEMENT_3D ( 'NONE', #7483, #18929, #28284 ) ;
#24745 = ORIENTED_EDGE ( 'NONE', *, *, #11789, .F. ) ;
#24746 = CARTESIAN_POINT ( 'NONE',  ( 168.6922820468853104, -9.999999999999998224, -9.266330736598359152 ) ) ;
#24747 = CARTESIAN_POINT ( 'NONE',  ( 33.10952763335142635, -11.62914684427059697, -19.38687730282833499 ) ) ;
#24748 = CARTESIAN_POINT ( 'NONE',  ( 141.1922820468854525, -1.999999999999978462, -10.74328820663507678 ) ) ;
#24749 = VECTOR ( 'NONE', #5159, 1000.000000000000000 ) ;
#24750 = VERTEX_POINT ( 'NONE', #19221 ) ;
#24751 = PLANE ( 'NONE',  #8047 ) ;
#24752 = PRODUCT_DEFINITION_CONTEXT ( 'detailed design', #28058, 'design' ) ;
#24753 = CARTESIAN_POINT ( 'NONE',  ( 16.59405769476016701, 11.43796928512929867, -11.86713876492064124 ) ) ;
#24754 = CARTESIAN_POINT ( 'NONE',  ( 32.30218501430429967, -10.99871056796995816, -17.40035725849610060 ) ) ;
#24755 = DIRECTION ( 'NONE',  ( 0.3090169943749472292, 8.338696094057992503E-17, -0.9510565162951536422 ) ) ;
#24756 = VERTEX_POINT ( 'NONE', #23983 ) ;
#24757 = CARTESIAN_POINT ( 'NONE',  ( 142.0152310637606092, -10.00000000000000355, -24.27857615940569147 ) ) ;
#24758 = ORIENTED_EDGE ( 'NONE', *, *, #15787, .F. ) ;
#24759 = CARTESIAN_POINT ( 'NONE',  ( 10.66616952815763320, 9.056185211661334833, -16.41224021383828102 ) ) ;
#24760 = LINE ( 'NONE', #3846, #24409 ) ;
#24761 = CARTESIAN_POINT ( 'NONE',  ( 142.2287565553230309, -10.00000000000000533, -29.49038105676660138 ) ) ;
#24762 = ORIENTED_EDGE ( 'NONE', *, *, #18420, .F. ) ;
#24763 = CARTESIAN_POINT ( 'NONE',  ( 14.75361449413180637, 10.34920949090176201, -14.61276839131081218 ) ) ;
#24764 = CARTESIAN_POINT ( 'NONE',  ( 33.87301206822314725, -11.11198276574163302, -17.60644260715651299 ) ) ;
#24765 = CARTESIAN_POINT ( 'NONE',  ( 25.36810815240369621, -0.9165050883202133791, -18.11329069065276443 ) ) ;
#24766 = ORIENTED_EDGE ( 'NONE', *, *, #21864, .T. ) ;
#24767 = VERTEX_POINT ( 'NONE', #28577 ) ;
#24768 = AXIS2_PLACEMENT_3D ( 'NONE', #2618, #8592, #24949 ) ;
#24769 = CARTESIAN_POINT ( 'NONE',  ( 139.5152310637606092, -4.999999999999980460, -11.28819510263909542 ) ) ;
#24770 = PLANE ( 'NONE',  #6296 ) ;
#24771 = CARTESIAN_POINT ( 'NONE',  ( 134.7287565553230024, -1.999999999999980460, -7.839745962155602044 ) ) ;
#24772 = CARTESIAN_POINT ( 'NONE',  ( 24.51672896724849338, -10.45039314358892035, -14.45231470433035170 ) ) ;
#24773 = CIRCLE ( 'NONE', #26722, 8.000000000000005329 ) ;
#24774 = CARTESIAN_POINT ( 'NONE',  ( 21.18694592818775746, 3.276320881159561438, -13.81383015674761339 ) ) ;
#24775 = EDGE_CURVE ( 'NONE', #4875, #14798, #21973, .T. ) ;
#24777 = ORIENTED_EDGE ( 'NONE', *, *, #21004, .F. ) ;
#24776 = EDGE_CURVE ( 'NONE', #2878, #5097, #5800, .T. ) ;
#24778 = LINE ( 'NONE', #29091, #4003 ) ;
#24779 = DIRECTION ( 'NONE',  ( 0.5877852522924731371, 1.586114251531760728E-16, -0.8090169943749474513 ) ) ;
#24780 = LINE ( 'NONE', #13166, #6039 ) ;
#24781 = CARTESIAN_POINT ( 'NONE',  ( 161.1922820468853104, -10.00000000000000000, -4.936203717676158398 ) ) ;
#24782 = PLANE ( 'NONE',  #13092 ) ;
#24783 = FACE_OUTER_BOUND ( 'NONE', #4924, .T. ) ;
#24784 = VECTOR ( 'NONE', #12200, 1000.000000000000000 ) ;
#24785 = CARTESIAN_POINT ( 'NONE',  ( 11.40026617402801179, 8.559985368287675200, -17.14749594687102174 ) ) ;
#24786 = CARTESIAN_POINT ( 'NONE',  ( 12.39803340617553928, 8.535179507765855433, -15.21071672276548625 ) ) ;
#24787 = CARTESIAN_POINT ( 'NONE',  ( 148.6922820468854241, -1.999999999999977129, -15.07341522555727664 ) ) ;
#24788 = ORIENTED_EDGE ( 'NONE', *, *, #13925, .T. ) ;
#24789 = LINE ( 'NONE', #3880, #6641 ) ;
#24790 = CONICAL_SURFACE ( 'NONE', #7232, 4.513000000000000789, 0.2131563744996339549 ) ;
#24791 = CARTESIAN_POINT ( 'NONE',  ( 0.000000000000000000, 0.000000000000000000, -2.450000000000000178 ) ) ;
#24792 = VERTEX_POINT ( 'NONE', #10510 ) ;
#24793 = CARTESIAN_POINT ( 'NONE',  ( 9.641350810849047548, 17.66889113945805789, -17.91752729848689185 ) ) ;
#24794 = CARTESIAN_POINT ( 'NONE',  ( 0.000000000000000000, 0.000000000000000000, 1.699999999999996625 ) ) ;
#24795 = CARTESIAN_POINT ( 'NONE',  ( 174.5152310637604103, -9.999999999999994671, -13.05155085951651195 ) ) ;
#24796 = CARTESIAN_POINT ( 'NONE',  ( 24.14317479683219858, -6.286850201977149055, -18.60698471650063723 ) ) ;
#24797 = VECTOR ( 'NONE', #19344, 999.9999999999998863 ) ;
#24798 = ORIENTED_EDGE ( 'NONE', *, *, #2447, .T. ) ;
#24799 = PLANE ( 'NONE',  #24179 ) ;
#24800 = CARTESIAN_POINT ( 'NONE',  ( 11.05541531668977662, 17.68942339022145305, -17.93331994345748726 ) ) ;
#24801 = EDGE_CURVE ( 'NONE', #7028, #11745, #24122, .T. ) ;
#24802 = VECTOR ( 'NONE', #20665, 1000.000000000000000 ) ;
#24803 = LINE ( 'NONE', #5732, #13934 ) ;
#24804 = DIRECTION ( 'NONE',  ( 0.9510565162951536422, 0.000000000000000000, -0.3090169943749475623 ) ) ;
#24805 = ORIENTED_EDGE ( 'NONE', *, *, #12756, .F. ) ;
#24806 = ORIENTED_EDGE ( 'NONE', *, *, #22103, .F. ) ;
#24807 = CARTESIAN_POINT ( 'NONE',  ( 23.29338531092689735, -7.078548041224526521, -17.51562821661096336 ) ) ;
#24808 = CARTESIAN_POINT ( 'NONE',  ( 153.6922820468853672, -4.999999999999976019, -9.266330736598359152 ) ) ;
#24809 = CARTESIAN_POINT ( 'NONE',  ( 22.26732294003774015, -3.469656073077215463, -14.71322089325822624 ) ) ;
#24810 = ORIENTED_EDGE ( 'NONE', *, *, #16305, .F. ) ;
#24811 = DIRECTION ( 'NONE',  ( -0.5877852522924731371, -1.586114251531760235E-16, 0.8090169943749474513 ) ) ;
#24812 = CARTESIAN_POINT ( 'NONE',  ( 19.42071131597032974, 7.574497315622086724, -15.00200944635056644 ) ) ;
#24813 = CARTESIAN_POINT ( 'NONE',  ( 20.76230466941008146, -3.840972149463459218, -19.45223659164069474 ) ) ;
#24814 = EDGE_CURVE ( 'NONE', #6532, #25128, #26889, .T. ) ;
#24815 = ORIENTED_EDGE ( 'NONE', *, *, #8799, .F. ) ;
#24816 = CARTESIAN_POINT ( 'NONE',  ( 31.81434894052502571, -10.04473835610349575, -15.03854332269495764 ) ) ;
#24817 = AXIS2_PLACEMENT_3D ( 'NONE', #28949, #10728, #22177 ) ;
#24818 = LINE ( 'NONE', #5900, #21121 ) ;
#24819 = AXIS2_PLACEMENT_3D ( 'NONE', #10282, #26490, #5723 ) ;
#24820 = CLOSED_SHELL ( 'NONE', ( #135, #14018, #23596, #21003, #3242, #6191, #29121, #9331, #26187, #17244, #26509, #1628, #21554, #864, #14780, #28453 ) ) ;
#24821 = DIRECTION ( 'NONE',  ( -2.698458740408365879E-16, 1.000000000000000000, 0.000000000000000000 ) ) ;
#24822 = DIRECTION ( 'NONE',  ( 0.5877852522924731371, 1.586114251531760728E-16, 0.8090169943749474513 ) ) ;
#24823 = CARTESIAN_POINT ( 'NONE',  ( 87.72563772519548309, -4.999999999999993783, 63.73640660374597644 ) ) ;
#24824 = CARTESIAN_POINT ( 'NONE',  ( 6.938893903907228378E-15, 55.00000000000000711, -12.50000000000001066 ) ) ;
#24825 = CARTESIAN_POINT ( 'NONE',  ( 26.63310354640557520, -6.268104337495945977, -18.78393408973622769 ) ) ;
#24826 = CARTESIAN_POINT ( 'NONE',  ( 21.10828700581006601, 3.717818950362942854, -18.90958453460783417 ) ) ;
#24827 = CARTESIAN_POINT ( 'NONE',  ( 36.54859390954303677, -22.18451583373416014, -15.55638201429745848 ) ) ;
#24828 = DIRECTION ( 'NONE',  ( -0.5000000000000017764, -0.8660254037844377084, 0.000000000000000000 ) ) ;
#24829 = CARTESIAN_POINT ( 'NONE',  ( 12.49664108868010182, 8.569232744350554043, -15.13285098609708790 ) ) ;
#24830 = LINE ( 'NONE', #8924, #8809 ) ;
#24831 = DIRECTION ( 'NONE',  ( -0.8090169943749474513, -2.183098979609982436E-16, -0.5877852522924731371 ) ) ;
#24832 = CARTESIAN_POINT ( 'NONE',  ( 13.34161425493533315, 8.667191563245470576, -15.73815750552000381 ) ) ;
#24833 = CARTESIAN_POINT ( 'NONE',  ( 0.6527133886630124282, -8.860760056385789341, -4.503039949738222525 ) ) ;
#24834 = LINE ( 'NONE', #3925, #778 ) ;
#24835 = CARTESIAN_POINT ( 'NONE',  ( 11.47257016429183452, 9.270685755423764718, -15.86103888016343255 ) ) ;
#24836 = EDGE_CURVE ( 'NONE', #968, #12496, #29187, .T. ) ;
#24837 = ORIENTED_EDGE ( 'NONE', *, *, #2938, .T. ) ;
#24838 = CONICAL_SURFACE ( 'NONE', #11650, 5.999999999999977796, 0.7853981633974509435 ) ;
#24839 = CARTESIAN_POINT ( 'NONE',  ( 0.000000000000000000, 0.000000000000000000, 0.000000000000000000 ) ) ;
#24840 = LINE ( 'NONE', #23000, #14147 ) ;
#24841 = EDGE_CURVE ( 'NONE', #21691, #24463, #14459, .T. ) ;
#24842 = PLANE ( 'NONE',  #29834 ) ;
#24843 = B_SPLINE_CURVE_WITH_KNOTS ( 'NONE', 3,
 ( #13866, #23805, #2302, #2904 ),
 .UNSPECIFIED., .F., .F.,
 ( 4, 4 ),
 ( 2.380737581560122065E-07, 0.002336974151641542981 ),
 .UNSPECIFIED. ) ;
#24844 = CIRCLE ( 'NONE', #7294, 0.4999999999999986677 ) ;
#24845 = EDGE_LOOP ( 'NONE', ( #5781, #1568, #24237, #4847 ) ) ;
#24846 = CARTESIAN_POINT ( 'NONE',  ( 8.944617638130560877, 16.95144162614991501, -17.89908301402565982 ) ) ;
#24847 = CARTESIAN_POINT ( 'NONE',  ( 36.54859105337858693, -23.18450300252589003, -18.42496455282032386 ) ) ;
#24848 = ORIENTED_EDGE ( 'NONE', *, *, #15853, .F. ) ;
#24849 = CARTESIAN_POINT ( 'NONE',  ( 18.57953865233433532, 8.080199298666570940, -13.63460617990120838 ) ) ;
#24850 = CARTESIAN_POINT ( 'NONE',  ( 27.87518295380144551, -11.54787579004265652, -18.81772651352153858 ) ) ;
#24851 = PLANE ( 'NONE',  #17968 ) ;
#24852 = CARTESIAN_POINT ( 'NONE',  ( 163.6922820468853956, -9.999999999999998224, -35.24709285013155835 ) ) ;
#24853 = DIRECTION ( 'NONE',  ( 0.000000000000000000, -0.000000000000000000, 1.000000000000000000 ) ) ;
#24854 = CARTESIAN_POINT ( 'NONE',  ( 22.48601049859325585, 2.925819830077934558, -17.76611561182923893 ) ) ;
#24855 = ORIENTED_EDGE ( 'NONE', *, *, #8952, .F. ) ;
#24856 = LINE ( 'NONE', #1817, #4054 ) ;
#24857 = STYLED_ITEM ( 'NONE', ( #26166 ), #21 ) ;
#24858 = VECTOR ( 'NONE', #25053, 1000.000000000000000 ) ;
#24859 = ORIENTED_EDGE ( 'NONE', *, *, #28381, .F. ) ;
#24860 = CIRCLE ( 'NONE', #28796, 13.00000000000000178 ) ;
#24861 = CARTESIAN_POINT ( 'NONE',  ( 141.1922820468854525, -4.999999999999980460, -22.25671179336495697 ) ) ;
#24862 = CARTESIAN_POINT ( 'NONE',  ( 152.0152310637604955, -10.00000000000000178, -15.61832212156129351 ) ) ;
#24863 = VECTOR ( 'NONE', #28076, 1000.000000000000000 ) ;
#24864 = AXIS2_PLACEMENT_3D ( 'NONE', #28838, #12899, #7727 ) ;
#24865 = CARTESIAN_POINT ( 'NONE',  ( 12.84373479294319864, 8.511860559062048637, -16.13004233893675377 ) ) ;
#24866 = CARTESIAN_POINT ( 'NONE',  ( 35.54859390953724585, -21.18451583373416014, -17.22552805718784441 ) ) ;
#24867 = EDGE_LOOP ( 'NONE', ( #29346, #29547, #1145, #27608, #22119 ) ) ;
#24868 = CARTESIAN_POINT ( 'NONE',  ( 10.62817821613907476, 9.230418211344437296, -16.42795095778131298 ) ) ;
#24869 = ORIENTED_EDGE ( 'NONE', *, *, #17332, .F. ) ;
#24870 = CARTESIAN_POINT ( 'NONE',  ( 24.87127057246125972, -9.548149280147088191, -14.79180087847266556 ) ) ;
#24871 = CARTESIAN_POINT ( 'NONE',  ( 12.90243451339205194, 9.531139938431367753, -16.08819151157827321 ) ) ;
#24872 = CARTESIAN_POINT ( 'NONE',  ( 127.7287565553229598, -1.999999999999982681, -33.50000000000000000 ) ) ;
#24873 = ADVANCED_FACE ( 'NONE', ( #24421 ), #12497, .T. ) ;
#24874 = ORIENTED_EDGE ( 'NONE', *, *, #10380, .F. ) ;
#24875 = DIRECTION ( 'NONE',  ( -0.8090169943749474513, -2.183098979609982436E-16, 0.5877852522924731371 ) ) ;
#24876 = VERTEX_POINT ( 'NONE', #7631 ) ;
#24877 = ADVANCED_FACE ( 'NONE', ( #19525 ), #5954, .T. ) ;
#24878 = FACE_OUTER_BOUND ( 'NONE', #18714, .T. ) ;
#24879 = FACE_OUTER_BOUND ( 'NONE', #25435, .T. ) ;
#24880 = EDGE_CURVE ( 'NONE', #13256, #9641, #26268, .T. ) ;
#24881 = DIRECTION ( 'NONE',  ( 0.3090169943749475623, 8.338696094058001131E-17, 0.9510565162951536422 ) ) ;
#24882 = EDGE_LOOP ( 'NONE', ( #14593, #23228, #14132, #12242 ) ) ;
#24883 = AXIS2_PLACEMENT_3D ( 'NONE', #25822, #25665, #4753 ) ;
#24884 = CARTESIAN_POINT ( 'NONE',  ( 13.39606018151479461, 8.691252192278360766, -15.69476314099692971 ) ) ;
#24885 = AXIS2_PLACEMENT_3D ( 'NONE', #16771, #9432, #7019 ) ;
#24886 = CARTESIAN_POINT ( 'NONE',  ( 16.96299543436377633, 3.857017182823994084, -13.23919852190412527 ) ) ;
#24887 = CARTESIAN_POINT ( 'NONE',  ( 17.83966564144121136, 6.109271821037239647, -21.09843361817607388 ) ) ;
#24888 = ORIENTED_EDGE ( 'NONE', *, *, #27246, .T. ) ;
#24889 = VECTOR ( 'NONE', #11947, 1000.000000000000000 ) ;
#24890 = DIRECTION ( 'NONE',  ( 1.000000000000000000, 0.000000000000000000, 0.000000000000000000 ) ) ;
#24891 = CARTESIAN_POINT ( 'NONE',  ( 156.1922820468853388, -1.999999999999975353, -4.936203717676158398 ) ) ;
#24892 = CARTESIAN_POINT ( 'NONE',  ( 19.61192361542596529, -2.405681417800469291, -14.70675912396028906 ) ) ;
#24893 = ORIENTED_EDGE ( 'NONE', *, *, #23049, .T. ) ;
#24894 = CARTESIAN_POINT ( 'NONE',  ( 153.6922820468853388, -1.999999999999976241, -17.92658477444275533 ) ) ;
#24895 = AXIS2_PLACEMENT_3D ( 'NONE', #18252, #15808, #1954 ) ;
#24896 = FACE_OUTER_BOUND ( 'NONE', #22316, .T. ) ;
#24897 = VECTOR ( 'NONE', #16218, 1000.000000000000000 ) ;
#24898 = CARTESIAN_POINT ( 'NONE',  ( 136.1922820468854241, -10.00000000000000533, -10.74328820663507322 ) ) ;
#24899 = CARTESIAN_POINT ( 'NONE',  ( 34.82539348385352440, -18.93555941106099993, -20.13934242161363741 ) ) ;
#24900 = CARTESIAN_POINT ( 'NONE',  ( 173.6922820468852535, -4.999999999999969802, 2.247092850131519715 ) ) ;
#24901 = ORIENTED_EDGE ( 'NONE', *, *, #16238, .T. ) ;
#24902 = ORIENTED_EDGE ( 'NONE', *, *, #4737, .T. ) ;
#24903 = CARTESIAN_POINT ( 'NONE',  ( 162.2287565553229172, -1.999999999999972689, -12.16987298107780369 ) ) ;
#24904 = CARTESIAN_POINT ( 'NONE',  ( 12.24532799939971284, 9.516186676127107447, -15.33315318048745013 ) ) ;
#24905 = CARTESIAN_POINT ( 'NONE',  ( 35.54859390953724585, -23.18451583373416014, -17.99055332684694974 ) ) ;
#24906 = ORIENTED_EDGE ( 'NONE', *, *, #13482, .F. ) ;
#24907 = DIRECTION ( 'NONE',  ( -2.698458740408365879E-16, 1.000000000000000000, 0.000000000000000000 ) ) ;
#24908 = EDGE_CURVE ( 'NONE', #26572, #24722, #24574, .T. ) ;
#24909 = CARTESIAN_POINT ( 'NONE',  ( 11.28991474634619863, 7.910464746135025926, -16.02350989558273753 ) ) ;
#24910 = CARTESIAN_POINT ( 'NONE',  ( 163.6922820468853388, -9.999999999999998224, -15.07341522555727664 ) ) ;
#24911 = DIRECTION ( 'NONE',  ( -2.698458740408365879E-16, 1.000000000000000000, 0.000000000000000000 ) ) ;
#24912 = EDGE_CURVE ( 'NONE', #4960, #3275, #21662, .T. ) ;
#24913 = EDGE_CURVE ( 'NONE', #22429, #722, #28736, .T. ) ;
#24914 = ORIENTED_EDGE ( 'NONE', *, *, #20809, .T. ) ;
#24915 = CARTESIAN_POINT ( 'NONE',  ( 134.5152310637605808, -1.999999999999980460, -28.60870317832789311 ) ) ;
#24916 = ADVANCED_FACE ( 'NONE', ( #16937 ), #26417, .T. ) ;
#24917 = ORIENTED_EDGE ( 'NONE', *, *, #9965, .F. ) ;
#24918 = CARTESIAN_POINT ( 'NONE',  ( 10.35864918915110877, 16.97212501191939538, -17.91752729848689185 ) ) ;
#24919 = VECTOR ( 'NONE', #2393, 1000.000000000000000 ) ;
#24921 = VECTOR ( 'NONE', #11894, 1000.000000000000000 ) ;
#24920 = CARTESIAN_POINT ( 'NONE',  ( 34.41982446195410716, -12.62108234628556680, -19.94648786050102274 ) ) ;
#24922 = CARTESIAN_POINT ( 'NONE',  ( 23.86551563699305234, 2.542095107771292106, -17.79649620197707094 ) ) ;
#24923 = LINE ( 'NONE', #6593, #19390 ) ;
#24924 = LINE ( 'NONE', #6869, #20872 ) ;
#24925 = CARTESIAN_POINT ( 'NONE',  ( 144.7287565553230309, -4.999999999999978684, -33.82050807568879947 ) ) ;
#24926 = CARTESIAN_POINT ( 'NONE',  ( 0.000000000000000000, 0.000000000000000000, 0.000000000000000000 ) ) ;
#24927 =( GEOMETRIC_REPRESENTATION_CONTEXT ( 3 ) GLOBAL_UNCERTAINTY_ASSIGNED_CONTEXT ( ( #20485 ) ) GLOBAL_UNIT_ASSIGNED_CONTEXT ( ( #16538, #72, #11491 ) ) REPRESENTATION_CONTEXT ( 'NONE', 'WORKASPACE' ) );
#24928 = CARTESIAN_POINT ( 'NONE',  ( 29.30807694892355286, -8.357723062633453992, -13.20244061823602522 ) ) ;
#24929 = CARTESIAN_POINT ( 'NONE',  ( 23.94974919959990345, -8.117095362258064384, -14.41405346848900848 ) ) ;
#24930 = EDGE_LOOP ( 'NONE', ( #9745, #20147 ) ) ;
#24931 = DIRECTION ( 'NONE',  ( -1.000000000000000000, 0.000000000000000000, 0.000000000000000000 ) ) ;
#24932 = LINE ( 'NONE', #5325, #25789 ) ;
#24933 = FACE_OUTER_BOUND ( 'NONE', #402, .T. ) ;
#24934 = VECTOR ( 'NONE', #23584, 1000.000000000000000 ) ;
#24935 = ADVANCED_FACE ( 'NONE', ( #17382 ), #4114, .T. ) ;
#24936 = PLANE ( 'NONE',  #27682 ) ;
#24937 = CARTESIAN_POINT ( 'NONE',  ( 159.5152310637605240, -9.999999999999998224, -30.37205893520531319 ) ) ;
#24938 = VECTOR ( 'NONE', #15626, 1000.000000000000000 ) ;
#24939 = DIRECTION ( 'NONE',  ( 1.000000000000000000, 0.000000000000000000, 0.000000000000000000 ) ) ;
#24940 = CARTESIAN_POINT ( 'NONE',  ( 11.22387317355479475, 9.091340879052031809, -17.24161325043666082 ) ) ;
#24941 = CARTESIAN_POINT ( 'NONE',  ( 10.33811693838771717, 18.38618951776012267, -17.93331994345748726 ) ) ;
#24942 = LINE ( 'NONE', #29419, #6340 ) ;
#24943 = ORIENTED_EDGE ( 'NONE', *, *, #19776, .T. ) ;
#24944 = CARTESIAN_POINT ( 'NONE',  ( 12.82896712056928124, -5.000000000000014211, 39.48350090593866923 ) ) ;
#24945 = DIRECTION ( 'NONE',  ( -1.000000000000000000, 4.884981308350688778E-15, 0.000000000000000000 ) ) ;
#24946 = EDGE_LOOP ( 'NONE', ( #11119, #10215, #2852, #7864, #11583 ) ) ;
#24947 = CARTESIAN_POINT ( 'NONE',  ( 9.641350777746193756, 17.66889129127197577, -17.91630266473768884 ) ) ;
#24948 = EDGE_CURVE ( 'NONE', #19824, #28625, #1714, .T. ) ;
#24949 = DIRECTION ( 'NONE',  ( -2.698458740408365879E-16, 1.000000000000000000, 0.000000000000000000 ) ) ;
#24950 = CARTESIAN_POINT ( 'NONE',  ( 171.1922820468853672, -9.999999999999994671, -30.91696583120936026 ) ) ;
#24951 = PLANE ( 'NONE',  #23016 ) ;
#24952 = EDGE_CURVE ( 'NONE', #6495, #26976, #27501, .T. ) ;
#24954 = ORIENTED_EDGE ( 'NONE', *, *, #16896, .F. ) ;
#24953 = CARTESIAN_POINT ( 'NONE',  ( 25.21413058671614849, -1.115224416820481457, -18.44856734933592080 ) ) ;
#24955 = VERTEX_POINT ( 'NONE', #20128 ) ;
#24956 = CARTESIAN_POINT ( 'NONE',  ( 176.1922820468853388, -1.999999999999969580, -28.06379628232387802 ) ) ;
#24957 = EDGE_CURVE ( 'NONE', #28570, #2318, #6099, .T. ) ;
#24958 = CARTESIAN_POINT ( 'NONE',  ( 12.25364105430271700, 9.519861518574414205, -15.32652744092241726 ) ) ;
#24959 = CARTESIAN_POINT ( 'NONE',  ( 33.14486676600987636, -11.77651092997264293, -17.78036478212233717 ) ) ;
#24960 = DIRECTION ( 'NONE',  ( 0.9510565162951536422, 0.000000000000000000, -0.3090169943749475623 ) ) ;
#24961 = CARTESIAN_POINT ( 'NONE',  ( 28.15048769591263067, -5.842385520647848551, -16.89978903947823241 ) ) ;
#24962 = CARTESIAN_POINT ( 'NONE',  ( 8.000000000000008882, 3.871967595402145967, -4.501061386767531758 ) ) ;
#24963 = CARTESIAN_POINT ( 'NONE',  ( 24.04487210496366245, -0.6674514567044148583, -16.01806975046538284 ) ) ;
#24964 = ORIENTED_EDGE ( 'NONE', *, *, #3406, .T. ) ;
#24965 = DIRECTION ( 'NONE',  ( 0.000000000000000000, 0.000000000000000000, 1.000000000000000000 ) ) ;
#24966 = ORIENTED_EDGE ( 'NONE', *, *, #15085, .T. ) ;
#24967 = ORIENTED_EDGE ( 'NONE', *, *, #23419, .F. ) ;
#24968 = SURFACE_STYLE_FILL_AREA ( #22969 ) ;
#24969 = CARTESIAN_POINT ( 'NONE',  ( 13.93491968177131923, 5.624373287173536795, -18.66784319378200863 ) ) ;
#24970 = CARTESIAN_POINT ( 'NONE',  ( 29.99716341122577745, -11.34936846952144585, -14.08097903537201212 ) ) ;
#24971 = ORIENTED_EDGE ( 'NONE', *, *, #9024, .F. ) ;
#24972 = CARTESIAN_POINT ( 'NONE',  ( 26.57062215293289498, -11.41726559881178638, -18.09730928560479057 ) ) ;
#24973 = PRODUCT_DEFINITION_SHAPE ( 'NONE', 'NONE',  #11917 ) ;
#24974 = AXIS2_PLACEMENT_3D ( 'NONE', #24472, #984, #20032 ) ;
#24975 = CARTESIAN_POINT ( 'NONE',  ( 168.6922820468853672, -1.999999999999970912, -26.58683881228715862 ) ) ;
#24976 = CARTESIAN_POINT ( 'NONE',  ( 137.0152310637605808, -4.999999999999980460, -17.38167787843870826 ) ) ;
#24977 = DIRECTION ( 'NONE',  ( -0.9510565162951536422, 0.000000000000000000, -0.3090169943749472292 ) ) ;
#24978 = CARTESIAN_POINT ( 'NONE',  ( 420.0000000000002274, 27.64101615137744972, 12.00000000000000178 ) ) ;
#24979 = AXIS2_PLACEMENT_3D ( 'NONE', #11870, #14604, #5167 ) ;
#24980 = FACE_OUTER_BOUND ( 'NONE', #27475, .T. ) ;
#24981 = CARTESIAN_POINT ( 'NONE',  ( 27.63487812444411418, -5.020849242181972372, -17.14317672846274831 ) ) ;
#24982 = CARTESIAN_POINT ( 'NONE',  ( 16.29141254853644227, 2.771581735061156682, -15.76764191790683611 ) ) ;
#24984 = ORIENTED_EDGE ( 'NONE', *, *, #2349, .F. ) ;
#24983 = CARTESIAN_POINT ( 'NONE',  ( 34.30083361619418980, -13.08651950748960680, -20.95284133056243192 ) ) ;
#24985 = DIRECTION ( 'NONE',  ( -0.5877852522924731371, -1.586114251531760235E-16, 0.8090169943749474513 ) ) ;
#24986 = CARTESIAN_POINT ( 'NONE',  ( 11.97192087863669663, 8.579774655713777065, -15.53257280409644991 ) ) ;
#24987 = DIRECTION ( 'NONE',  ( -2.698458740408365879E-16, 1.000000000000000000, 0.000000000000000000 ) ) ;
#24988 = CARTESIAN_POINT ( 'NONE',  ( 102.1495906963740623, -4.999999999999989342, -74.21602185925650019 ) ) ;
#24989 = CARTESIAN_POINT ( 'NONE',  ( 9.661883066202028303, 16.25482661256886630, -17.91573536996246929 ) ) ;
#24990 = DIRECTION ( 'NONE',  ( -2.698458740408365879E-16, 1.000000000000000000, 0.000000000000000000 ) ) ;
#24991 = CARTESIAN_POINT ( 'NONE',  ( 0.000000000000000000, 0.000000000000000000, 4.999999999999997335 ) ) ;
#24992 = ADVANCED_FACE ( 'NONE', ( #3968 ), #9098, .T. ) ;
#24993 = CARTESIAN_POINT ( 'NONE',  ( 12.49664108868010182, 8.569232744350554043, -15.13285098609708790 ) ) ;
#24994 = ORIENTED_EDGE ( 'NONE', *, *, #28524, .T. ) ;
#24995 = DIRECTION ( 'NONE',  ( 0.9510565162951536422, 2.566386769018988816E-16, 0.3090169943749472292 ) ) ;
#24996 = CARTESIAN_POINT ( 'NONE',  ( 129.5152310637605524, -1.999999999999982236, -21.71180489736090991 ) ) ;
#24997 = LINE ( 'NONE', #1650, #24405 ) ;
#24998 = ORIENTED_EDGE ( 'NONE', *, *, #29487, .T. ) ;
#24999 = ORIENTED_EDGE ( 'NONE', *, *, #22323, .T. ) ;
#25000 = CARTESIAN_POINT ( 'NONE',  ( 13.39286676965551059, 7.631811206235384226, -15.69730834661896424 ) ) ;
#25001 = CARTESIAN_POINT ( 'NONE',  ( 36.19022241692326247, -21.57454255207833071, -21.10101832753974449 ) ) ;
#25002 = CARTESIAN_POINT ( 'NONE',  ( 18.25722813608836859, -0.08152059447761372812, -18.39925177747023710 ) ) ;
#25003 = CARTESIAN_POINT ( 'NONE',  ( 19.09420370221858931, 5.586061004495046056, -18.95245686415860220 ) ) ;
#25004 = CARTESIAN_POINT ( 'NONE',  ( -19.99999999999999645, 60.00000000000000711, -30.00000000000000711 ) ) ;
#25005 = AXIS2_PLACEMENT_3D ( 'NONE', #17145, #19129, #5096 ) ;
#25006 = CARTESIAN_POINT ( 'NONE',  ( 136.1922820468854241, -4.999999999999980460, -28.06379628232387446 ) ) ;
#25007 = CARTESIAN_POINT ( 'NONE',  ( 24.91205307904067112, 1.131441846345163427, -15.76301496618838627 ) ) ;
#25008 = ORIENTED_EDGE ( 'NONE', *, *, #3278, .T. ) ;
#25009 = CYLINDRICAL_SURFACE ( 'NONE', #2603, 2.000000000000000000 ) ;
#25010 = ADVANCED_FACE ( 'NONE', ( #10965 ), #29661, .T. ) ;
#25011 = FACE_OUTER_BOUND ( 'NONE', #8100, .T. ) ;
#25012 = CARTESIAN_POINT ( 'NONE',  ( 156.1922820468853956, -10.00000000000000000, -19.40354224447947828 ) ) ;
#25013 = CARTESIAN_POINT ( 'NONE',  ( 174.5152310637604103, -1.999999999999970024, -2.627941064794695691 ) ) ;
#25014 = CARTESIAN_POINT ( 'NONE',  ( 33.85795792134603488, -11.10969635406632072, -17.56389463281766439 ) ) ;
#25015 = VERTEX_POINT ( 'NONE', #1992 ) ;
#25016 = CARTESIAN_POINT ( 'NONE',  ( 10.60386377644718614, 9.341927331141327784, -16.43800583390468262 ) ) ;
#25017 = ORIENTED_EDGE ( 'NONE', *, *, #19612, .T. ) ;
#25018 = VECTOR ( 'NONE', #13827, 1000.000000000000000 ) ;
#25019 = CARTESIAN_POINT ( 'NONE',  ( 30.24922550192677306, -10.40856591028444278, -13.02298783260255988 ) ) ;
#25020 = CARTESIAN_POINT ( 'NONE',  ( 143.6922820468854525, -4.999999999999978684, -23.73366926340167282 ) ) ;
#25021 = CARTESIAN_POINT ( 'NONE',  ( 12.87521155010636242, 9.519109623917222152, -16.10988869383489686 ) ) ;
#25022 = CARTESIAN_POINT ( 'NONE',  ( 172.7287565553229456, -4.999999999999971578, 0.5000000000000029976 ) ) ;
#25023 = VERTEX_POINT ( 'NONE', #15843 ) ;
#25024 = ORIENTED_EDGE ( 'NONE', *, *, #5815, .T. ) ;
#25025 = CARTESIAN_POINT ( 'NONE',  ( 159.5152310637604955, -4.999999999999974243, -1.770974823053889042E-14 ) ) ;
#25026 = CARTESIAN_POINT ( 'NONE',  ( 12.77278825050581013, 8.691252192278360766, -14.91275796197543890 ) ) ;
#25027 = CARTESIAN_POINT ( 'NONE',  ( 157.0152310637604955, -4.999999999999975131, -17.38167787843871182 ) ) ;
#25028 = ORIENTED_EDGE ( 'NONE', *, *, #19173, .F. ) ;
#25029 = CARTESIAN_POINT ( 'NONE',  ( 167.2287565553229456, -4.999999999999972466, -12.16987298107780013 ) ) ;
#25030 = ORIENTED_EDGE ( 'NONE', *, *, #23379, .F. ) ;
#25031 = CARTESIAN_POINT ( 'NONE',  ( 9.661883061612440926, 16.25482663361732705, -17.91752729848688830 ) ) ;
#25032 = CARTESIAN_POINT ( 'NONE',  ( 22.87531825017061848, 1.851759407679815173, -13.77476424085121742 ) ) ;
#25033 = CARTESIAN_POINT ( 'NONE',  ( 18.23272808550097679, 0.7689261898593379163, -20.18852386690180367 ) ) ;
#25034 = ORIENTED_EDGE ( 'NONE', *, *, #25610, .T. ) ;
#25035 = CARTESIAN_POINT ( 'NONE',  ( 31.84774147790582433, -10.54213090804960018, -15.00000000011102763 ) ) ;
#25036 = CARTESIAN_POINT ( 'NONE',  ( -4.000000000000020428, -6.928203230275511437, 0.000000000000000000 ) ) ;
#25037 = CARTESIAN_POINT ( 'NONE',  ( 19.38992137333195842, 2.881095379261479739, -20.30776781288435373 ) ) ;
#25038 = VECTOR ( 'NONE', #20661, 1000.000000000000000 ) ;
#25039 = DIRECTION ( 'NONE',  ( -0.8090169943749474513, -2.183098979609982436E-16, -0.5877852522924731371 ) ) ;
#25040 = EDGE_CURVE ( 'NONE', #357, #18885, #15996, .T. ) ;
#25041 = CARTESIAN_POINT ( 'NONE',  ( 2.500000000000000444, 2.357898499370430834, -3.469446951953614189E-15 ) ) ;
#25042 = ADVANCED_FACE ( 'NONE', ( #15548 ), #10673, .T. ) ;
#25043 = EDGE_CURVE ( 'NONE', #27247, #3985, #1684, .T. ) ;
#25044 = EDGE_CURVE ( 'NONE', #22963, #25794, #22433, .T. ) ;
#25045 = ORIENTED_EDGE ( 'NONE', *, *, #20809, .F. ) ;
#25046 = CARTESIAN_POINT ( 'NONE',  ( 10.46960557229346733, 16.46326489517938541, -17.33590790293451178 ) ) ;
#25047 = CARTESIAN_POINT ( 'NONE',  ( 33.17819505895439391, -11.78846528140086924, -19.49437495119144259 ) ) ;
#25048 = CARTESIAN_POINT ( 'NONE',  ( 154.5152310637604955, -1.999999999999974909, -13.05155085951651195 ) ) ;
#25049 = VERTEX_POINT ( 'NONE', #1536 ) ;
#25050 = DIRECTION ( 'NONE',  ( 0.5877852522924731371, 1.586114251531760728E-16, 0.8090169943749474513 ) ) ;
#25051 = CARTESIAN_POINT ( 'NONE',  ( 30.71753525214919378, -10.10955902127019179, -14.92479911117869484 ) ) ;
#25052 = CARTESIAN_POINT ( 'NONE',  ( 12.24503583471362234, 9.516058715885376884, -15.33338595299508889 ) ) ;
#25053 = DIRECTION ( 'NONE',  ( 1.110223024625156540E-16, 2.995891024602366092E-32, 1.000000000000000000 ) ) ;
#25054 = ORIENTED_EDGE ( 'NONE', *, *, #11481, .F. ) ;
#25055 = LINE ( 'NONE', #22466, #8838 ) ;
#25056 = CIRCLE ( 'NONE', #15780, 13.00000000000000178 ) ;
#25057 = CARTESIAN_POINT ( 'NONE',  ( 12.77299770905688803, 7.633314995549595139, -14.91259101981587420 ) ) ;
#25058 = FACE_OUTER_BOUND ( 'NONE', #23884, .T. ) ;
#25059 = CARTESIAN_POINT ( 'NONE',  ( 4.000000000000019540, 6.928203230275512325, -5.000000000000000888 ) ) ;
#25060 = ORIENTED_EDGE ( 'NONE', *, *, #28880, .T. ) ;
#25061 = CARTESIAN_POINT ( 'NONE',  ( 10.35864917552468611, 16.97212507441191320, -17.91611982430173455 ) ) ;
#25062 = CARTESIAN_POINT ( 'NONE',  ( 33.68917633736438688, -10.64779379647620949, -18.96437360758372748 ) ) ;
#25063 = CARTESIAN_POINT ( 'NONE',  ( 24.00918528248616468, -0.5066965781341161712, -13.81223085940890627 ) ) ;
#25064 = DIRECTION ( 'NONE',  ( 1.000000000000000000, 0.000000000000000000, 0.000000000000000000 ) ) ;
#25065 = LINE ( 'NONE', #23080, #28911 ) ;
#25066 =( LENGTH_UNIT ( ) NAMED_UNIT ( * ) SI_UNIT ( .MILLI., .METRE. ) );
#25067 = CARTESIAN_POINT ( 'NONE',  ( 27.85014272824177795, -5.137623357037004013, -13.74226875356335320 ) ) ;
#25068 = CARTESIAN_POINT ( 'NONE',  ( 24.68698569862014480, -7.792836496385216805, -13.74806253080685359 ) ) ;
#25069 = EDGE_CURVE ( 'NONE', #17347, #14415, #11537, .T. ) ;
#25070 = ORIENTED_EDGE ( 'NONE', *, *, #892, .T. ) ;
#25071 = LINE ( 'NONE', #6456, #16194 ) ;
#25072 = EDGE_CURVE ( 'NONE', #11670, #29672, #20427, .T. ) ;
#25073 = EDGE_CURVE ( 'NONE', #25256, #25636, #15700, .T. ) ;
#25074 = LINE ( 'NONE', #8434, #15936 ) ;
#25075 = DIRECTION ( 'NONE',  ( 0.5877852522924731371, 1.586114251531760728E-16, -0.8090169943749474513 ) ) ;
#25076 = DIRECTION ( 'NONE',  ( -1.000000000000000000, 0.000000000000000000, 0.000000000000000000 ) ) ;
#25077 = CARTESIAN_POINT ( 'NONE',  ( 11.14294825671155209, 9.462472856991839265, -17.27507855072861176 ) ) ;
#25078 = VECTOR ( 'NONE', #18503, 1000.000000000000000 ) ;
#25079 = CARTESIAN_POINT ( 'NONE',  ( 12.50098444160134470, 8.571137227758441668, -15.12939039523150520 ) ) ;
#25080 = LINE ( 'NONE', #8883, #5358 ) ;
#25081 = VERTEX_POINT ( 'NONE', #8968 ) ;
#25082 = LINE ( 'NONE', #4170, #18346 ) ;
#25083 = ORIENTED_EDGE ( 'NONE', *, *, #8829, .F. ) ;
#25084 = CARTESIAN_POINT ( 'NONE',  ( 9.641352920869014298, 17.66888146263751125, -17.91030124961049097 ) ) ;
#25085 = CARTESIAN_POINT ( 'NONE',  ( 142.0152310637605524, -4.999999999999979572, -1.576685793744487278E-14 ) ) ;
#25086 = CARTESIAN_POINT ( 'NONE',  ( 30.81871029749655477, -11.10956723898439868, -14.94490981684777431 ) ) ;
#25087 = FACE_OUTER_BOUND ( 'NONE', #18141, .T. ) ;
#25088 = CARTESIAN_POINT ( 'NONE',  ( 129.5152310637605524, -1.999999999999982236, -13.05155085951650840 ) ) ;
#25090 = VERTEX_POINT ( 'NONE', #25029 ) ;
#25089 = CARTESIAN_POINT ( 'NONE',  ( 24.92864811393110358, -0.2441600445015326137, -14.78813717129899885 ) ) ;
#25091 = ORIENTED_EDGE ( 'NONE', *, *, #10771, .T. ) ;
#25092 = CARTESIAN_POINT ( 'NONE',  ( 4.000000000000000000, -1.933795701539638534, -2.201162342337696476 ) ) ;
#25093 = CARTESIAN_POINT ( 'NONE',  ( 12.24591402697972775, 9.516428332920080280, -15.33268742708093235 ) ) ;
#25094 = EDGE_LOOP ( 'NONE', ( #16929, #23262, #25739, #13428, #13805 ) ) ;
#25095 = CARTESIAN_POINT ( 'NONE',  ( 35.18065281855160720, -20.53155141575438591, -20.22037173032050461 ) ) ;
#25096 = PLANE ( 'NONE',  #3976 ) ;
#25097 = CARTESIAN_POINT ( 'NONE',  ( 25.71553203045151292, -8.406338935355361031, -18.42709291467145150 ) ) ;
#25098 = AXIS2_PLACEMENT_3D ( 'NONE', #28642, #14546, #5257 ) ;
#25099 = CARTESIAN_POINT ( 'NONE',  ( 8.000000000000012434, 0.7809653281576151018, -4.999999999999993783 ) ) ;
#25100 = CARTESIAN_POINT ( 'NONE',  ( 20.63450008290067927, -1.653576198284400833, -18.07233451455898532 ) ) ;
#25101 = ORIENTED_EDGE ( 'NONE', *, *, #29173, .F. ) ;
#25102 = CARTESIAN_POINT ( 'NONE',  ( 166.1922820468853672, -1.999999999999970912, -28.06379628232387802 ) ) ;
#25103 = CARTESIAN_POINT ( 'NONE',  ( 26.89114594638229505, -13.18314149429672000, -12.91981678032827041 ) ) ;
#25104 = CARTESIAN_POINT ( 'NONE',  ( 25.09247252535503492, -10.89683230441130135, -15.98339435310939827 ) ) ;
#25105 = EDGE_LOOP ( 'NONE', ( #3962, #13778, #28605, #15959 ) ) ;
#25106 = EDGE_LOOP ( 'NONE', ( #13737, #4257, #20499, #26075, #29662 ) ) ;
#25107 = CARTESIAN_POINT ( 'NONE',  ( 157.2287565553229456, -1.999999999999974021, -12.16987298107780369 ) ) ;
#25108 = ADVANCED_FACE ( 'NONE', ( #8826 ), #18284, .T. ) ;
#25109 = ADVANCED_FACE ( 'NONE', ( #12957 ), #22272, .T. ) ;
#25110 = EDGE_CURVE ( 'NONE', #19118, #8559, #2587, .T. ) ;
#25111 = PLANE ( 'NONE',  #29972 ) ;
#25113 = VERTEX_POINT ( 'NONE', #11862 ) ;
#25112 = EDGE_CURVE ( 'NONE', #13066, #19416, #11413, .T. ) ;
#25114 = CARTESIAN_POINT ( 'NONE',  ( 0.000000000000000000, 0.000000000000000000, 9.480888224575629408 ) ) ;
#25115 = CARTESIAN_POINT ( 'NONE',  ( 169.7287565553229172, -1.999999999999970468, -16.50000000000000355 ) ) ;
#25116 = LINE ( 'NONE', #13054, #20178 ) ;
#25117 = AXIS2_PLACEMENT_3D ( 'NONE', #1560, #22606, #7951 ) ;
#25118 = CARTESIAN_POINT ( 'NONE',  ( 9.641350810849047548, 17.66889113945805789, -23.00000000000000711 ) ) ;
#25119 = CARTESIAN_POINT ( 'NONE',  ( 25.82086518536678454, -3.233603117969178875, -16.21460360555060021 ) ) ;
#25120 = CARTESIAN_POINT ( 'NONE',  ( 19.36978511310259421, 2.022953856625822944, -19.43459320487130171 ) ) ;
#25121 = CARTESIAN_POINT ( 'NONE',  ( 32.62421882425100961, -9.622687980317111922, -18.08031881573170097 ) ) ;
#25122 = CARTESIAN_POINT ( 'NONE',  ( 148.6922820468854241, -1.999999999999976241, -15.07341522555727664 ) ) ;
#25123 = CARTESIAN_POINT ( 'NONE',  ( 12.50076791318051761, 8.571041463825640250, -15.12956297801270900 ) ) ;
#25124 = CARTESIAN_POINT ( 'NONE',  ( 132.0152310637605808, -1.999999999999981348, -32.93883019725009120 ) ) ;
#25125 = CARTESIAN_POINT ( 'NONE',  ( 2.500000000000000444, -1.768423874527823347, -1.020999999999997687 ) ) ;
#25126 = CARTESIAN_POINT ( 'NONE',  ( 9.678003265275730627, 16.18089732476941833, -17.88088483716984811 ) ) ;
#25128 = VERTEX_POINT ( 'NONE', #25603 ) ;
#25127 = CARTESIAN_POINT ( 'NONE',  ( 147.0152310637604955, -4.999999999999977796, -1.632196944975744474E-14 ) ) ;
#25129 = ORIENTED_EDGE ( 'NONE', *, *, #4198, .F. ) ;
#25130 = CARTESIAN_POINT ( 'NONE',  ( -31.74999999999995737, 0.000000000000000000, 0.000000000000000000 ) ) ;
#25131 = CARTESIAN_POINT ( 'NONE',  ( 10.33811693838771717, 18.38618951776012267, -19.66666666666843000 ) ) ;
#25132 = VERTEX_POINT ( 'NONE', #2729 ) ;
#25133 = CARTESIAN_POINT ( 'NONE',  ( 167.0152310637604955, -1.999999999999971356, -15.61832212156129707 ) ) ;
#25134 = CARTESIAN_POINT ( 'NONE',  ( 4.794903815660978452, -5.000000000000016875, 14.75719653579859347 ) ) ;
#25135 = FACE_OUTER_BOUND ( 'NONE', #30253, .T. ) ;
#25136 = VERTEX_POINT ( 'NONE', #9569 ) ;
#25137 = CARTESIAN_POINT ( 'NONE',  ( 8.944584683310379702, 16.95159276115599667, -19.66666666666843000 ) ) ;
#25138 = CARTESIAN_POINT ( 'NONE',  ( 35.54859390953724585, -23.18451583373416014, -17.78191007148576119 ) ) ;
#25139 = CARTESIAN_POINT ( 'NONE',  ( 19.82966512453777952, 6.730073478465656400, -20.48479553209826065 ) ) ;
#25140 = VECTOR ( 'NONE', #27068, 1000.000000000000000 ) ;
#25141 = CARTESIAN_POINT ( 'NONE',  ( 31.37220973900873489, -11.08107799475175348, -13.94606079199652982 ) ) ;
#25142 = AXIS2_PLACEMENT_3D ( 'NONE', #15653, #13216, #22838 ) ;
#25143 = DIRECTION ( 'NONE',  ( -2.698458740408365879E-16, 1.000000000000000000, 0.000000000000000000 ) ) ;
#25144 = CARTESIAN_POINT ( 'NONE',  ( 20.16317987096495656, -0.6177526724804084379, -13.65447574297484223 ) ) ;
#25145 = ORIENTED_EDGE ( 'NONE', *, *, #28365, .F. ) ;
#25146 = EDGE_CURVE ( 'NONE', #12292, #19109, #9113, .T. ) ;
#25147 = LINE ( 'NONE', #10802, #5517 ) ;
#25148 = EDGE_CURVE ( 'NONE', #2706, #10096, #22763, .T. ) ;
#25149 = VECTOR ( 'NONE', #18240, 1000.000000000000000 ) ;
#25151 = EDGE_LOOP ( 'NONE', ( #982, #8223, #8751, #25709 ) ) ;
#25150 =( LENGTH_UNIT ( ) NAMED_UNIT ( * ) SI_UNIT ( .MILLI., .METRE. ) );
#25152 = DIRECTION ( 'NONE',  ( -2.698458740408365879E-16, 1.000000000000000000, 0.000000000000000000 ) ) ;
#25153 = CARTESIAN_POINT ( 'NONE',  ( 172.7287565553229456, -4.999999999999970690, -33.50000000000000000 ) ) ;
#25154 = VECTOR ( 'NONE', #18887, 1000.000000000000000 ) ;
#25155 = DIRECTION ( 'NONE',  ( -1.000000000000000000, 0.000000000000000000, 0.000000000000000000 ) ) ;
#25156 = CARTESIAN_POINT ( 'NONE',  ( 35.54686456755326418, -21.17674681625933530, -18.46270299499373735 ) ) ;
#25157 = ORIENTED_EDGE ( 'NONE', *, *, #14363, .T. ) ;
#25158 = VECTOR ( 'NONE', #17459, 1000.000000000000000 ) ;
#25159 = CARTESIAN_POINT ( 'NONE',  ( 12.22241433628510165, 7.513235304754858568, -15.34201686955167609 ) ) ;
#25160 = ORIENTED_EDGE ( 'NONE', *, *, #27732, .F. ) ;
#25161 = AXIS2_PLACEMENT_3D ( 'NONE', #7651, #16955, #8840 ) ;
#25162 = CARTESIAN_POINT ( 'NONE',  ( 138.6922820468854525, -10.00000000000000533, -32.39392330124607611 ) ) ;
#25163 = PLANE ( 'NONE',  #13333 ) ;
#25164 = CARTESIAN_POINT ( 'NONE',  ( 11.86602117609799301, 10.05912493454434120, -16.75833615892761586 ) ) ;
#25165 = DIRECTION ( 'NONE',  ( 0.9510565162951536422, 0.000000000000000000, -0.3090169943749475623 ) ) ;
#25166 = VERTEX_POINT ( 'NONE', #25771 ) ;
#25167 = CONICAL_SURFACE ( 'NONE', #11986, 8.000000000000007105, 1.047197551196596077 ) ;
#25168 = VERTEX_POINT ( 'NONE', #9266 ) ;
#25169 = LINE ( 'NONE', #6702, #23183 ) ;
#25170 = DIRECTION ( 'NONE',  ( -2.698458740408365879E-16, 1.000000000000000000, 0.000000000000000000 ) ) ;
#25172 = ORIENTED_EDGE ( 'NONE', *, *, #14950, .F. ) ;
#25171 = CARTESIAN_POINT ( 'NONE',  ( 25.00000000000001066, 60.00000000000000711, 29.99999999999998579 ) ) ;
#25173 = DIRECTION ( 'NONE',  ( 0.3090169943749472292, 8.338696094057992503E-17, -0.9510565162951536422 ) ) ;
#25174 = EDGE_LOOP ( 'NONE', ( #1133, #9812, #26453, #3844, #9723 ) ) ;
#25175 = CARTESIAN_POINT ( 'NONE',  ( 13.15785925275590529, 8.585986940276173485, -15.88461348575242305 ) ) ;
#25176 = EDGE_CURVE ( 'NONE', #22060, #20312, #28088, .T. ) ;
#25177 = CARTESIAN_POINT ( 'NONE',  ( 20.53425600248055005, 0.8933117467920750343, -13.02782074225586406 ) ) ;
#25178 = CARTESIAN_POINT ( 'NONE',  ( 21.76882177598054113, -1.089445278190608102, -19.78435629462099854 ) ) ;
#25179 = CARTESIAN_POINT ( 'NONE',  ( 18.72775033408030154, 1.433941090885695768, -19.03071139844121262 ) ) ;
#25180 = VECTOR ( 'NONE', #15311, 1000.000000000000000 ) ;
#25181 = CARTESIAN_POINT ( 'NONE',  ( 20.00000000000001066, 55.00000000000000711, 24.99999999999998579 ) ) ;
#25182 = EDGE_LOOP ( 'NONE', ( #9567, #16187, #27331, #22579 ) ) ;
#25183 = CARTESIAN_POINT ( 'NONE',  ( 0.000000000000000000, 0.000000000000000000, 23.00000000000000000 ) ) ;
#25184 = AXIS2_PLACEMENT_3D ( 'NONE', #13146, #6739, #16031 ) ;
#25185 = CARTESIAN_POINT ( 'NONE',  ( 22.86252235622482587, -0.9498377794471745128, -13.29674124224850118 ) ) ;
#25186 = ORIENTED_EDGE ( 'NONE', *, *, #7535, .F. ) ;
#25187 = PLANE ( 'NONE',  #11025 ) ;
#25188 = CARTESIAN_POINT ( 'NONE',  ( 176.1922820468852819, -1.999999999999969580, -13.59645775552055902 ) ) ;
#25189 = VERTEX_POINT ( 'NONE', #12013 ) ;
#25190 = CARTESIAN_POINT ( 'NONE',  ( 126.3258676456270564, -4.999999999999984013, -91.78111523172451314 ) ) ;
#25191 = CARTESIAN_POINT ( 'NONE',  ( 161.1922820468853672, -1.999999999999972689, -19.40354224447947828 ) ) ;
#25192 = CARTESIAN_POINT ( 'NONE',  ( 168.6922820468853956, -1.999999999999970468, -35.24709285013155835 ) ) ;
#25193 = ORIENTED_EDGE ( 'NONE', *, *, #8692, .F. ) ;
#25194 = ORIENTED_EDGE ( 'NONE', *, *, #4909, .T. ) ;
#25195 = CARTESIAN_POINT ( 'NONE',  ( 137.2287565553230309, -4.999999999999981348, -3.509618943233400401 ) ) ;
#25196 = AXIS2_PLACEMENT_3D ( 'NONE', #7681, #21115, #221 ) ;
#25197 = CARTESIAN_POINT ( 'NONE',  ( 17.85084670134855145, 5.929878015568476712, -20.08862479909851828 ) ) ;
#25198 = CARTESIAN_POINT ( 'NONE',  ( 12.29957980484737767, 9.540162674316999158, -15.28991344586433421 ) ) ;
#25199 = CARTESIAN_POINT ( 'NONE',  ( 34.75406370242679799, -18.61511248754081294, -20.11778113987843852 ) ) ;
#25200 = ORIENTED_EDGE ( 'NONE', *, *, #12072, .F. ) ;
#25201 = AXIS2_PLACEMENT_3D ( 'NONE', #17532, #15241, #3368 ) ;
#25202 = CARTESIAN_POINT ( 'NONE',  ( 153.6922820468853388, -10.00000000000000178, 2.247092850131519715 ) ) ;
#25203 = VECTOR ( 'NONE', #279, 1000.000000000000000 ) ;
#25204 = CARTESIAN_POINT ( 'NONE',  ( 9.641350810849047548, 17.66889113945805789, -17.91664992932186351 ) ) ;
#25205 = CARTESIAN_POINT ( 'NONE',  ( 2.500000000000000444, 0.000000000000000000, 0.000000000000000000 ) ) ;
#25206 = CARTESIAN_POINT ( 'NONE',  ( 159.7287565553229172, -4.999999999999975131, -7.839745962155600267 ) ) ;
#25207 = ORIENTED_EDGE ( 'NONE', *, *, #7407, .F. ) ;
#25208 = LINE ( 'NONE', #18175, #19801 ) ;
#25209 = VERTEX_POINT ( 'NONE', #435 ) ;
#25210 = CARTESIAN_POINT ( 'NONE',  ( 12.87053260329167692, 9.517041913610183812, -16.11361789703515868 ) ) ;
#25211 = EDGE_CURVE ( 'NONE', #12251, #27629, #4243, .T. ) ;
#25212 = ADVANCED_FACE ( 'NONE', ( #21175 ), #7149, .F. ) ;
#25213 = VECTOR ( 'NONE', #13167, 1000.000000000000000 ) ;
#25214 = CARTESIAN_POINT ( 'NONE',  ( 34.31936231504242585, -12.17391896401218609, -19.91370162440023250 ) ) ;
#25215 = CARTESIAN_POINT ( 'NONE',  ( 28.15048769591263067, -5.842385520647848551, -16.89978903947823241 ) ) ;
#25216 = ORIENTED_EDGE ( 'NONE', *, *, #17817, .F. ) ;
#25218 = ADVANCED_FACE ( 'NONE', ( #11712 ), #25467, .T. ) ;
#25217 = PRODUCT_DEFINITION_SHAPE ( 'NONE', 'NONE',  #30271 ) ;
#25219 = DIRECTION ( 'NONE',  ( 0.9510565162951535312, 2.566386769018988816E-16, -0.3090169943749475623 ) ) ;
#25220 = CARTESIAN_POINT ( 'NONE',  ( 1.244173783436457737E-15, -5.000000000000017764, 0.000000000000000000 ) ) ;
#25221 =( LENGTH_UNIT ( ) NAMED_UNIT ( * ) SI_UNIT ( .MILLI., .METRE. ) );
#25222 = CARTESIAN_POINT ( 'NONE',  ( 22.98083118076628040, -7.181321033737746440, -13.97658420854277850 ) ) ;
#25223 = CARTESIAN_POINT ( 'NONE',  ( 25.54411345550068191, -6.057473962578058035, -19.57277538061955013 ) ) ;
#25224 =( GEOMETRIC_REPRESENTATION_CONTEXT ( 3 ) GLOBAL_UNCERTAINTY_ASSIGNED_CONTEXT ( ( #11325 ) ) GLOBAL_UNIT_ASSIGNED_CONTEXT ( ( #15429, #29850, #6737 ) ) REPRESENTATION_CONTEXT ( 'NONE', 'WORKASPACE' ) );
#25225 = ORIENTED_EDGE ( 'NONE', *, *, #27970, .F. ) ;
#25226 = CARTESIAN_POINT ( 'NONE',  ( 95.42913260352182192, -4.999999999999991118, 69.33332324712154104 ) ) ;
#25227 = AXIS2_PLACEMENT_3D ( 'NONE', #6935, #1918, #23109 ) ;
#25228 = LINE ( 'NONE', #15453, #5711 ) ;
#25229 = PLANE ( 'NONE',  #12141 ) ;
#25230 = DIRECTION ( 'NONE',  ( -0.9510565162951536422, 0.000000000000000000, -0.3090169943749472292 ) ) ;
#25231 = CARTESIAN_POINT ( 'NONE',  ( 12.53458732174692258, 8.585986940276173485, -15.10260830673100330 ) ) ;
#25232 = CARTESIAN_POINT ( 'NONE',  ( 133.6922820468854241, -1.999999999999981348, -0.6060766987539614181 ) ) ;
#25233 = VERTEX_POINT ( 'NONE', #19045 ) ;
#25234 = PLANE ( 'NONE',  #28142 ) ;
#25235 = EDGE_LOOP ( 'NONE', ( #24577, #20464, #23762, #10288 ) ) ;
#25236 = CARTESIAN_POINT ( 'NONE',  ( 9.641350810849047548, 17.66889113945805789, -17.95086732675817132 ) ) ;
#25237 = VECTOR ( 'NONE', #5952, 1000.000000000000000 ) ;
#25238 = CARTESIAN_POINT ( 'NONE',  ( 27.28133297882270014, -12.52022702279392874, -15.45456112525011427 ) ) ;
#25239 = DIRECTION ( 'NONE',  ( -2.698458740408365879E-16, 1.000000000000000000, 0.000000000000000000 ) ) ;
#25240 = FACE_OUTER_BOUND ( 'NONE', #22993, .T. ) ;
#25242 = ORIENTED_EDGE ( 'NONE', *, *, #17621, .T. ) ;
#25241 = CARTESIAN_POINT ( 'NONE',  ( 26.18758235895636233, -4.355437658720127558, -18.53605802859044260 ) ) ;
#25243 = DIRECTION ( 'NONE',  ( -2.698458740408365879E-16, 1.000000000000000000, 0.000000000000000000 ) ) ;
#25244 = CARTESIAN_POINT ( 'NONE',  ( 12.25159070717542065, 9.517778977577904698, -15.32825133053543887 ) ) ;
#25245 = ORIENTED_EDGE ( 'NONE', *, *, #23562, .F. ) ;
#25246 = EDGE_CURVE ( 'NONE', #13920, #10352, #13711, .T. ) ;
#25247 = CIRCLE ( 'NONE', #14015, 13.00000000000000178 ) ;
#25248 = CARTESIAN_POINT ( 'NONE',  ( 35.22227017426903473, -20.71851614966110233, -20.19360243392694088 ) ) ;
#25249 = DIRECTION ( 'NONE',  ( 0.3090169943749475623, 8.338696094058001131E-17, 0.9510565162951536422 ) ) ;
#25250 = VERTEX_POINT ( 'NONE', #28400 ) ;
#25251 = ADVANCED_FACE ( 'NONE', ( #14151 ), #7454, .T. ) ;
#25252 = CARTESIAN_POINT ( 'NONE',  ( 24.18219217278060995, -6.970120066757704791, -14.18070892486464629 ) ) ;
#25253 = CARTESIAN_POINT ( 'NONE',  ( 49.00000000000000000, -1.387778780781445676E-16, 5.000000000000000888 ) ) ;
#25254 = EDGE_CURVE ( 'NONE', #6140, #16946, #23173, .T. ) ;
#25255 = CARTESIAN_POINT ( 'NONE',  ( 20.47999367081501632, -2.041782396245861442, -15.93780510180117638 ) ) ;
#25256 = VERTEX_POINT ( 'NONE', #16604 ) ;
#25257 = CARTESIAN_POINT ( 'NONE',  ( 22.76426963133880221, -5.000000000000011546, -70.06121788019005692 ) ) ;
#25258 = CARTESIAN_POINT ( 'NONE',  ( 25.88562516208081021, -13.15641406947225889, -17.87304489109560990 ) ) ;
#25259 = CARTESIAN_POINT ( 'NONE',  ( 30.94061990612449264, -11.12808277128230294, -15.28946652318938959 ) ) ;
#25260 = ORIENTED_EDGE ( 'NONE', *, *, #6403, .T. ) ;
#25261 = ORIENTED_EDGE ( 'NONE', *, *, #19616, .T. ) ;
#25262 = LINE ( 'NONE', #4347, #17540 ) ;
#25263 = VECTOR ( 'NONE', #30049, 1000.000000000000000 ) ;
#25264 = DIRECTION ( 'NONE',  ( 0.000000000000000000, 0.000000000000000000, 1.000000000000000000 ) ) ;
#25265 = PLANE ( 'NONE',  #15581 ) ;
#25266 = VECTOR ( 'NONE', #11563, 999.9999999999998863 ) ;
#25267 = CARTESIAN_POINT ( 'NONE',  ( 176.1922820468852535, -9.999999999999994671, -2.083034168790677043 ) ) ;
#25268 = DIRECTION ( 'NONE',  ( 0.000000000000000000, 0.000000000000000000, -1.000000000000000000 ) ) ;
#25269 = DIRECTION ( 'NONE',  ( -1.000000000000000000, -2.698458740408365879E-16, 1.779203565104417375E-16 ) ) ;
#25270 = CARTESIAN_POINT ( 'NONE',  ( 23.05283280155556724, -4.691836721735100468, -12.69353859562758124 ) ) ;
#25271 = CARTESIAN_POINT ( 'NONE',  ( 17.97606266963480692, 4.724414365053664966, -20.23074386977120298 ) ) ;
#25272 = CARTESIAN_POINT ( 'NONE',  ( 36.54859390953723874, -22.18451583373416014, -15.00000000000000000 ) ) ;
#25273 = DIRECTION ( 'NONE',  ( 0.000000000000000000, 2.775557561562890735E-17, -1.000000000000000000 ) ) ;
#25274 = CARTESIAN_POINT ( 'NONE',  ( 11.47231678315799464, 9.271847796573304379, -15.86114366194887815 ) ) ;
#25275 = DIRECTION ( 'NONE',  ( 0.000000000000000000, -2.775557561562890735E-17, 1.000000000000000000 ) ) ;
#25276 = DIRECTION ( 'NONE',  ( -0.5877852522924731371, 0.000000000000000000, 0.8090169943749474513 ) ) ;
#25277 = CARTESIAN_POINT ( 'NONE',  ( 9.732710754582456048, 15.93000180522596665, -17.85826136589200175 ) ) ;
#25278 = PLANE ( 'NONE',  #10722 ) ;
#25279 = EDGE_LOOP ( 'NONE', ( #21245, #18352 ) ) ;
#25280 = DIRECTION ( 'NONE',  ( 0.5877852522924731371, 1.586114251531760728E-16, -0.8090169943749474513 ) ) ;
#25281 = CARTESIAN_POINT ( 'NONE',  ( 15.61762486822808604, 9.948436389806387226, -12.64537296286936829 ) ) ;
#25282 = ORIENTED_EDGE ( 'NONE', *, *, #17246, .F. ) ;
#25283 = FACE_OUTER_BOUND ( 'NONE', #29979, .T. ) ;
#25284 = CARTESIAN_POINT ( 'NONE',  ( 152.2287565553230024, -1.999999999999974909, -20.83012701892220520 ) ) ;
#25285 = ORIENTED_EDGE ( 'NONE', *, *, #7200, .F. ) ;
#25286 = ADVANCED_FACE ( 'NONE', ( #11555 ), #25926, .F. ) ;
#25287 = EDGE_CURVE ( 'NONE', #16652, #29408, #20871, .T. ) ;
#25288 = ADVANCED_FACE ( 'NONE', ( #4701 ), #13993, .T. ) ;
#25289 = ORIENTED_EDGE ( 'NONE', *, *, #23417, .T. ) ;
#25290 = EDGE_CURVE ( 'NONE', #2121, #15637, #136, .T. ) ;
#25291 = CARTESIAN_POINT ( 'NONE',  ( 9.153102208164984432, 15.99530481237056989, -17.03794677594065021 ) ) ;
#25292 = CARTESIAN_POINT ( 'NONE',  ( 35.54859125455464408, -23.18450390630307822, -18.42126094939176895 ) ) ;
#25293 = CONICAL_SURFACE ( 'NONE', #18947, 8.000000000000007105, 1.047197551196596077 ) ;
#25294 = CARTESIAN_POINT ( 'NONE',  ( 18.57670912428364574, -0.2836015139962214660, -15.28694485256269608 ) ) ;
#25295 = CARTESIAN_POINT ( 'NONE',  ( 17.54325408622900184, 7.715740848240963068, -20.30207397218512000 ) ) ;
#25296 = AXIS2_PLACEMENT_3D ( 'NONE', #16908, #21796, #26392 ) ;
#25297 = LINE ( 'NONE', #20397, #24512 ) ;
#25298 = CARTESIAN_POINT ( 'NONE',  ( 19.06759106800826586, -1.100202736525451641, -14.71838255749352165 ) ) ;
#25299 = VECTOR ( 'NONE', #6046, 1000.000000000000114 ) ;
#25300 = EDGE_LOOP ( 'NONE', ( #18479, #6184, #15526, #2752, #10136 ) ) ;
#25301 = DIRECTION ( 'NONE',  ( 1.000000000000000000, 0.000000000000000000, 0.000000000000000000 ) ) ;
#25303 = ORIENTED_EDGE ( 'NONE', *, *, #10601, .F. ) ;
#25302 = DIRECTION ( 'NONE',  ( 1.110223024625156540E-16, 2.995891024602366092E-32, 1.000000000000000000 ) ) ;
#25304 = ORIENTED_EDGE ( 'NONE', *, *, #9721, .T. ) ;
#25305 = FACE_OUTER_BOUND ( 'NONE', #6705, .T. ) ;
#25306 = DIRECTION ( 'NONE',  ( -0.8090169943749474513, -2.183098979609982436E-16, 0.5877852522924731371 ) ) ;
#25307 = ORIENTED_EDGE ( 'NONE', *, *, #26868, .T. ) ;
#25308 = CARTESIAN_POINT ( 'NONE',  ( 35.24753590068310416, -19.83202167481471889, -19.22462439892593977 ) ) ;
#25309 = VECTOR ( 'NONE', #7214, 1000.000000000000000 ) ;
#25310 = CARTESIAN_POINT ( 'NONE',  ( 10.65249265583095095, 9.118909091547207524, -16.41789608165773728 ) ) ;
#25311 = ORIENTED_EDGE ( 'NONE', *, *, #23772, .F. ) ;
#25312 = CARTESIAN_POINT ( 'NONE',  ( 29.90031526554274777, -7.862644070287768905, -16.42500436498598049 ) ) ;
#25313 = DIRECTION ( 'NONE',  ( 1.110223024625156540E-16, 2.995891024602366092E-32, 1.000000000000000000 ) ) ;
#25314 = CARTESIAN_POINT ( 'NONE',  ( 10.47175433613752027, 16.45341039028688002, -17.33491556667247835 ) ) ;
#25315 = DIRECTION ( 'NONE',  ( 0.5877852522924731371, 1.586114251531760728E-16, -0.8090169943749474513 ) ) ;
#25316 = VECTOR ( 'NONE', #26801, 1000.000000000000000 ) ;
#25317 = DIRECTION ( 'NONE',  ( 1.110223024625156540E-16, 2.995891024602366092E-32, 1.000000000000000000 ) ) ;
#25318 = EDGE_LOOP ( 'NONE', ( #20065, #327, #16527, #23393 ) ) ;
#25319 = CARTESIAN_POINT ( 'NONE',  ( 157.0152310637604671, -1.999999999999974909, 1.702185954127501066 ) ) ;
#25320 = EDGE_CURVE ( 'NONE', #25907, #4151, #1160, .T. ) ;
#25321 = CARTESIAN_POINT ( 'NONE',  ( 12.51757296969303290, 8.578467993704791184, -15.11616904564172792 ) ) ;
#25322 = ORIENTED_EDGE ( 'NONE', *, *, #27483, .T. ) ;
#25323 = EDGE_LOOP ( 'NONE', ( #12294, #30086, #17381, #11588, #3992 ) ) ;
#25324 = EDGE_CURVE ( 'NONE', #22451, #25397, #10294, .T. ) ;
#25325 = DIRECTION ( 'NONE',  ( 1.000000000000000000, 4.440892098500622217E-16, 0.000000000000000000 ) ) ;
#25326 = EDGE_LOOP ( 'NONE', ( #27906, #13076, #28136, #23446 ) ) ;
#25327 = EDGE_CURVE ( 'NONE', #7152, #5129, #29586, .T. ) ;
#25328 = CARTESIAN_POINT ( 'NONE',  ( 10.96464236563772943, 10.28020640217055259, -17.34881430896752619 ) ) ;
#25329 = CARTESIAN_POINT ( 'NONE',  ( 24.32739057165333207, -2.318628849198325348, -18.36682367714799824 ) ) ;
#25330 = CARTESIAN_POINT ( 'NONE',  ( 23.89160689111651337, -1.335809292830872241, -14.36923488517323477 ) ) ;
#25331 = CARTESIAN_POINT ( 'NONE',  ( 21.13650371987585075, 4.769999862021419901, -15.38713752973847448 ) ) ;
#25332 = DIRECTION ( 'NONE',  ( 0.3331260486002958765, -0.05059491534325381845, -0.9415238660200613285 ) ) ;
#25333 = DIRECTION ( 'NONE',  ( -0.000000000000000000, 0.000000000000000000, 1.000000000000000000 ) ) ;
#25334 = VECTOR ( 'NONE', #30128, 1000.000000000000000 ) ;
#25335 = CARTESIAN_POINT ( 'NONE',  ( 24.66978787416869068, -0.3063955544261361963, -14.42797892638687784 ) ) ;
#25336 = VECTOR ( 'NONE', #19650, 1000.000000000000000 ) ;
#25337 = CARTESIAN_POINT ( 'NONE',  ( 162.0152310637604103, -1.999999999999973577, -0.06116980274991495881 ) ) ;
#25338 = DIRECTION ( 'NONE',  ( -0.9510565162951536422, 0.000000000000000000, -0.3090169943749472292 ) ) ;
#25339 = EDGE_CURVE ( 'NONE', #6838, #7265, #17763, .T. ) ;
#25340 = CARTESIAN_POINT ( 'NONE',  ( 10.35864918915110877, 16.97212501191939538, -17.92454625180715766 ) ) ;
#25341 = DIRECTION ( 'NONE',  ( 0.000000000000000000, 0.000000000000000000, 1.000000000000000000 ) ) ;
#25342 = CARTESIAN_POINT ( 'NONE',  ( 2.500000000000000444, -1.768423874527823347, 1.021000000000001018 ) ) ;
#25343 = ORIENTED_EDGE ( 'NONE', *, *, #8456, .T. ) ;
#25344 = DIRECTION ( 'NONE',  ( -0.9510565162951536422, -2.566386769018988323E-16, 0.3090169943749475623 ) ) ;
#25345 = CARTESIAN_POINT ( 'NONE',  ( 16.34386185847872142, 4.569898679961749366, -19.52586945278800812 ) ) ;
#25346 = CARTESIAN_POINT ( 'NONE',  ( 11.05542614047498873, 17.68937375096277265, -17.90480922774079175 ) ) ;
#25347 = DIRECTION ( 'NONE',  ( -2.698458740408365879E-16, 1.000000000000000000, 0.000000000000000000 ) ) ;
#25348 = ORIENTED_EDGE ( 'NONE', *, *, #22671, .F. ) ;
#25349 = VECTOR ( 'NONE', #15658, 1000.000000000000000 ) ;
#25350 = VERTEX_POINT ( 'NONE', #17315 ) ;
#25351 = CARTESIAN_POINT ( 'NONE',  ( 9.917332382238186028, 16.40320447359955125, -16.50418441153501448 ) ) ;
#25352 = CARTESIAN_POINT ( 'NONE',  ( 9.641890818133653340, 17.66641459721583374, -17.82828029666912073 ) ) ;
#25353 = CARTESIAN_POINT ( 'NONE',  ( -1.310841663519413114, 0.000000000000000000, 0.000000000000000000 ) ) ;
#25354 = CARTESIAN_POINT ( 'NONE',  ( 147.0152310637605524, -1.999999999999976685, -17.38167787843871182 ) ) ;
#25355 = VECTOR ( 'NONE', #11395, 1000.000000000000000 ) ;
#25356 = ORIENTED_EDGE ( 'NONE', *, *, #11405, .F. ) ;
#25357 = LINE ( 'NONE', #20463, #25674 ) ;
#25358 = ORIENTED_EDGE ( 'NONE', *, *, #20200, .F. ) ;
#25359 = CARTESIAN_POINT ( 'NONE',  ( 10.35864918915110877, 16.97212501191939538, -17.98596209335946128 ) ) ;
#25360 = CARTESIAN_POINT ( 'NONE',  ( 34.28781561389841670, -12.04879923890588422, -19.89451123369701691 ) ) ;
#25361 = CARTESIAN_POINT ( 'NONE',  ( 26.04489551603160180, -6.130266781319400948, -13.71289979607875154 ) ) ;
#25362 = ORIENTED_EDGE ( 'NONE', *, *, #14270, .T. ) ;
#25363 = CARTESIAN_POINT ( 'NONE',  ( 162.0152310637604387, -1.999999999999973133, -8.721423840594312082 ) ) ;
#25364 = DIRECTION ( 'NONE',  ( 1.000000000000000000, 0.000000000000000000, 0.000000000000000000 ) ) ;
#25365 = VECTOR ( 'NONE', #12275, 1000.000000000000000 ) ;
#25366 = SHAPE_DEFINITION_REPRESENTATION ( #3755, #23798 ) ;
#25367 = VECTOR ( 'NONE', #23585, 1000.000000000000000 ) ;
#25368 = CARTESIAN_POINT ( 'NONE',  ( 14.69068284915647560, 4.968298739062387170, -17.53091140782979807 ) ) ;
#25369 = CARTESIAN_POINT ( 'NONE',  ( 21.89112544314524200, -5.209854132323804343, -13.34451667507982364 ) ) ;
#25370 = EDGE_LOOP ( 'NONE', ( #26577, #512, #5077, #22762 ) ) ;
#25371 = DIRECTION ( 'NONE',  ( 0.5877852522924731371, 1.586114251531760728E-16, -0.8090169943749474513 ) ) ;
#25372 = AXIS2_PLACEMENT_3D ( 'NONE', #27959, #21190, #9590 ) ;
#25373 = EDGE_CURVE ( 'NONE', #25744, #13500, #14482, .T. ) ;
#25374 = CARTESIAN_POINT ( 'NONE',  ( 75.00000000000000000, 0.000000000000000000, 0.000000000000000000 ) ) ;
#25375 = CARTESIAN_POINT ( 'NONE',  ( 144.5152310637605524, -1.999999999999977573, -13.05155085951651195 ) ) ;
#25376 = EDGE_CURVE ( 'NONE', #4884, #10508, #21486, .T. ) ;
#25377 = DIRECTION ( 'NONE',  ( -0.9510565162951536422, -2.566386769018988816E-16, -0.3090169943749472292 ) ) ;
#25378 = UNCERTAINTY_MEASURE_WITH_UNIT (LENGTH_MEASURE( 1.000000000000000082E-05 ), #17320, 'distance_accuracy_value', 'NONE');
#25379 = CARTESIAN_POINT ( 'NONE',  ( 10.78565875124225393, 16.33370571569710705, -15.92737460872590738 ) ) ;
#25381 = VECTOR ( 'NONE', #8188, 1000.000000000000000 ) ;
#25380 = CARTESIAN_POINT ( 'NONE',  ( 26.88053589187069292, -12.95240298029966119, -14.33176627689639382 ) ) ;
#25382 =( GEOMETRIC_REPRESENTATION_CONTEXT ( 3 ) GLOBAL_UNCERTAINTY_ASSIGNED_CONTEXT ( ( #27261 ) ) GLOBAL_UNIT_ASSIGNED_CONTEXT ( ( #15008, #3585, #8299 ) ) REPRESENTATION_CONTEXT ( 'NONE', 'WORKASPACE' ) );
#25383 = ORIENTED_EDGE ( 'NONE', *, *, #12930, .F. ) ;
#25384 = CARTESIAN_POINT ( 'NONE',  ( 159.5152310637604387, -4.999999999999974243, -4.391296821672111328 ) ) ;
#25385 = ORIENTED_EDGE ( 'NONE', *, *, #7121, .F. ) ;
#25386 = VECTOR ( 'NONE', #18019, 1000.000000000000000 ) ;
#25387 = CARTESIAN_POINT ( 'NONE',  ( 11.47079713067724782, 9.278817116560638567, -15.86177209170659275 ) ) ;
#25388 = CARTESIAN_POINT ( 'NONE',  ( 15.31194320040279777, 8.488938064892046498, -14.62880434596509183 ) ) ;
#25389 = CARTESIAN_POINT ( 'NONE',  ( 152.2287565553229456, -10.00000000000000178, -3.509618943233403510 ) ) ;
#25390 = CARTESIAN_POINT ( 'NONE',  ( 169.5152310637604387, -9.999999999999996447, -13.05155085951651195 ) ) ;
#25392 = ORIENTED_EDGE ( 'NONE', *, *, #17179, .F. ) ;
#25391 = CARTESIAN_POINT ( 'NONE',  ( 26.87449084144840938, -11.88902188497427481, -13.49525739704605343 ) ) ;
#25393 = ORIENTED_EDGE ( 'NONE', *, *, #23556, .T. ) ;
#25394 = CARTESIAN_POINT ( 'NONE',  ( 23.71918465946406229, -5.000000000000011546, -73.00014414165241305 ) ) ;
#25395 = CARTESIAN_POINT ( 'NONE',  ( 12.25193961909737794, 9.519109623917222152, -15.32788351481347355 ) ) ;
#25396 = EDGE_CURVE ( 'NONE', #22051, #20539, #1017, .T. ) ;
#25397 = VERTEX_POINT ( 'NONE', #19749 ) ;
#25398 = CARTESIAN_POINT ( 'NONE',  ( 35.54859390953724585, -22.18451583373416014, -17.22552805718784441 ) ) ;
#25399 = LINE ( 'NONE', #14226, #15662 ) ;
#25400 = DIRECTION ( 'NONE',  ( -0.5877852522924731371, 0.000000000000000000, 0.8090169943749474513 ) ) ;
#25401 = CARTESIAN_POINT ( 'NONE',  ( 23.72730982194951466, -1.509008702439352589, -18.09242500859757996 ) ) ;
#25402 = ORIENTED_EDGE ( 'NONE', *, *, #8952, .T. ) ;
#25403 = PLANE ( 'NONE',  #6679 ) ;
#25404 = CARTESIAN_POINT ( 'NONE',  ( 28.55206495951409096, -10.69471729813234795, -19.99811924356017911 ) ) ;
#25405 = CARTESIAN_POINT ( 'NONE',  ( 29.77493782482978091, -9.049732786019394126, -14.43420072379011643 ) ) ;
#25406 = VERTEX_POINT ( 'NONE', #24808 ) ;
#25407 = AXIS2_PLACEMENT_3D ( 'NONE', #6361, #13363, #22687 ) ;
#25408 = DIRECTION ( 'NONE',  ( -2.698458740408365879E-16, 1.000000000000000000, 0.000000000000000000 ) ) ;
#25409 = VECTOR ( 'NONE', #21748, 1000.000000000000000 ) ;
#25410 = CARTESIAN_POINT ( 'NONE',  ( 2.500000000000002665, 1.416384724411995397E-15, -2.424599999999998978 ) ) ;
#25411 = EDGE_CURVE ( 'NONE', #22699, #966, #12167, .T. ) ;
#25412 = EDGE_CURVE ( 'NONE', #3067, #2371, #29118, .T. ) ;
#25413 = CARTESIAN_POINT ( 'NONE',  ( 144.5152310637605524, -4.999999999999978684, -1.604441369360116192E-14 ) ) ;
#25414 = CARTESIAN_POINT ( 'NONE',  ( 167.0152310637604103, -4.999999999999972466, -0.06116980274991495881 ) ) ;
#25415 = EDGE_CURVE ( 'NONE', #4159, #11708, #10894, .T. ) ;
#25416 = PLANE ( 'NONE',  #21637 ) ;
#25417 = EDGE_CURVE ( 'NONE', #19263, #14150, #6180, .T. ) ;
#25418 = DIRECTION ( 'NONE',  ( -2.698458740408365879E-16, 1.000000000000000000, 0.000000000000000000 ) ) ;
#25419 = CARTESIAN_POINT ( 'NONE',  ( 18.23559491442917135, -2.176271773050306724, -15.57877364869929515 ) ) ;
#25420 = CARTESIAN_POINT ( 'NONE',  ( 20.73027244251523626, 3.305903845835247434, -19.25852547563239625 ) ) ;
#25421 = CARTESIAN_POINT ( 'NONE',  ( 33.08402606333302742, -12.15068820457383403, -20.63309441556253176 ) ) ;
#25422 = LINE ( 'NONE', #16097, #8061 ) ;
#25423 = CARTESIAN_POINT ( 'NONE',  ( 11.65548303173490652, 8.849831895876286936, -15.75351705932409985 ) ) ;
#25424 = PLANE ( 'NONE',  #12232 ) ;
#25425 = LINE ( 'NONE', #24988, #9528 ) ;
#25426 = FACE_OUTER_BOUND ( 'NONE', #1456, .T. ) ;
#25427 = ORIENTED_EDGE ( 'NONE', *, *, #8065, .F. ) ;
#25428 = LINE ( 'NONE', #697, #14889 ) ;
#25429 = CARTESIAN_POINT ( 'NONE',  ( 12.46899830068120352, 8.557956911948249257, -15.15481108270911825 ) ) ;
#25430 = EDGE_LOOP ( 'NONE', ( #7875, #28870, #26446, #23824 ) ) ;
#25431 = VECTOR ( 'NONE', #17304, 1000.000000000000000 ) ;
#25432 = LINE ( 'NONE', #13809, #28601 ) ;
#25433 = DIRECTION ( 'NONE',  ( -2.698458740408365879E-16, 1.000000000000000000, 0.000000000000000000 ) ) ;
#25434 = FACE_OUTER_BOUND ( 'NONE', #12836, .T. ) ;
#25435 = EDGE_LOOP ( 'NONE', ( #18949, #21445, #11144 ) ) ;
#25436 = CARTESIAN_POINT ( 'NONE',  ( 9.112223960064733674, 16.18277766892301983, -17.05485288603163951 ) ) ;
#25437 = CARTESIAN_POINT ( 'NONE',  ( 34.86302720852563652, -20.10462780087231138, -21.19305451400748552 ) ) ;
#25438 = CARTESIAN_POINT ( 'NONE',  ( 15.95545008109832530, 6.956385541780823800, -13.20154910664163950 ) ) ;
#25439 = CARTESIAN_POINT ( 'NONE',  ( 15.50826552155665183, 8.864470348925614474, -13.64319937614855149 ) ) ;
#25440 = DIRECTION ( 'NONE',  ( 0.000000000000000000, -1.000000000000000000, -0.000000000000000000 ) ) ;
#25441 = CARTESIAN_POINT ( 'NONE',  ( 25.18022790295009727, 0.7303485828293051485, -17.76052596840512621 ) ) ;
#25442 = VECTOR ( 'NONE', #14645, 1000.000000000000000 ) ;
#25443 = ORIENTED_EDGE ( 'NONE', *, *, #2942, .F. ) ;
#25444 = FACE_OUTER_BOUND ( 'NONE', #26004, .T. ) ;
#25445 = ORIENTED_EDGE ( 'NONE', *, *, #7697, .F. ) ;
#25447 = ORIENTED_EDGE ( 'NONE', *, *, #3278, .F. ) ;
#25446 = CARTESIAN_POINT ( 'NONE',  ( 142.2287565553230309, -1.999999999999978018, -20.83012701892220164 ) ) ;
#25448 = VERTEX_POINT ( 'NONE', #24504 ) ;
#25449 = ADVANCED_FACE ( 'NONE', ( #12737 ), #22516, .F. ) ;
#25450 = PLANE ( 'NONE',  #4121 ) ;
#25451 = EDGE_CURVE ( 'NONE', #26769, #10452, #26656, .T. ) ;
#25452 = ADVANCED_FACE ( 'NONE', ( #12884 ), #14450, .T. ) ;
#25453 = DIRECTION ( 'NONE',  ( -2.698458740408366372E-16, 1.000000000000000000, 0.000000000000000000 ) ) ;
#25454 = CARTESIAN_POINT ( 'NONE',  ( 36.30315773322485740, -20.08190110472122214, -19.47147371593984388 ) ) ;
#25455 = CARTESIAN_POINT ( 'NONE',  ( 12.00353595525870887, 7.537035219234042849, -15.50727442731917272 ) ) ;
#25456 = ORIENTED_EDGE ( 'NONE', *, *, #24246, .F. ) ;
#25457 = PLANE ( 'NONE',  #28373 ) ;
#25458 = CARTESIAN_POINT ( 'NONE',  ( 158.6922820468854241, -9.999999999999998224, -32.39392330124607611 ) ) ;
#25459 = CARTESIAN_POINT ( 'NONE',  ( 10.48820292689142519, 16.37797505638186735, -17.32811247259324716 ) ) ;
#25460 = FACE_BOUND ( 'NONE', #26201, .T. ) ;
#25461 = FACE_OUTER_BOUND ( 'NONE', #2721, .T. ) ;
#25462 = EDGE_LOOP ( 'NONE', ( #1697, #10415, #12379, #17962, #17649 ) ) ;
#25463 = CARTESIAN_POINT ( 'NONE',  ( 144.7287565553230309, -1.999999999999977129, -33.82050807568879947 ) ) ;
#25464 = DIRECTION ( 'NONE',  ( 0.000000000000000000, 0.000000000000000000, -1.000000000000000000 ) ) ;
#25465 = VERTEX_POINT ( 'NONE', #2883 ) ;
#25466 = ORIENTED_EDGE ( 'NONE', *, *, #23846, .T. ) ;
#25467 = CYLINDRICAL_SURFACE ( 'NONE', #16429, 4.000000000000001776 ) ;
#25468 = EDGE_LOOP ( 'NONE', ( #21663, #18931, #9260, #12163 ) ) ;
#25469 = CARTESIAN_POINT ( 'NONE',  ( 9.661894807476521407, 16.25477276558749296, -17.91386948909976695 ) ) ;
#25470 = CARTESIAN_POINT ( 'NONE',  ( 20.53830075755067952, -2.223150928429542095, -18.95983797452030828 ) ) ;
#25471 = CARTESIAN_POINT ( 'NONE',  ( 24.26229878782818261, 2.002655289519151172, -16.31248287692968546 ) ) ;
#25472 = ORIENTED_EDGE ( 'NONE', *, *, #6301, .T. ) ;
#25473 = CARTESIAN_POINT ( 'NONE',  ( 18.63710449947919301, 3.826706299981984305, -14.11708861520305192 ) ) ;
#25474 = CARTESIAN_POINT ( 'NONE',  ( 168.6922820468853388, -1.999999999999971356, -17.92658477444275889 ) ) ;
#25475 = CARTESIAN_POINT ( 'NONE',  ( -3.319543390096041602, 7.321065037175435108, -0.01688885742777280694 ) ) ;
#25476 = ORIENTED_EDGE ( 'NONE', *, *, #14268, .F. ) ;
#25477 = CARTESIAN_POINT ( 'NONE',  ( -4.339467034331215167, -6.732211846623414431, -1.342271935690208390E-14 ) ) ;
#25478 = CARTESIAN_POINT ( 'NONE',  ( 28.09718568327657806, -5.958257988085632562, -17.17874431236187149 ) ) ;
#25479 = VECTOR ( 'NONE', #21188, 1000.000000000000000 ) ;
#25480 = ORIENTED_EDGE ( 'NONE', *, *, #15028, .T. ) ;
#25481 = LINE ( 'NONE', #7168, #21776 ) ;
#25482 = DIRECTION ( 'NONE',  ( -0.5877852522924731371, 0.000000000000000000, 0.8090169943749474513 ) ) ;
#25483 = DIRECTION ( 'NONE',  ( -0.5877852522924731371, -1.586114251531760235E-16, 0.8090169943749474513 ) ) ;
#25484 = EDGE_CURVE ( 'NONE', #29002, #5247, #28678, .T. ) ;
#25485 = EDGE_CURVE ( 'NONE', #12041, #5801, #3447, .T. ) ;
#25486 = DIRECTION ( 'NONE',  ( 1.110223024625156540E-16, 2.995891024602366092E-32, 1.000000000000000000 ) ) ;
#25487 = FACE_OUTER_BOUND ( 'NONE', #26782, .T. ) ;
#25488 = VECTOR ( 'NONE', #26242, 1000.000000000000000 ) ;
#25489 = EDGE_CURVE ( 'NONE', #28726, #15010, #26973, .T. ) ;
#25490 = ADVANCED_FACE ( 'NONE', ( #24648 ), #1357, .T. ) ;
#25491 = DIRECTION ( 'NONE',  ( 0.000000000000000000, 0.000000000000000000, -1.000000000000000000 ) ) ;
#25492 = DIRECTION ( 'NONE',  ( -1.000000000000000000, -4.440892098500623203E-16, 0.000000000000000000 ) ) ;
#25493 = CARTESIAN_POINT ( 'NONE',  ( 159.5152310637605240, -9.999999999999998224, -19.94844914048349693 ) ) ;
#25494 = VERTEX_POINT ( 'NONE', #17904 ) ;
#25495 = VERTEX_POINT ( 'NONE', #11051 ) ;
#25496 = DIRECTION ( 'NONE',  ( -0.5877852522924731371, -1.586114251531760235E-16, 0.8090169943749474513 ) ) ;
#25497 = CARTESIAN_POINT ( 'NONE',  ( 19.20291185354690811, 8.143073066566493878, -16.32372945079811188 ) ) ;
#25498 = CARTESIAN_POINT ( 'NONE',  ( 11.21766632152761822, 16.94531959984159641, -16.84123939818963223 ) ) ;
#25499 = CARTESIAN_POINT ( 'NONE',  ( 33.44337896868773186, -12.72690026786775341, -19.72159258799634074 ) ) ;
#25500 = EDGE_LOOP ( 'NONE', ( #762, #18682, #10087, #20858 ) ) ;
#25501 = ORIENTED_EDGE ( 'NONE', *, *, #1454, .F. ) ;
#25502 = CARTESIAN_POINT ( 'NONE',  ( 9.916336358462064737, 16.40777236560037622, -16.50459729666445696 ) ) ;
#25503 = CARTESIAN_POINT ( 'NONE',  ( 9.641350810849047548, 17.66889113945805789, -17.98596209335946128 ) ) ;
#25504 = CARTESIAN_POINT ( 'NONE',  ( 133.6922820468854241, -10.00000000000000711, -15.07341522555727309 ) ) ;
#25505 = LINE ( 'NONE', #5347, #8166 ) ;
#25506 = ORIENTED_EDGE ( 'NONE', *, *, #18942, .F. ) ;
#25507 = CARTESIAN_POINT ( 'NONE',  ( 133.7287565553229172, -9.999999999999980460, -33.50000000000000000 ) ) ;
#25508 = ORIENTED_EDGE ( 'NONE', *, *, #21137, .T. ) ;
#25509 = CARTESIAN_POINT ( 'NONE',  ( 10.38089682401341385, 16.87009452252716102, -17.57504515238516873 ) ) ;
#25510 = CARTESIAN_POINT ( 'NONE',  ( 34.38415957124060895, -12.46085888452578594, -19.93570721963346060 ) ) ;
#25511 = CARTESIAN_POINT ( 'NONE',  ( 28.12266609392075267, -5.599633216697744942, -16.00068813756295327 ) ) ;
#25512 = EDGE_LOOP ( 'NONE', ( #18248, #20165, #4222, #10438, #25466 ) ) ;
#25513 = CARTESIAN_POINT ( 'NONE',  ( 0.000000000000000000, 0.000000000000000000, 18.00000000000000000 ) ) ;
#25514 = CARTESIAN_POINT ( 'NONE',  ( 139.5152310637605808, -4.999999999999980460, -13.05155085951651195 ) ) ;
#25515 = DIRECTION ( 'NONE',  ( 1.000000000000000000, 0.000000000000000000, 0.000000000000000000 ) ) ;
#25516 = CARTESIAN_POINT ( 'NONE',  ( 13.80032290073870449, 8.087308377618120048, -14.09379472307618641 ) ) ;
#25517 = CARTESIAN_POINT ( 'NONE',  ( 25.51035504519657593, -9.958856436819656821, -16.28203429854516315 ) ) ;
#25518 = EDGE_LOOP ( 'NONE', ( #21598, #26343, #7717, #29198 ) ) ;
#25519 = AXIS2_PLACEMENT_3D ( 'NONE', #29949, #2130, #8817 ) ;
#25520 = DIRECTION ( 'NONE',  ( 0.9510565162951536422, 2.566386769018988816E-16, 0.3090169943749472292 ) ) ;
#25521 = EDGE_CURVE ( 'NONE', #6680, #12148, #2215, .T. ) ;
#25522 = CARTESIAN_POINT ( 'NONE',  ( 139.5152310637605808, -10.00000000000000533, -13.05155085951651195 ) ) ;
#25523 = LINE ( 'NONE', #18343, #24328 ) ;
#25524 = CARTESIAN_POINT ( 'NONE',  ( 133.7287565553229456, -4.999999999999982236, 0.5000000000000029976 ) ) ;
#25525 = AXIS2_PLACEMENT_3D ( 'NONE', #11103, #6391, #27025 ) ;
#25526 = CARTESIAN_POINT ( 'NONE',  ( 10.33811697311952216, 18.38618935847563307, -17.91478972043705298 ) ) ;
#25527 = DIRECTION ( 'NONE',  ( -0.9510565162951536422, 0.000000000000000000, -0.3090169943749472292 ) ) ;
#25528 = DIRECTION ( 'NONE',  ( -2.698458740408365879E-16, 1.000000000000000000, 0.000000000000000000 ) ) ;
#25529 = ORIENTED_EDGE ( 'NONE', *, *, #7725, .F. ) ;
#25530 = CARTESIAN_POINT ( 'NONE',  ( 9.916411867603999397, 16.40742607105030260, -16.50456570466356965 ) ) ;
#25531 = CARTESIAN_POINT ( 'NONE',  ( 16.02697758069565381, 6.204487712298734081, -15.55946274640501237 ) ) ;
#25532 = CYLINDRICAL_SURFACE ( 'NONE', #23426, 5.000000000000000888 ) ;
#25533 = LINE ( 'NONE', #13772, #24346 ) ;
#25535 = ORIENTED_EDGE ( 'NONE', *, *, #24702, .T. ) ;
#25534 = CARTESIAN_POINT ( 'NONE',  ( 31.59793210864275537, -10.01186915388335485, -14.42687813506083039 ) ) ;
#25536 = ORIENTED_EDGE ( 'NONE', *, *, #25875, .F. ) ;
#25537 = CARTESIAN_POINT ( 'NONE',  ( 138.6922820468854525, -10.00000000000000533, -9.266330736598359152 ) ) ;
#25538 = CARTESIAN_POINT ( 'NONE',  ( 11.34095285796786712, 16.37991182834946713, -16.75774407480071559 ) ) ;
#25539 = EDGE_LOOP ( 'NONE', ( #17206, #5006, #28780, #17403, #18772, #21577, #1341, #10089 ) ) ;
#25540 = CARTESIAN_POINT ( 'NONE',  ( 35.07504771885155037, -20.05712364337910714, -20.21480690768607857 ) ) ;
#25541 = LINE ( 'NONE', #6933, #1066 ) ;
#25542 = DIRECTION ( 'NONE',  ( 0.5877852522924731371, 0.000000000000000000, 0.8090169943749474513 ) ) ;
#25543 = CARTESIAN_POINT ( 'NONE',  ( 24.92984004655564334, -8.306894832562658593, -19.61321747044761921 ) ) ;
#25544 = EDGE_LOOP ( 'NONE', ( #20498, #18465, #29682, #27715 ) ) ;
#25545 = LINE ( 'NONE', #25102, #10569 ) ;
#25546 = ADVANCED_FACE ( 'NONE', ( #27573 ), #2342, .T. ) ;
#25547 = CARTESIAN_POINT ( 'NONE',  ( 20.05507840940144959, 2.642024363331392234, -19.51255487852252912 ) ) ;
#25548 = CARTESIAN_POINT ( 'NONE',  ( 26.63012090756776828, -10.30360588212082007, -13.56444477573641905 ) ) ;
#25549 = AXIS2_PLACEMENT_3D ( 'NONE', #22831, #4648, #4955 ) ;
#25550 = ORIENTED_EDGE ( 'NONE', *, *, #3640, .F. ) ;
#25551 = DIRECTION ( 'NONE',  ( 0.9510565162951536422, 0.000000000000000000, -0.3090169943749475623 ) ) ;
#25552 = FACE_OUTER_BOUND ( 'NONE', #3166, .T. ) ;
#25553 = DIRECTION ( 'NONE',  ( -2.698458740408365879E-16, 1.000000000000000000, -0.000000000000000000 ) ) ;
#25554 = CARTESIAN_POINT ( 'NONE',  ( 175.7287565553229456, -4.999999999999969802, -28.21440484423852979 ) ) ;
#25555 = CARTESIAN_POINT ( 'NONE',  ( 9.905109554012803130, 16.45925992188944420, -16.51025697316969953 ) ) ;
#25556 = CARTESIAN_POINT ( 'NONE',  ( 26.07721637849146390, 0.4197350235787081774, -17.11807909718082144 ) ) ;
#25557 = CARTESIAN_POINT ( 'NONE',  ( 22.42023978564754927, -3.655767601918122445, -13.54521809681785172 ) ) ;
#25559 = ORIENTED_EDGE ( 'NONE', *, *, #13930, .T. ) ;
#25558 = CARTESIAN_POINT ( 'NONE',  ( 33.10306327339915811, -12.22190834454405106, -20.64716665866461298 ) ) ;
#25560 = FACE_OUTER_BOUND ( 'NONE', #15196, .T. ) ;
#25561 = AXIS2_PLACEMENT_3D ( 'NONE', #19138, #7844, #26329 ) ;
#25562 = DIRECTION ( 'NONE',  ( 0.9510565162951535312, 2.566386769018988816E-16, -0.3090169943749475623 ) ) ;
#25563 = FACE_OUTER_BOUND ( 'NONE', #17383, .T. ) ;
#25564 = CARTESIAN_POINT ( 'NONE',  ( 15.54217852991911997, 3.796156774867226247, -18.16774540469225485 ) ) ;
#25565 = VERTEX_POINT ( 'NONE', #2066 ) ;
#25566 = DIRECTION ( 'NONE',  ( -0.5877852522924731371, -1.586114251531760728E-16, -0.8090169943749474513 ) ) ;
#25567 = CARTESIAN_POINT ( 'NONE',  ( 10.33811693838771717, 18.38618951776012267, -17.92981046679734547 ) ) ;
#25568 = ORIENTED_EDGE ( 'NONE', *, *, #5718, .T. ) ;
#25569 = DIRECTION ( 'NONE',  ( 0.000000000000000000, 0.000000000000000000, -1.000000000000000000 ) ) ;
#25570 = CARTESIAN_POINT ( 'NONE',  ( 157.0152310637605240, -1.999999999999974021, -15.61832212156129707 ) ) ;
#25571 = CARTESIAN_POINT ( 'NONE',  ( 16.06572049258021195, 3.735912457719189117, -15.00855390560170477 ) ) ;
#25572 = ORIENTED_EDGE ( 'NONE', *, *, #18884, .F. ) ;
#25573 = CARTESIAN_POINT ( 'NONE',  ( 35.28941737075538043, -22.02017293461823755, -20.69856730472309891 ) ) ;
#25574 = ORIENTED_EDGE ( 'NONE', *, *, #27935, .T. ) ;
#25575 = EDGE_CURVE ( 'NONE', #28740, #19419, #22785, .T. ) ;
#25576 = EDGE_CURVE ( 'NONE', #29239, #26232, #2796, .T. ) ;
#25577 = CARTESIAN_POINT ( 'NONE',  ( 23.98539618923253514, -1.204509296099786297, -17.73462021633622143 ) ) ;
#25578 = ADVANCED_FACE ( 'NONE', ( #11196 ), #27879, .T. ) ;
#25579 = CARTESIAN_POINT ( 'NONE',  ( 14.86918570794847305, 4.945381287188965302, -16.48322999939953704 ) ) ;
#25580 = EDGE_CURVE ( 'NONE', #15051, #9036, #20353, .T. ) ;
#25581 = CARTESIAN_POINT ( 'NONE',  ( 20.85427418779519826, -0.3072727129311651484, -13.36207100503020584 ) ) ;
#25582 = VECTOR ( 'NONE', #12560, 999.9999999999998863 ) ;
#25583 = VERTEX_POINT ( 'NONE', #20649 ) ;
#25584 = CARTESIAN_POINT ( 'NONE',  ( -8.000000000000000000, 0.7809653281576059980, -5.000000000000003553 ) ) ;
#25586 = ORIENTED_EDGE ( 'NONE', *, *, #20743, .T. ) ;
#25585 = CARTESIAN_POINT ( 'NONE',  ( 156.1922820468853956, -10.00000000000000000, -22.25671179336496053 ) ) ;
#25587 = ORIENTED_EDGE ( 'NONE', *, *, #1665, .T. ) ;
#25588 = PLANE ( 'NONE',  #28531 ) ;
#25589 = CARTESIAN_POINT ( 'NONE',  ( 134.5152310637605524, -10.00000000000000533, -21.71180489736090991 ) ) ;
#25590 = CARTESIAN_POINT ( 'NONE',  ( 36.14373538984320078, -19.36570096427324827, -19.42526322947885475 ) ) ;
#25591 = CARTESIAN_POINT ( 'NONE',  ( 9.641350810849047548, 17.66889113945805789, -17.94384837343789485 ) ) ;
#25592 = ORIENTED_EDGE ( 'NONE', *, *, #18559, .F. ) ;
#25593 = DIRECTION ( 'NONE',  ( -0.8090169943749474513, -2.183098979609982436E-16, -0.5877852522924731371 ) ) ;
#25594 = CARTESIAN_POINT ( 'NONE',  ( 142.0152310637605808, -4.999999999999979572, -1.576685793744487594E-14 ) ) ;
#25595 = CARTESIAN_POINT ( 'NONE',  ( 10.44197622278032611, 16.58997661396885803, -17.36392598754248695 ) ) ;
#25596 = FACE_OUTER_BOUND ( 'NONE', #19337, .T. ) ;
#25597 = CARTESIAN_POINT ( 'NONE',  ( 132.0152310637605524, -4.999999999999982236, -1.465663491281971624E-14 ) ) ;
#25598 = EDGE_LOOP ( 'NONE', ( #16360, #17368, #8902, #27974 ) ) ;
#25599 = LINE ( 'NONE', #25767, #297 ) ;
#25600 = AXIS2_PLACEMENT_3D ( 'NONE', #28158, #25986, #501 ) ;
#25601 = FACE_OUTER_BOUND ( 'NONE', #14380, .T. ) ;
#25602 = VERTEX_POINT ( 'NONE', #20954 ) ;
#25603 = CARTESIAN_POINT ( 'NONE',  ( 144.5152310637605240, -1.999999999999978018, -4.391296821672111328 ) ) ;
#25604 = ORIENTED_EDGE ( 'NONE', *, *, #26602, .F. ) ;
#25605 = CARTESIAN_POINT ( 'NONE',  ( 9.665905706931651409, 16.23637826941602569, -17.88729680195882565 ) ) ;
#25606 = ORIENTED_EDGE ( 'NONE', *, *, #12719, .F. ) ;
#25607 = ADVANCED_FACE ( 'NONE', ( #4338 ), #30036, .T. ) ;
#25608 = CARTESIAN_POINT ( 'NONE',  ( 23.43490106394649430, 0.5024168867186777909, -19.39616715318824802 ) ) ;
#25609 = CARTESIAN_POINT ( 'NONE',  ( 23.01595892079019379, -1.674233493421072305, -13.97569732891719241 ) ) ;
#25610 = EDGE_CURVE ( 'NONE', #18285, #6891, #18217, .T. ) ;
#25611 = ORIENTED_EDGE ( 'NONE', *, *, #20076, .T. ) ;
#25612 = ADVANCED_FACE ( 'NONE', ( #22814 ), #16229, .T. ) ;
#25613 = CARTESIAN_POINT ( 'NONE',  ( 20.07445496384854877, 6.874260549971754841, -18.87959640166664954 ) ) ;
#25614 = CARTESIAN_POINT ( 'NONE',  ( 162.2287565553229740, -1.999999999999971800, -29.49038105676660493 ) ) ;
#25615 = DIRECTION ( 'NONE',  ( -0.000000000000000000, -0.000000000000000000, -1.000000000000000000 ) ) ;
#25616 = EDGE_CURVE ( 'NONE', #6165, #25166, #8749, .T. ) ;
#25617 = B_SPLINE_CURVE_WITH_KNOTS ( 'NONE', 3,
 ( #9184, #18811, #14219, #13916 ),
 .UNSPECIFIED., .F., .F.,
 ( 4, 4 ),
 ( 2.380737582341341346E-07, 0.002336974151641586783 ),
 .UNSPECIFIED. ) ;
#25618 = DIRECTION ( 'NONE',  ( -2.698458740408365879E-16, 1.000000000000000000, 0.000000000000000000 ) ) ;
#25619 = VECTOR ( 'NONE', #1037, 1000.000000000000000 ) ;
#25620 = CARTESIAN_POINT ( 'NONE',  ( 26.85315702054868936, -3.432285194908070380, -17.01323758698984889 ) ) ;
#25621 = AXIS2_PLACEMENT_3D ( 'NONE', #2725, #28856, #25923 ) ;
#25622 = ORIENTED_EDGE ( 'NONE', *, *, #11914, .T. ) ;
#25623 = PLANE ( 'NONE',  #10544 ) ;
#25624 = LINE ( 'NONE', #11875, #13275 ) ;
#25625 = CARTESIAN_POINT ( 'NONE',  ( 167.0152310637604671, -4.999999999999971578, -6.958068083716895558 ) ) ;
#25626 = AXIS2_PLACEMENT_3D ( 'NONE', #398, #14408, #28052 ) ;
#25627 = CARTESIAN_POINT ( 'NONE',  ( 2.100000000000002753, 9.325873406851319278E-16, 1.700000000000000178 ) ) ;
#25629 = CARTESIAN_POINT ( 'NONE',  ( 2.000000000000008882, -3.464101615137750390, -2.450000000000000622 ) ) ;
#25628 = AXIS2_PLACEMENT_3D ( 'NONE', #14251, #20671, #25273 ) ;
#25630 = CARTESIAN_POINT ( 'NONE',  ( 10.35864919664826900, 16.97212497753646687, -17.91558149794984445 ) ) ;
#25631 = DIRECTION ( 'NONE',  ( -0.8090169943749474513, -2.183098979609982436E-16, 0.5877852522924731371 ) ) ;
#25632 = CARTESIAN_POINT ( 'NONE',  ( 33.38708106686501509, -12.47399286361455850, -19.70456970583452616 ) ) ;
#25633 = VECTOR ( 'NONE', #6949, 1000.000000000000000 ) ;
#25634 = EDGE_LOOP ( 'NONE', ( #24610, #11305, #29338, #24603 ) ) ;
#25635 = CARTESIAN_POINT ( 'NONE',  ( 11.22408442728515077, 9.090372555205103566, -17.24152585048573982 ) ) ;
#25636 = VERTEX_POINT ( 'NONE', #25253 ) ;
#25637 = DIRECTION ( 'NONE',  ( 6.938893903907227392E-16, -0.000000000000000000, 1.000000000000000000 ) ) ;
#25638 = CARTESIAN_POINT ( 'NONE',  ( 20.52488529563827058, 3.974637744936419637, -19.97762432673833288 ) ) ;
#25639 = CARTESIAN_POINT ( 'NONE',  ( 11.27588265011317326, 16.67833209609329259, -16.78465339804365541 ) ) ;
#25640 = LINE ( 'NONE', #26106, #9705 ) ;
#25641 = ORIENTED_EDGE ( 'NONE', *, *, #22874, .T. ) ;
#25642 = ORIENTED_EDGE ( 'NONE', *, *, #10268, .F. ) ;
#25643 = CARTESIAN_POINT ( 'NONE',  ( 9.915248083523094280, 16.41276333319327918, -16.50506225043874409 ) ) ;
#25644 = DIRECTION ( 'NONE',  ( -2.698458740408365879E-16, 1.000000000000000000, 0.000000000000000000 ) ) ;
#25645 = VECTOR ( 'NONE', #24534, 1000.000000000000000 ) ;
#25646 = CARTESIAN_POINT ( 'NONE',  ( 9.916775705961365261, 16.40575746196480011, -16.50441451066904364 ) ) ;
#25647 = DIRECTION ( 'NONE',  ( -0.5877852522924731371, 0.000000000000000000, 0.8090169943749474513 ) ) ;
#25648 = CARTESIAN_POINT ( 'NONE',  ( 149.7287565553229740, -1.999999999999976241, -7.839745962155603820 ) ) ;
#25649 = ORIENTED_EDGE ( 'NONE', *, *, #14236, .F. ) ;
#25650 = CARTESIAN_POINT ( 'NONE',  ( -3.344563996438228770, -2.687817229851498180, -0.1586754815285055242 ) ) ;
#25651 = ORIENTED_EDGE ( 'NONE', *, *, #2557, .T. ) ;
#25652 = CARTESIAN_POINT ( 'NONE',  ( 10.50441255335269020, 16.30363564318377811, -17.32140922184415288 ) ) ;
#25653 = ORIENTED_EDGE ( 'NONE', *, *, #20077, .F. ) ;
#25655 = CARTESIAN_POINT ( 'NONE',  ( 36.48591233058812833, -21.90292070287360460, -19.44112467175505898 ) ) ;
#25654 = VECTOR ( 'NONE', #17418, 1000.000000000000000 ) ;
#25656 = CARTESIAN_POINT ( 'NONE',  ( 24.14317479683219858, -6.286850201977149055, -18.60698471650063723 ) ) ;
#25657 = ORIENTED_EDGE ( 'NONE', *, *, #16829, .F. ) ;
#25658 = EDGE_CURVE ( 'NONE', #14105, #22950, #13338, .T. ) ;
#25659 = VECTOR ( 'NONE', #1446, 1000.000000000000000 ) ;
#25660 = DIRECTION ( 'NONE',  ( -1.226925503391459091E-16, 1.000000000000000000, 0.000000000000000000 ) ) ;
#25661 = ADVANCED_FACE ( 'NONE', ( #16072 ), #22661, .T. ) ;
#25662 = EDGE_CURVE ( 'NONE', #18003, #23706, #18068, .T. ) ;
#25663 = ADVANCED_FACE ( 'NONE', ( #30186 ), #9196, .T. ) ;
#25664 = CARTESIAN_POINT ( 'NONE',  ( 167.0152310637605524, -9.999999999999996447, -32.93883019725009120 ) ) ;
#25665 = DIRECTION ( 'NONE',  ( 1.000000000000000000, 0.000000000000000000, 0.000000000000000000 ) ) ;
#25666 = CARTESIAN_POINT ( 'NONE',  ( 18.18682981270212196, 6.389142113859191952, -14.72334701657588063 ) ) ;
#25667 = CARTESIAN_POINT ( 'NONE',  ( 29.41685937463160272, -8.713933360145817986, -16.19581194183416883 ) ) ;
#25668 = ORIENTED_EDGE ( 'NONE', *, *, #29210, .T. ) ;
#25669 = CARTESIAN_POINT ( 'NONE',  ( 148.6922820468853956, -1.999999999999976685, -6.413161187712876909 ) ) ;
#25670 = VECTOR ( 'NONE', #22165, 1000.000000000000000 ) ;
#25671 = EDGE_LOOP ( 'NONE', ( #22595, #14924, #25245, #4944, #27923, #10322 ) ) ;
#25672 = DIRECTION ( 'NONE',  ( -1.110223024625156540E-16, 0.000000000000000000, -1.000000000000000000 ) ) ;
#25673 = CARTESIAN_POINT ( 'NONE',  ( 151.1922820468853672, -10.00000000000000178, -2.083034168790677043 ) ) ;
#25674 = VECTOR ( 'NONE', #4450, 1000.000000000000000 ) ;
#25675 = LINE ( 'NONE', #23090, #1221 ) ;
#25676 = AXIS2_PLACEMENT_3D ( 'NONE', #4027, #13322, #22502 ) ;
#25677 = PRODUCT_DEFINITION_CONTEXT ( 'detailed design', #13390, 'design' ) ;
#25678 = CARTESIAN_POINT ( 'NONE',  ( 10.72061166913284325, 16.63201992582523658, -15.95427402900266856 ) ) ;
#25679 = CARTESIAN_POINT ( 'NONE',  ( 152.0152310637604955, -4.999999999999976907, -15.61832212156129351 ) ) ;
#25680 = ORIENTED_EDGE ( 'NONE', *, *, #4274, .T. ) ;
#25681 = AXIS2_PLACEMENT_3D ( 'NONE', #10870, #22489, #27257 ) ;
#25682 = LINE ( 'NONE', #2800, #6188 ) ;
#25683 = ORIENTED_EDGE ( 'NONE', *, *, #9126, .F. ) ;
#25684 = CARTESIAN_POINT ( 'NONE',  ( 11.47288049726737214, 9.269262779257836371, -15.86091052746238184 ) ) ;
#25685 = ORIENTED_EDGE ( 'NONE', *, *, #24665, .T. ) ;
#25686 = CARTESIAN_POINT ( 'NONE',  ( 15.10317701704014226, 5.923596928851710075, -17.67988701311836053 ) ) ;
#25687 = LINE ( 'NONE', #7225, #23925 ) ;
#25688 = DIRECTION ( 'NONE',  ( -2.698458740408365879E-16, 1.000000000000000000, 0.000000000000000000 ) ) ;
#25689 = CARTESIAN_POINT ( 'NONE',  ( 27.89048517759004753, -11.43816616845083445, -12.79876095355805177 ) ) ;
#25690 = ORIENTED_EDGE ( 'NONE', *, *, #21767, .T. ) ;
#25691 = DIRECTION ( 'NONE',  ( 0.000000000000000000, 2.775557561562890735E-17, -1.000000000000000000 ) ) ;
#25692 = CARTESIAN_POINT ( 'NONE',  ( 11.27636807789780171, 16.67610586239533177, -16.78445215232725118 ) ) ;
#25693 = CARTESIAN_POINT ( 'NONE',  ( 35.26536834604049631, -19.91213340569504808, -19.23001471935974038 ) ) ;
#25694 = CARTESIAN_POINT ( 'NONE',  ( 162.0152310637604387, -1.999999999999973577, 1.702185954127501066 ) ) ;
#25695 = ORIENTED_EDGE ( 'NONE', *, *, #9505, .T. ) ;
#25696 = ORIENTED_EDGE ( 'NONE', *, *, #17850, .F. ) ;
#25697 = EDGE_CURVE ( 'NONE', #7245, #17600, #23561, .T. ) ;
#25698 = DIRECTION ( 'NONE',  ( 0.5877852522924731371, 0.000000000000000000, 0.8090169943749474513 ) ) ;
#25699 = CARTESIAN_POINT ( 'NONE',  ( 23.53678897557974281, -9.624609092408482169, -17.82855203159936863 ) ) ;
#25700 = ADVANCED_FACE ( 'NONE', ( #7389 ), #14681, .T. ) ;
#25701 = ORIENTED_EDGE ( 'NONE', *, *, #14473, .T. ) ;
#25702 = EDGE_CURVE ( 'NONE', #10712, #18131, #376, .T. ) ;
#25703 = DIRECTION ( 'NONE',  ( 0.9510565162951536422, 2.566386769018988816E-16, 0.3090169943749472292 ) ) ;
#25704 = ORIENTED_EDGE ( 'NONE', *, *, #30047, .T. ) ;
#25705 = FILL_AREA_STYLE_COLOUR ( '', #29861 ) ;
#25706 = CARTESIAN_POINT ( 'NONE',  ( 22.98323032518889519, 2.094654362561221284, -17.51695658672324640 ) ) ;
#25707 = VECTOR ( 'NONE', #15316, 1000.000000000000000 ) ;
#25708 = CARTESIAN_POINT ( 'NONE',  ( 16.16754939756797782, 8.873905313537072459, -14.69432754670026142 ) ) ;
#25709 = ORIENTED_EDGE ( 'NONE', *, *, #11445, .T. ) ;
#25710 = EDGE_LOOP ( 'NONE', ( #20448, #18765, #13730, #17376 ) ) ;
#25711 = DIRECTION ( 'NONE',  ( 1.000000000000000000, 0.000000000000000000, 0.000000000000000000 ) ) ;
#25712 = CARTESIAN_POINT ( 'NONE',  ( 133.6922820468854241, -1.999999999999980904, -32.39392330124607611 ) ) ;
#25713 = ORIENTED_EDGE ( 'NONE', *, *, #16918, .T. ) ;
#25714 = CARTESIAN_POINT ( 'NONE',  ( 144.7287565553230024, -10.00000000000000355, -7.839745962155603820 ) ) ;
#25715 = LINE ( 'NONE', #23425, #12703 ) ;
#25716 = ORIENTED_EDGE ( 'NONE', *, *, #28491, .F. ) ;
#25717 = LINE ( 'NONE', #4800, #26063 ) ;
#25718 = AXIS2_PLACEMENT_3D ( 'NONE', #25171, #8376, #22269 ) ;
#25719 = CARTESIAN_POINT ( 'NONE',  ( 9.642214727206800617, 17.66492910891761525, -17.80644250212319690 ) ) ;
#25720 = CARTESIAN_POINT ( 'NONE',  ( 23.72497280669020014, -7.722717790116627512, -18.49470058199314693 ) ) ;
#25721 = CARTESIAN_POINT ( 'NONE',  ( 23.07678757892180244, -0.1267571646896241688, -14.23703129728563965 ) ) ;
#25722 = ADVANCED_FACE ( 'NONE', ( #26161 ), #2972, .T. ) ;
#25724 = ORIENTED_EDGE ( 'NONE', *, *, #7439, .F. ) ;
#25723 = CARTESIAN_POINT ( 'NONE',  ( 32.11502935538656800, -10.34531343835429062, -18.85863636141847621 ) ) ;
#25725 = CIRCLE ( 'NONE', #392, 4.000000000000003553 ) ;
#25726 = CARTESIAN_POINT ( 'NONE',  ( 12.56861602585598980, 8.601024833420110483, -15.07548682890769243 ) ) ;
#25727 = CARTESIAN_POINT ( 'NONE',  ( 174.7287565553229456, -9.999999999999994671, -33.82050807568879947 ) ) ;
#25728 = CARTESIAN_POINT ( 'NONE',  ( 2.500000000000000444, 0.000000000000000000, -2.041999999999998483 ) ) ;
#25729 = CARTESIAN_POINT ( 'NONE',  ( 17.63704213852533442, 9.806822523219006271, -18.50018230520716145 ) ) ;
#25730 = VERTEX_POINT ( 'NONE', #2815 ) ;
#25731 = CARTESIAN_POINT ( 'NONE',  ( 133.7287565553229456, -9.999999999999982236, 3.500000000000003109 ) ) ;
#25732 = CARTESIAN_POINT ( 'NONE',  ( 10.33811811146757265, 18.38618413786636552, -17.91101973220562371 ) ) ;
#25733 = ORIENTED_EDGE ( 'NONE', *, *, #16900, .F. ) ;
#25734 = CARTESIAN_POINT ( 'NONE',  ( 167.0152310637604387, -1.999999999999972244, 1.702185954127501066 ) ) ;
#25735 = PLANE ( 'NONE',  #7868 ) ;
#25736 = CARTESIAN_POINT ( 'NONE',  ( 17.21692058948253035, 4.245457944912791604, -14.13226496128363863 ) ) ;
#25737 = CARTESIAN_POINT ( 'NONE',  ( 13.18850634723077242, 6.203946520731500769, -19.20132247218941401 ) ) ;
#25738 = ADVANCED_FACE ( 'NONE', ( #12395 ), #23872, .T. ) ;
#25739 = ORIENTED_EDGE ( 'NONE', *, *, #16517, .T. ) ;
#25740 = CARTESIAN_POINT ( 'NONE',  ( 33.13932541451587355, -12.36573032794433047, -20.66922553108291538 ) ) ;
#25741 = CARTESIAN_POINT ( 'NONE',  ( 20.63450008290067927, -1.653576198284400833, -18.07233451455898532 ) ) ;
#25742 = CARTESIAN_POINT ( 'NONE',  ( 20.64697163712990857, 4.580154932681155699, -17.29389188279686707 ) ) ;
#25743 = VECTOR ( 'NONE', #19391, 1000.000000000000114 ) ;
#25744 = VERTEX_POINT ( 'NONE', #3122 ) ;
#25745 = CARTESIAN_POINT ( 'NONE',  ( 28.34689840388910653, -5.967659833748593101, -13.48819167749268644 ) ) ;
#25746 = CIRCLE ( 'NONE', #29707, 49.99999999999998579 ) ;
#25747 = ORIENTED_EDGE ( 'NONE', *, *, #8829, .T. ) ;
#25748 = LINE ( 'NONE', #11690, #10856 ) ;
#25749 = AXIS2_PLACEMENT_3D ( 'NONE', #6574, #25341, #18614 ) ;
#25750 = DIRECTION ( 'NONE',  ( 1.000000000000000000, 2.698458740408365879E-16, -1.110223024625156540E-16 ) ) ;
#25751 = VERTEX_POINT ( 'NONE', #16376 ) ;
#25752 = CARTESIAN_POINT ( 'NONE',  ( 158.6922820468853672, -10.00000000000000000, -15.07341522555727664 ) ) ;
#25753 = CARTESIAN_POINT ( 'NONE',  ( 0.000000000000000000, -1.178949249685215417, 2.042000000000002036 ) ) ;
#25754 = EDGE_CURVE ( 'NONE', #3594, #18808, #2660, .T. ) ;
#25755 = CARTESIAN_POINT ( 'NONE',  ( 36.27242973171742335, -19.94385647102418702, -19.46417027601260230 ) ) ;
#25756 = CARTESIAN_POINT ( 'NONE',  ( 9.641350810849047548, 17.66889113945805789, -21.33333333332589277 ) ) ;
#25757 = EDGE_CURVE ( 'NONE', #10926, #26594, #21112, .T. ) ;
#25758 = ORIENTED_EDGE ( 'NONE', *, *, #16701, .T. ) ;
#25759 = CIRCLE ( 'NONE', #11603, 2.100000000000002753 ) ;
#25760 = DIRECTION ( 'NONE',  ( -0.9510565162951536422, 0.000000000000000000, -0.3090169943749472292 ) ) ;
#25761 = FACE_OUTER_BOUND ( 'NONE', #799, .T. ) ;
#25762 = CARTESIAN_POINT ( 'NONE',  ( 10.47249985125707106, 16.44999136291752251, -17.33460624675630513 ) ) ;
#25763 = CARTESIAN_POINT ( 'NONE',  ( 133.6922820468854241, -4.999999999999981348, 2.247092850131519715 ) ) ;
#25764 = CARTESIAN_POINT ( 'NONE',  ( 143.6922820468854525, -4.999999999999978684, -26.58683881228715506 ) ) ;
#25765 = ORIENTED_EDGE ( 'NONE', *, *, #14205, .T. ) ;
#25766 = CIRCLE ( 'NONE', #19430, 2.500000000000002665 ) ;
#25767 = CARTESIAN_POINT ( 'NONE',  ( 123.4761516755868627, -4.999999999999984901, -89.71067538675424657 ) ) ;
#25768 = FACE_OUTER_BOUND ( 'NONE', #26559, .T. ) ;
#25769 = ORIENTED_EDGE ( 'NONE', *, *, #101, .T. ) ;
#25770 = ORIENTED_EDGE ( 'NONE', *, *, #24594, .T. ) ;
#25771 = CARTESIAN_POINT ( 'NONE',  ( 176.1922820468852535, -1.999999999999969358, -2.083034168790677931 ) ) ;
#25772 = EDGE_LOOP ( 'NONE', ( #25356, #12947, #15906, #15224 ) ) ;
#25773 = CARTESIAN_POINT ( 'NONE',  ( 9.662070302079424522, 16.25396792496884046, -17.90822120357413638 ) ) ;
#25774 = VERTEX_POINT ( 'NONE', #5087 ) ;
#25775 = AXIS2_PLACEMENT_3D ( 'NONE', #11578, #25631, #4721 ) ;
#25776 = CARTESIAN_POINT ( 'NONE',  ( 23.95332181684718975, -6.025008234661991757, -14.41687206698971124 ) ) ;
#25777 = CARTESIAN_POINT ( 'NONE',  ( 20.41927524488895429, 4.553956414902842198, -14.69105443414393264 ) ) ;
#25778 = CARTESIAN_POINT ( 'NONE',  ( 174.5152310637604103, -1.999999999999969580, -13.05155085951651195 ) ) ;
#25779 = CARTESIAN_POINT ( 'NONE',  ( 4.396394917579590889, -5.000000000000016875, 13.53071226075565470 ) ) ;
#25780 = DIRECTION ( 'NONE',  ( -1.110223024625156540E-16, 0.000000000000000000, -1.000000000000000000 ) ) ;
#25781 = CARTESIAN_POINT ( 'NONE',  ( 24.18219217278060995, -6.970120066757704791, -14.18070892486464629 ) ) ;
#25782 = ORIENTED_EDGE ( 'NONE', *, *, #18382, .T. ) ;
#25783 = CARTESIAN_POINT ( 'NONE',  ( 147.0152310637604955, -10.00000000000000355, -0.06116980274991495881 ) ) ;
#25784 = DIRECTION ( 'NONE',  ( -2.698458740408365879E-16, 1.000000000000000000, 0.000000000000000000 ) ) ;
#25785 = VECTOR ( 'NONE', #10427, 1000.000000000000000 ) ;
#25786 =( LENGTH_UNIT ( ) NAMED_UNIT ( * ) SI_UNIT ( .MILLI., .METRE. ) );
#25787 = DIRECTION ( 'NONE',  ( 1.110223024625156540E-16, 2.995891024602366092E-32, 1.000000000000000000 ) ) ;
#25788 = DIRECTION ( 'NONE',  ( -2.698458740408365879E-16, 1.000000000000000000, 0.000000000000000000 ) ) ;
#25789 = VECTOR ( 'NONE', #2455, 1000.000000000000000 ) ;
#25790 = CARTESIAN_POINT ( 'NONE',  ( 10.47184394332236224, 16.45299944031493311, -17.33487789703667303 ) ) ;
#25791 = ADVANCED_FACE ( 'NONE', ( #9497 ), #4936, .T. ) ;
#25792 = DIRECTION ( 'NONE',  ( -0.5877852522924731371, -1.586114251531760235E-16, 0.8090169943749474513 ) ) ;
#25793 = CARTESIAN_POINT ( 'NONE',  ( 33.10952763335142635, -11.62914684427059697, -19.38687730282833499 ) ) ;
#25794 = VERTEX_POINT ( 'NONE', #14529 ) ;
#25795 = CARTESIAN_POINT ( 'NONE',  ( 8.944584683310379702, 16.95159276115599667, -21.33333333332589632 ) ) ;
#25796 = ADVANCED_FACE ( 'NONE', ( #28023 ), #9656, .T. ) ;
#25797 = FACE_OUTER_BOUND ( 'NONE', #14576, .T. ) ;
#25798 = ADVANCED_FACE ( 'NONE', ( #19265 ), #9349, .T. ) ;
#25799 = CARTESIAN_POINT ( 'NONE',  ( 20.72626264887238534, -1.914771856900582714, -13.62749948506543518 ) ) ;
#25800 = CARTESIAN_POINT ( 'NONE',  ( 11.26867954870061439, 16.71136643735313143, -16.78814161468471156 ) ) ;
#25801 = FACE_OUTER_BOUND ( 'NONE', #29429, .T. ) ;
#25802 = VERTEX_POINT ( 'NONE', #5394 ) ;
#25803 = ORIENTED_EDGE ( 'NONE', *, *, #25489, .F. ) ;
#25804 = CARTESIAN_POINT ( 'NONE',  ( 9.641350944112486943, 17.66889052829492002, -17.91441860517739215 ) ) ;
#25805 = CARTESIAN_POINT ( 'NONE',  ( 153.6922820468853388, -10.00000000000000178, 2.247092850131519715 ) ) ;
#25806 = CARTESIAN_POINT ( 'NONE',  ( 11.34314632229486364, 9.864239995495806212, -15.91456019135469013 ) ) ;
#25807 = DIRECTION ( 'NONE',  ( -1.110223024625156540E-16, 0.000000000000000000, -1.000000000000000000 ) ) ;
#25808 = CARTESIAN_POINT ( 'NONE',  ( 0.6554360035617690095, -4.240386000424094526, -2.291324518471481220 ) ) ;
#25809 = ORIENTED_EDGE ( 'NONE', *, *, #24563, .F. ) ;
#25810 = DIRECTION ( 'NONE',  ( -2.698458740408365879E-16, 1.000000000000000000, 0.000000000000000000 ) ) ;
#25811 = VERTEX_POINT ( 'NONE', #14227 ) ;
#25812 = CARTESIAN_POINT ( 'NONE',  ( 10.79618582965528439, 14.96552620561766567, -17.20075070836251996 ) ) ;
#25813 = EDGE_LOOP ( 'NONE', ( #7630, #1256, #7814, #22149 ) ) ;
#25814 = VECTOR ( 'NONE', #23385, 1000.000000000000000 ) ;
#25815 = CARTESIAN_POINT ( 'NONE',  ( 36.07559364978101968, -20.05957622185551870, -20.44697815928661200 ) ) ;
#25816 = CARTESIAN_POINT ( 'NONE',  ( 14.78952226657687063, 10.37904477376192069, -15.12939866669752575 ) ) ;
#25817 = CARTESIAN_POINT ( 'NONE',  ( 27.95388715220626707, -5.541385876428546631, -15.41148221666858831 ) ) ;
#25818 = LINE ( 'NONE', #21222, #28204 ) ;
#25819 = EDGE_LOOP ( 'NONE', ( #16986, #29676, #27157, #3728 ) ) ;
#25820 =( GEOMETRIC_REPRESENTATION_CONTEXT ( 3 ) GLOBAL_UNCERTAINTY_ASSIGNED_CONTEXT ( ( #7366 ) ) GLOBAL_UNIT_ASSIGNED_CONTEXT ( ( #25150, #22715, #1516 ) ) REPRESENTATION_CONTEXT ( 'NONE', 'WORKASPACE' ) );
#25821 = DIRECTION ( 'NONE',  ( 0.5877852522924731371, 0.000000000000000000, 0.8090169943749474513 ) ) ;
#25822 = CARTESIAN_POINT ( 'NONE',  ( -20.00000000000017053, 34.64101615137744972, 15.00000000000000000 ) ) ;
#25823 = CARTESIAN_POINT ( 'NONE',  ( 17.40794641162625567, 9.636182090832996039, -14.27881468665684395 ) ) ;
#25824 = CARTESIAN_POINT ( 'NONE',  ( 14.03850921439652311, 8.975161913830900673, -15.18271992443145635 ) ) ;
#25825 = ORIENTED_EDGE ( 'NONE', *, *, #26824, .T. ) ;
#25826 = DIRECTION ( 'NONE',  ( -0.8090169943749474513, -2.183098979609982436E-16, 0.5877852522924731371 ) ) ;
#25827 = DIRECTION ( 'NONE',  ( -2.698458740408365879E-16, 1.000000000000000000, 0.000000000000000000 ) ) ;
#25828 = EDGE_CURVE ( 'NONE', #6258, #5247, #16534, .T. ) ;
#25829 = CARTESIAN_POINT ( 'NONE',  ( 131.1922820468854241, -10.00000000000000888, -22.25671179336495697 ) ) ;
#25830 = VECTOR ( 'NONE', #19073, 999.9999999999998863 ) ;
#25831 = DIRECTION ( 'NONE',  ( -2.698458740408365879E-16, 1.000000000000000000, 0.000000000000000000 ) ) ;
#25832 = EDGE_CURVE ( 'NONE', #30106, #5942, #25858, .T. ) ;
#25833 = DIRECTION ( 'NONE',  ( -2.698458740408365879E-16, 1.000000000000000000, 0.000000000000000000 ) ) ;
#25834 = EDGE_CURVE ( 'NONE', #3555, #14905, #18977, .T. ) ;
#25835 = EDGE_CURVE ( 'NONE', #6518, #24599, #14375, .T. ) ;
#25836 = VECTOR ( 'NONE', #20258, 1000.000000000000000 ) ;
#25837 = CARTESIAN_POINT ( 'NONE',  ( 10.71880336532874445, 16.64031303757595026, -15.95504377300109944 ) ) ;
#25838 = VECTOR ( 'NONE', #23929, 1000.000000000000000 ) ;
#25839 = EDGE_CURVE ( 'NONE', #9877, #7345, #9809, .T. ) ;
#25840 = LINE ( 'NONE', #26141, #29019 ) ;
#25841 = EDGE_LOOP ( 'NONE', ( #4677, #15994, #22574, #4200 ) ) ;
#25842 = CARTESIAN_POINT ( 'NONE',  ( 0.000000000000000000, 0.000000000000000000, 4.999999999999998224 ) ) ;
#25843 = ORIENTED_EDGE ( 'NONE', *, *, #25834, .T. ) ;
#25844 = CARTESIAN_POINT ( 'NONE',  ( 10.95411528722473626, 11.64838591225006859, -16.07543820933196699 ) ) ;
#25845 = ORIENTED_EDGE ( 'NONE', *, *, #20621, .T. ) ;
#25846 = CARTESIAN_POINT ( 'NONE',  ( 9.665905706931651409, 16.23637826941602569, -17.88729680195882565 ) ) ;
#25847 = CARTESIAN_POINT ( 'NONE',  ( 16.58324305800299925, 4.586402732284541095, -18.38077023430394163 ) ) ;
#25848 = DIRECTION ( 'NONE',  ( -0.5877852522924731371, -1.586114251531760235E-16, 0.8090169943749474513 ) ) ;
#25849 = DIRECTION ( 'NONE',  ( -2.698458740408365879E-16, 1.000000000000000000, 0.000000000000000000 ) ) ;
#25850 = CARTESIAN_POINT ( 'NONE',  ( 27.91615220763155847, -6.225400021157185826, -17.67258836524805332 ) ) ;
#25851 = EDGE_LOOP ( 'NONE', ( #24506, #9418, #2958, #7747 ) ) ;
#25852 = DIRECTION ( 'NONE',  ( -0.5877852522924731371, 0.000000000000000000, 0.8090169943749474513 ) ) ;
#25853 = CARTESIAN_POINT ( 'NONE',  ( 11.05542208158282769, 17.68939236555957706, -17.90700183802944778 ) ) ;
#25854 = ORIENTED_EDGE ( 'NONE', *, *, #24663, .F. ) ;
#25856 = VECTOR ( 'NONE', #13181, 1000.000000000000000 ) ;
#25855 = CARTESIAN_POINT ( 'NONE',  ( 34.76605987604303749, -17.66900494105776787, -19.07908574721388462 ) ) ;
#25857 = FACE_OUTER_BOUND ( 'NONE', #20610, .T. ) ;
#25858 = LINE ( 'NONE', #7081, #5243 ) ;
#25859 = CARTESIAN_POINT ( 'NONE',  ( 23.66316133457650750, -10.02594615916883392, -14.11990577516520595 ) ) ;
#25860 = VERTEX_POINT ( 'NONE', #5991 ) ;
#25861 = DIRECTION ( 'NONE',  ( 1.000000000000000000, 0.000000000000000000, 0.000000000000000000 ) ) ;
#25862 = AXIS2_PLACEMENT_3D ( 'NONE', #10466, #21926, #1041 ) ;
#25863 = CARTESIAN_POINT ( 'NONE',  ( 16.05281274719596496, 2.901206577426825639, -17.92093306952238407 ) ) ;
#25864 = CARTESIAN_POINT ( 'NONE',  ( 16.85369750842388825, 4.841181898090542113, -18.70119709635011418 ) ) ;
#25865 = ORIENTED_EDGE ( 'NONE', *, *, #13208, .T. ) ;
#25866 = VERTEX_POINT ( 'NONE', #24461 ) ;
#25867 = LINE ( 'NONE', #7838, #17152 ) ;
#25868 = DIRECTION ( 'NONE',  ( -2.698458740408365879E-16, 1.000000000000000000, 0.000000000000000000 ) ) ;
#25869 = VECTOR ( 'NONE', #5309, 1000.000000000000000 ) ;
#25870 = CARTESIAN_POINT ( 'NONE',  ( 0.000000000000000000, 0.000000000000000000, 0.000000000000000000 ) ) ;
#25871 = DIRECTION ( 'NONE',  ( -2.698458740408365879E-16, 1.000000000000000000, -0.000000000000000000 ) ) ;
#25872 = VECTOR ( 'NONE', #14031, 1000.000000000000000 ) ;
#25873 = ADVANCED_FACE ( 'NONE', ( #28785 ), #10713, .T. ) ;
#25874 = CARTESIAN_POINT ( 'NONE',  ( 4.250000000000000000, 1.887379141862764541E-15, -4.449444346342715129 ) ) ;
#25875 = EDGE_CURVE ( 'NONE', #888, #10558, #29081, .T. ) ;
#25876 = CARTESIAN_POINT ( 'NONE',  ( 9.914377700407460026, 16.41675502110963336, -16.50544604630902867 ) ) ;
#25877 = EDGE_CURVE ( 'NONE', #29393, #24131, #5547, .T. ) ;
#25878 = CARTESIAN_POINT ( 'NONE',  ( 22.63726333831294468, -4.877931240889711972, -12.86144741616201870 ) ) ;
#25879 = CARTESIAN_POINT ( 'NONE',  ( 22.47820520476076567, 2.340993144345510313, -15.49451772223075707 ) ) ;
#25881 = EDGE_LOOP ( 'NONE', ( #8372, #12956, #1543, #161 ) ) ;
#25880 = CARTESIAN_POINT ( 'NONE',  ( 33.31547190024930671, -13.15228156363260581, -20.72525089784059560 ) ) ;
#25883 = CARTESIAN_POINT ( 'NONE',  ( 144.5152310637605808, -4.999999999999978684, -30.37205893520530964 ) ) ;
#25882 =( GEOMETRIC_REPRESENTATION_CONTEXT ( 3 ) GLOBAL_UNCERTAINTY_ASSIGNED_CONTEXT ( ( #11026 ) ) GLOBAL_UNIT_ASSIGNED_CONTEXT ( ( #26354, #28977, #24208 ) ) REPRESENTATION_CONTEXT ( 'NONE', 'WORKASPACE' ) );
#25884 = CARTESIAN_POINT ( 'NONE',  ( 12.51417009928267099, 8.576964204390579383, -15.11888119342340353 ) ) ;
#25885 = CARTESIAN_POINT ( 'NONE',  ( 156.1922820468853388, -10.00000000000000178, -2.083034168790677043 ) ) ;
#25886 = LINE ( 'NONE', #14254, #25367 ) ;
#25887 = CARTESIAN_POINT ( 'NONE',  ( 19.11618317516819587, 7.271703427217982352, -19.10559232466456692 ) ) ;
#25888 = LINE ( 'NONE', #18705, #21727 ) ;
#25889 = CARTESIAN_POINT ( 'NONE',  ( 10.72183334705107960, 16.62641715516447150, -15.95376865854981929 ) ) ;
#25890 = B_SPLINE_CURVE_WITH_KNOTS ( 'NONE', 3,
 ( #10752, #29584, #6331, #8454, #1916, #20504 ),
 .UNSPECIFIED., .F., .F.,
 ( 4, 2, 4 ),
 ( 0.004120275011746851387, 0.005288420935197119671, 0.006456566858647387087 ),
 .UNSPECIFIED. ) ;
#25891 = VERTEX_POINT ( 'NONE', #13002 ) ;
#25892 = DIRECTION ( 'NONE',  ( -2.698458740408366372E-16, 1.000000000000000000, 0.000000000000000000 ) ) ;
#25893 = DIRECTION ( 'NONE',  ( -2.698458740408365879E-16, 1.000000000000000000, 0.000000000000000000 ) ) ;
#25894 = CARTESIAN_POINT ( 'NONE',  ( 16.89609864265585060, 4.102175112930991574, -14.31125941877678720 ) ) ;
#25895 = ORIENTED_EDGE ( 'NONE', *, *, #4949, .F. ) ;
#25896 = CARTESIAN_POINT ( 'NONE',  ( 13.03988341252192917, 6.056598437983586436, -18.79510648546616736 ) ) ;
#25897 = ORIENTED_EDGE ( 'NONE', *, *, #29447, .T. ) ;
#25899 = AXIS2_PLACEMENT_3D ( 'NONE', #13665, #8631, #25275 ) ;
#25898 = CARTESIAN_POINT ( 'NONE',  ( 32.62126879184269512, -11.04717877266006987, -18.30218954475424908 ) ) ;
#25900 = CARTESIAN_POINT ( 'NONE',  ( 23.56326861202678202, -1.685860805813322427, -18.23406631578895798 ) ) ;
#25901 = AXIS2_PLACEMENT_3D ( 'NONE', #4489, #26006, #7078 ) ;
#25902 = CARTESIAN_POINT ( 'NONE',  ( 18.96452888794134495, 2.710274068595869057, -18.82741851907772457 ) ) ;
#25903 = CARTESIAN_POINT ( 'NONE',  ( 28.79879967665997142, -10.96283228269853893, -18.01937015232834938 ) ) ;
#25904 = COLOUR_RGB ( '', 0.08235294, 0.09019608, 0.10196078) ;
#25905 = ORIENTED_EDGE ( 'NONE', *, *, #27551, .F. ) ;
#25906 = LINE ( 'NONE', #14276, #9893 ) ;
#25907 = VERTEX_POINT ( 'NONE', #6143 ) ;
#25908 = FACE_OUTER_BOUND ( 'NONE', #1193, .T. ) ;
#25909 = ORIENTED_EDGE ( 'NONE', *, *, #20077, .T. ) ;
#25910 = DIRECTION ( 'NONE',  ( 0.9510565162951536422, 2.566386769018988816E-16, 0.3090169943749472292 ) ) ;
#25911 = ADVANCED_FACE ( 'NONE', ( #14828 ), #26464, .T. ) ;
#25912 = FACE_BOUND ( 'NONE', #1187, .T. ) ;
#25913 = CARTESIAN_POINT ( 'NONE',  ( 36.36958547251401797, -20.38032574959806098, -19.43068663056894252 ) ) ;
#25914 = VECTOR ( 'NONE', #13844, 1000.000000000000000 ) ;
#25915 = CARTESIAN_POINT ( 'NONE',  ( 9.641351338355821810, 17.66888872024471624, -17.91303689663363130 ) ) ;
#25916 = EDGE_LOOP ( 'NONE', ( #3809, #14037, #9302, #12585 ) ) ;
#25917 = DIRECTION ( 'NONE',  ( 1.000000000000000000, -1.332267629550188046E-15, 0.000000000000000000 ) ) ;
#25918 = LINE ( 'NONE', #7735, #24624 ) ;
#25919 = CARTESIAN_POINT ( 'NONE',  ( 12.07790154976966868, 9.144051220271959934, -16.66639656463015839 ) ) ;
#25920 = DIRECTION ( 'NONE',  ( 0.000000000000000000, 0.000000000000000000, 1.000000000000000000 ) ) ;
#25921 = CARTESIAN_POINT ( 'NONE',  ( 4.000000000000003553, 2.309401076758525573, -2.092734410091829034 ) ) ;
#25922 = ORIENTED_EDGE ( 'NONE', *, *, #4980, .T. ) ;
#25923 = DIRECTION ( 'NONE',  ( 0.5877852522924731371, 0.000000000000000000, 0.8090169943749474513 ) ) ;
#25924 = LINE ( 'NONE', #9416, #26872 ) ;
#25925 = ORIENTED_EDGE ( 'NONE', *, *, #16100, .F. ) ;
#25926 = PLANE ( 'NONE',  #20323 ) ;
#25927 = ORIENTED_EDGE ( 'NONE', *, *, #25112, .F. ) ;
#25928 = CARTESIAN_POINT ( 'NONE',  ( 9.668002105539015290, 16.22676391817335784, -17.88502066855795292 ) ) ;
#25929 = CARTESIAN_POINT ( 'NONE',  ( 27.39421632154990505, -5.413734532252513887, -17.93514013592066902 ) ) ;
#25930 = CARTESIAN_POINT ( 'NONE',  ( 20.31878617967674217, -0.6648838724932636390, -18.90140657046049455 ) ) ;
#25931 = DIRECTION ( 'NONE',  ( -2.698458740408365879E-16, 1.000000000000000000, 0.000000000000000000 ) ) ;
#25932 = DIRECTION ( 'NONE',  ( 0.000000000000000000, 0.8660254037844380415, -0.5000000000000011102 ) ) ;
#25933 = PLANE ( 'NONE',  #24979 ) ;
#25934 = ADVANCED_FACE ( 'NONE', ( #5844 ), #22319, .T. ) ;
#25935 = CARTESIAN_POINT ( 'NONE',  ( 25.77659985377941254, -6.250509680199615836, -13.67467641272277312 ) ) ;
#25936 = ORIENTED_EDGE ( 'NONE', *, *, #23629, .F. ) ;
#25937 = LINE ( 'NONE', #21497, #7911 ) ;
#25938 = FACE_OUTER_BOUND ( 'NONE', #2545, .T. ) ;
#25939 = CARTESIAN_POINT ( 'NONE',  ( 176.1922820468852819, -9.999999999999994671, -10.74328820663507678 ) ) ;
#25940 = DIRECTION ( 'NONE',  ( 1.000000000000000000, 4.440892098500622217E-16, 0.000000000000000000 ) ) ;
#25941 = CARTESIAN_POINT ( 'NONE',  ( 10.53683180627515981, 16.15495681678771689, -17.30800272034635867 ) ) ;
#25942 = CARTESIAN_POINT ( 'NONE',  ( 163.6922820468853104, -9.999999999999998224, -9.266330736598359152 ) ) ;
#25943 = CARTESIAN_POINT ( 'NONE',  ( 33.48796008207983022, -12.92717959506727965, -19.73506838908087246 ) ) ;
#25944 = VERTEX_POINT ( 'NONE', #24312 ) ;
#25945 = CARTESIAN_POINT ( 'NONE',  ( 8.944585970659694851, 16.95158685720792846, -17.91243444582771005 ) ) ;
#25946 = ORIENTED_EDGE ( 'NONE', *, *, #14740, .T. ) ;
#25947 = CARTESIAN_POINT ( 'NONE',  ( 0.000000000000000000, 0.000000000000000000, -2.144516984716112518 ) ) ;
#25948 = VECTOR ( 'NONE', #490, 1000.000000000000000 ) ;
#25949 = CARTESIAN_POINT ( 'NONE',  ( 17.33713706444265412, 0.9871066061555996418, -18.79342181739402307 ) ) ;
#25950 = CARTESIAN_POINT ( 'NONE',  ( 11.31663841827600692, 16.49142094814642334, -16.76779895092377615 ) ) ;
#25951 = CARTESIAN_POINT ( 'NONE',  ( 0.000000000000000000, 0.000000000000000000, 0.000000000000000000 ) ) ;
#25952 = ORIENTED_EDGE ( 'NONE', *, *, #131, .T. ) ;
#25953 = EDGE_LOOP ( 'NONE', ( #29515, #754, #30174, #1380 ) ) ;
#25954 = ORIENTED_EDGE ( 'NONE', *, *, #23626, .F. ) ;
#25955 = CARTESIAN_POINT ( 'NONE',  ( 9.641350810849047548, 17.66889113945805789, -17.91928203681695564 ) ) ;
#25956 = DIRECTION ( 'NONE',  ( -8.163404592832029035E-16, -2.202861047501738386E-31, -1.000000000000000000 ) ) ;
#25957 = CARTESIAN_POINT ( 'NONE',  ( 9.695397291186985456, 17.42102709130404747, -17.08803885907851594 ) ) ;
#25958 = CARTESIAN_POINT ( 'NONE',  ( 144.5152310637605524, -10.00000000000000355, -13.05155085951651195 ) ) ;
#25959 = ORIENTED_EDGE ( 'NONE', *, *, #10730, .F. ) ;
#25960 = CARTESIAN_POINT ( 'NONE',  ( 172.0152310637603819, -9.999999999999996447, -0.06116980274991495881 ) ) ;
#25961 = EDGE_LOOP ( 'NONE', ( #19277, #1227, #5284, #15064 ) ) ;
#25962 = CARTESIAN_POINT ( 'NONE',  ( 10.35866308580767026, 16.97206128008099313, -17.90676409391864610 ) ) ;
#25963 = ORIENTED_EDGE ( 'NONE', *, *, #1552, .F. ) ;
#25964 = CARTESIAN_POINT ( 'NONE',  ( 31.49515780845362301, -9.451207104696591088, -14.88922074032172205 ) ) ;
#25965 = CARTESIAN_POINT ( 'NONE',  ( 26.08768104250457753, -11.87935956797728210, -17.28510650846989805 ) ) ;
#25966 = CARTESIAN_POINT ( 'NONE',  ( 15.23264752967198099, 8.612683518626374379, -20.21708921969009154 ) ) ;
#25967 = VECTOR ( 'NONE', #17255, 1000.000000000000000 ) ;
#25968 = ORIENTED_EDGE ( 'NONE', *, *, #16137, .T. ) ;
#25969 = CARTESIAN_POINT ( 'NONE',  ( 63.44486372867149981, -20.00000000000000355, -186.4312945166758482 ) ) ;
#25970 = EDGE_LOOP ( 'NONE', ( #24788, #15782, #15718, #13228, #16757, #2876 ) ) ;
#25971 = CARTESIAN_POINT ( 'NONE',  ( 32.83462640711407232, -10.30445905196369516, -16.67331141712644538 ) ) ;
#25972 = APPLICATION_PROTOCOL_DEFINITION ( 'draft international standard', 'automotive_design', 1998, #10450 ) ;
#25973 = EDGE_CURVE ( 'NONE', #486, #25166, #3556, .T. ) ;
#25974 = EDGE_CURVE ( 'NONE', #1366, #29409, #12544, .T. ) ;
#25975 = CARTESIAN_POINT ( 'NONE',  ( 17.75014749421169213, 9.747325538739326944, -14.55496937630740639 ) ) ;
#25976 = EDGE_CURVE ( 'NONE', #17665, #28008, #972, .T. ) ;
#25977 = CARTESIAN_POINT ( 'NONE',  ( 17.17204249742301059, 10.23148044644768362, -15.96021614775051667 ) ) ;
#25978 = AXIS2_PLACEMENT_3D ( 'NONE', #13242, #27615, #4385 ) ;
#25979 = EDGE_CURVE ( 'NONE', #10099, #15678, #15439, .T. ) ;
#25980 = ORIENTED_EDGE ( 'NONE', *, *, #7157, .T. ) ;
#25981 = CARTESIAN_POINT ( 'NONE',  ( 133.7287565553229456, -84.33034373659253902, -41.50000000000000000 ) ) ;
#25982 = ORIENTED_EDGE ( 'NONE', *, *, #15411, .T. ) ;
#25983 = DIRECTION ( 'NONE',  ( 0.000000000000000000, -2.775557561562890735E-17, 1.000000000000000000 ) ) ;
#25984 = PLANE ( 'NONE',  #26216 ) ;
#25985 = DIRECTION ( 'NONE',  ( 0.000000000000000000, 0.000000000000000000, 1.000000000000000000 ) ) ;
#25986 = DIRECTION ( 'NONE',  ( 0.000000000000000000, 0.000000000000000000, -1.000000000000000000 ) ) ;
#25987 = UNCERTAINTY_MEASURE_WITH_UNIT (LENGTH_MEASURE( 1.000000000000000082E-05 ), #18544, 'distance_accuracy_value', 'NONE');
#25988 = CARTESIAN_POINT ( 'NONE',  ( 10.35722669462089840, 18.29854973974792998, -17.31575102165233915 ) ) ;
#25989 = FACE_OUTER_BOUND ( 'NONE', #882, .T. ) ;
#25990 = EDGE_LOOP ( 'NONE', ( #18253, #20389, #727, #8561, #12619 ) ) ;
#25991 = LINE ( 'NONE', #16968, #7591 ) ;
#25992 = EDGE_LOOP ( 'NONE', ( #7455, #14861, #19838, #13108 ) ) ;
#25993 = CARTESIAN_POINT ( 'NONE',  ( 9.981537699549546616, 16.10875070413535681, -16.47763325427154868 ) ) ;
#25994 = ORIENTED_EDGE ( 'NONE', *, *, #19781, .F. ) ;
#25995 = CARTESIAN_POINT ( 'NONE',  ( 9.669138625804738041, 16.22155169136211583, -17.88455067742322413 ) ) ;
#25996 = VECTOR ( 'NONE', #28984, 1000.000000000000000 ) ;
#25997 = CARTESIAN_POINT ( 'NONE',  ( 20.09928279393940898, 2.810699353624661168, -13.58730878818371401 ) ) ;
#25998 = DIRECTION ( 'NONE',  ( 1.000000000000000000, 0.000000000000000000, 0.000000000000000000 ) ) ;
#25999 = FILL_AREA_STYLE ('',( #16676 ) ) ;
#26000 = CARTESIAN_POINT ( 'NONE',  ( 29.22485947447185595, -8.910266539455653501, -18.36689805200119707 ) ) ;
#26001 = VERTEX_POINT ( 'NONE', #24769 ) ;
#26002 = FACE_OUTER_BOUND ( 'NONE', #5248, .T. ) ;
#26003 = CARTESIAN_POINT ( 'NONE',  ( 11.27146506517978786, 16.69859170370891377, -16.78668372539920739 ) ) ;
#26004 = EDGE_LOOP ( 'NONE', ( #1051, #20334, #15977, #29216 ) ) ;
#26005 = CARTESIAN_POINT ( 'NONE',  ( 33.40448403937627830, -11.94904316976568914, -18.43672998654903239 ) ) ;
#26006 = DIRECTION ( 'NONE',  ( 0.3090169943749475623, 8.338696094058001131E-17, 0.9510565162951536422 ) ) ;
#26007 = ORIENTED_EDGE ( 'NONE', *, *, #21722, .F. ) ;
#26008 = DIRECTION ( 'NONE',  ( 2.908569913943825061E-16, -1.000000000000000000, -6.826925868028081731E-18 ) ) ;
#26009 = CARTESIAN_POINT ( 'NONE',  ( 9.111869836743295537, 16.18440172361536611, -17.05500387803421702 ) ) ;
#26010 = CARTESIAN_POINT ( 'NONE',  ( 22.59934115267691368, -6.304331921927718518, -14.46034029096162143 ) ) ;
#26011 = VERTEX_POINT ( 'NONE', #1126 ) ;
#26012 = DIRECTION ( 'NONE',  ( 0.000000000000000000, 2.775557561562890735E-17, -1.000000000000000000 ) ) ;
#26013 = ORIENTED_EDGE ( 'NONE', *, *, #27323, .T. ) ;
#26014 =( NAMED_UNIT ( * ) SI_UNIT ( $, .STERADIAN. ) SOLID_ANGLE_UNIT ( ) );
#26015 = EDGE_CURVE ( 'NONE', #8715, #16514, #19568, .T. ) ;
#26016 = CARTESIAN_POINT ( 'NONE',  ( 16.03657434348277633, 2.746931742562784162, -16.83325620853174698 ) ) ;
#26017 = CARTESIAN_POINT ( 'NONE',  ( 18.33619432801213023, 6.228962682262685568, -18.83744168170139233 ) ) ;
#26018 = EDGE_CURVE ( 'NONE', #25015, #28921, #26616, .T. ) ;
#26019 = DIRECTION ( 'NONE',  ( -2.698458740408365879E-16, 1.000000000000000000, 0.000000000000000000 ) ) ;
#26020 = EDGE_CURVE ( 'NONE', #2818, #25866, #10106, .T. ) ;
#26021 = ORIENTED_EDGE ( 'NONE', *, *, #16824, .F. ) ;
#26022 = ORIENTED_EDGE ( 'NONE', *, *, #3982, .T. ) ;
#26023 = DIRECTION ( 'NONE',  ( -0.000000000000000000, -0.000000000000000000, -1.000000000000000000 ) ) ;
#26024 = AXIS2_PLACEMENT_3D ( 'NONE', #21122, #20811, #16240 ) ;
#26025 = LINE ( 'NONE', #9668, #9919 ) ;
#26026 = CARTESIAN_POINT ( 'NONE',  ( 0.6543461111163458854, 4.241015250120808489, -2.310849780464859560 ) ) ;
#26027 = LINE ( 'NONE', #9510, #10656 ) ;
#26028 = VERTEX_POINT ( 'NONE', #17426 ) ;
#26029 = DIRECTION ( 'NONE',  ( -2.698458740408365879E-16, 1.000000000000000000, 0.000000000000000000 ) ) ;
#26030 = CARTESIAN_POINT ( 'NONE',  ( 9.826288910175632552, 16.82074144182198694, -16.60662094963572244 ) ) ;
#26031 = CARTESIAN_POINT ( 'NONE',  ( 26.06970682676011464, -9.363093171025507644, -17.79562309782675911 ) ) ;
#26032 = CARTESIAN_POINT ( 'NONE',  ( 20.29352232415978463, 1.537418251635638944, -14.27211978419980021 ) ) ;
#26034 = ORIENTED_EDGE ( 'NONE', *, *, #23556, .F. ) ;
#26033 = CARTESIAN_POINT ( 'NONE',  ( 33.24414211882076842, -12.83183464011245967, -20.70368961610576264 ) ) ;
#26035 = LINE ( 'NONE', #12567, #15384 ) ;
#26036 = CARTESIAN_POINT ( 'NONE',  ( 12.50396148805030627, 8.572452836447732594, -15.12701763676990119 ) ) ;
#26037 = DIRECTION ( 'NONE',  ( -2.698458740408365879E-16, 1.000000000000000000, 0.000000000000000000 ) ) ;
#26038 = CARTESIAN_POINT ( 'NONE',  ( 157.0152310637604955, -1.999999999999974465, -6.958068083716895558 ) ) ;
#26039 = LINE ( 'NONE', #28050, #1487 ) ;
#26040 = DIRECTION ( 'NONE',  ( 0.3090169943749475623, 8.338696094058001131E-17, 0.9510565162951536422 ) ) ;
#26041 = CARTESIAN_POINT ( 'NONE',  ( 10.72335299953182286, 16.61944783517715862, -15.95314022879208693 ) ) ;
#26042 = DIRECTION ( 'NONE',  ( 0.9510565162951535312, 2.566386769018988816E-16, -0.3090169943749475623 ) ) ;
#26043 = LINE ( 'NONE', #18710, #11758 ) ;
#26044 = CARTESIAN_POINT ( 'NONE',  ( 16.21960234321935701, 7.070186740785398882, -14.59618053200276044 ) ) ;
#26045 = CIRCLE ( 'NONE', #1182, 5.000000000000000000 ) ;
#26046 = CARTESIAN_POINT ( 'NONE',  ( 18.20609423209794642, 11.47008825724650549, -18.02705416172272734 ) ) ;
#26047 = ORIENTED_EDGE ( 'NONE', *, *, #27967, .T. ) ;
#26048 = CARTESIAN_POINT ( 'NONE',  ( 33.43446274600908907, -12.68684440242773448, -19.71889742777951327 ) ) ;
#26049 = CARTESIAN_POINT ( 'NONE',  ( 22.08234585817149664, -3.071498426668943793, -18.09723855971599704 ) ) ;
#26050 = EDGE_CURVE ( 'NONE', #2624, #9503, #7210, .T. ) ;
#26051 = CARTESIAN_POINT ( 'NONE',  ( 18.46387099684246635, 2.251061286204190992, -18.51322769290417369 ) ) ;
#26052 = EDGE_CURVE ( 'NONE', #29696, #7452, #17280, .T. ) ;
#26053 = EDGE_CURVE ( 'NONE', #8387, #14514, #1271, .T. ) ;
#26054 = EDGE_CURVE ( 'NONE', #15139, #15488, #24773, .T. ) ;
#26055 = CARTESIAN_POINT ( 'NONE',  ( 27.61097550864939265, -12.05054904645494673, -17.30446993171443637 ) ) ;
#26056 = VERTEX_POINT ( 'NONE', #8267 ) ;
#26057 = ORIENTED_EDGE ( 'NONE', *, *, #30122, .F. ) ;
#26058 = ORIENTED_EDGE ( 'NONE', *, *, #29044, .F. ) ;
#26059 = DIRECTION ( 'NONE',  ( 0.000000000000000000, 0.8660254037844380415, -0.5000000000000012212 ) ) ;
#26061 = ORIENTED_EDGE ( 'NONE', *, *, #22669, .F. ) ;
#26060 = CARTESIAN_POINT ( 'NONE',  ( 100.8811111486825780, -4.999999999999990230, -73.29441752195363335 ) ) ;
#26062 = CARTESIAN_POINT ( 'NONE',  ( 169.5152310637604387, -4.999999999999971578, -13.05155085951651195 ) ) ;
#26063 = VECTOR ( 'NONE', #27586, 1000.000000000000000 ) ;
#26064 = ORIENTED_EDGE ( 'NONE', *, *, #5812, .T. ) ;
#26065 = CARTESIAN_POINT ( 'NONE',  ( 168.6922820468853672, -9.999999999999996447, -23.73366926340167637 ) ) ;
#26066 = CARTESIAN_POINT ( 'NONE',  ( 36.54859390953724585, -21.18451583373416014, -16.94733705004010105 ) ) ;
#26067 = CARTESIAN_POINT ( 'NONE',  ( 12.75768479220908169, 7.626547943635540783, -14.92479568483475028 ) ) ;
#26068 = VERTEX_POINT ( 'NONE', #21707 ) ;
#26069 = APPLICATION_CONTEXT ( 'automotive_design' ) ;
#26070 = FACE_OUTER_BOUND ( 'NONE', #3802, .T. ) ;
#26071 = DIRECTION ( 'NONE',  ( 0.9510565162951535312, 2.566386769018988816E-16, -0.3090169943749475623 ) ) ;
#26072 = CARTESIAN_POINT ( 'NONE',  ( 12.02780084644370007, 9.317182744227245905, -16.69143457430396893 ) ) ;
#26073 = PLANE ( 'NONE',  #2448 ) ;
#26074 = CARTESIAN_POINT ( 'NONE',  ( 4.000000000000000000, 0.000000000000000000, -2.450000000000000622 ) ) ;
#26075 = ORIENTED_EDGE ( 'NONE', *, *, #6052, .F. ) ;
#26076 = DIRECTION ( 'NONE',  ( 0.000000000000000000, 0.000000000000000000, 1.000000000000000000 ) ) ;
#26077 = LINE ( 'NONE', #21483, #5869 ) ;
#26078 = EDGE_LOOP ( 'NONE', ( #17568, #27190, #7048, #8511 ) ) ;
#26079 = CARTESIAN_POINT ( 'NONE',  ( 97.12043866711040607, -4.999999999999991118, 70.56212903019198279 ) ) ;
#26080 = EDGE_LOOP ( 'NONE', ( #4695, #23573, #28632, #21096, #1465 ) ) ;
#26081 = CARTESIAN_POINT ( 'NONE',  ( 13.37514969516658070, 7.623989538026159529, -15.71142857098959489 ) ) ;
#26082 = CARTESIAN_POINT ( 'NONE',  ( 27.64917536653120678, -4.837437286474155052, -16.54522848743341967 ) ) ;
#26083 = EDGE_CURVE ( 'NONE', #220, #6891, #22478, .T. ) ;
#26084 = CARTESIAN_POINT ( 'NONE',  ( 22.75707610144304383, -3.504958924507949991, -13.40925247317622571 ) ) ;
#26085 = DIRECTION ( 'NONE',  ( 0.000000000000000000, 0.000000000000000000, 1.000000000000000000 ) ) ;
#26086 = CARTESIAN_POINT ( 'NONE',  ( 168.6922820468853672, -4.999999999999971578, -23.73366926340167637 ) ) ;
#26087 = VECTOR ( 'NONE', #18994, 1000.000000000000000 ) ;
#26088 = LINE ( 'NONE', #9424, #18135 ) ;
#26089 = ADVANCED_FACE ( 'NONE', ( #20618 ), #13749, .F. ) ;
#26090 = EDGE_LOOP ( 'NONE', ( #2437, #6434, #13593, #25045 ) ) ;
#26091 = LINE ( 'NONE', #23961, #13303 ) ;
#26092 = VECTOR ( 'NONE', #28849, 1000.000000000000000 ) ;
#26093 = CARTESIAN_POINT ( 'NONE',  ( 153.6922820468853388, -1.999999999999975797, -15.07341522555727309 ) ) ;
#26094 = CARTESIAN_POINT ( 'NONE',  ( 152.0152310637604955, -10.00000000000000178, 1.702185954127501066 ) ) ;
#26095 = LINE ( 'NONE', #16462, #18064 ) ;
#26096 = PLANE ( 'NONE',  #11394 ) ;
#26097 = CARTESIAN_POINT ( 'NONE',  ( 12.02710433905669341, 9.320377015888107408, -16.69172260460959478 ) ) ;
#26098 = CARTESIAN_POINT ( 'NONE',  ( 115.2397606401234924, -4.999999999999985789, -83.72658702220800819 ) ) ;
#26099 = CARTESIAN_POINT ( 'NONE',  ( 33.54145741815126058, -13.16751478770765793, -19.75123935038191192 ) ) ;
#26100 = EDGE_LOOP ( 'NONE', ( #24717, #5646, #4392, #23829, #18215 ) ) ;
#26101 = CARTESIAN_POINT ( 'NONE',  ( 13.38095672321806795, 7.626547943635540783, -15.70680086385617358 ) ) ;
#26102 = CARTESIAN_POINT ( 'NONE',  ( 137.0152310637606092, -4.999999999999980460, -32.93883019725009120 ) ) ;
#26103 = AXIS2_PLACEMENT_3D ( 'NONE', #6886, #13732, #18467 ) ;
#26104 = CARTESIAN_POINT ( 'NONE',  ( 21.64656857049893901, 5.639188926465734220, -17.17864421186117951 ) ) ;
#26105 = CARTESIAN_POINT ( 'NONE',  ( 12.83231907764629476, 9.540323555994485005, -16.14101112307237074 ) ) ;
#26106 = CARTESIAN_POINT ( 'NONE',  ( 137.0152310637605808, -1.999999999999979572, -26.04193191628310800 ) ) ;
#26107 = EDGE_LOOP ( 'NONE', ( #10688, #6812, #15409, #28839, #27217 ) ) ;
#26108 = EDGE_CURVE ( 'NONE', #29328, #27629, #12070, .T. ) ;
#26109 = ORIENTED_EDGE ( 'NONE', *, *, #16897, .F. ) ;
#26110 = ORIENTED_EDGE ( 'NONE', *, *, #24389, .F. ) ;
#26111 = CARTESIAN_POINT ( 'NONE',  ( 11.50832337395308436, 9.139936167900076569, -15.84372008594036885 ) ) ;
#26112 = DIRECTION ( 'NONE',  ( 0.9510565162951535312, 2.566386769018988816E-16, -0.3090169943749475623 ) ) ;
#26113 = CARTESIAN_POINT ( 'NONE',  ( 9.924804006935172396, 16.36893865032855899, -16.50109463189289016 ) ) ;
#26114 = CARTESIAN_POINT ( 'NONE',  ( 142.0152310637605808, -1.999999999999978018, -17.38167787843871182 ) ) ;
#26115 = VERTEX_POINT ( 'NONE', #1725 ) ;
#26116 = LINE ( 'NONE', #23826, #20300 ) ;
#26117 = VERTEX_POINT ( 'NONE', #15590 ) ;
#26118 = CARTESIAN_POINT ( 'NONE',  ( 10.47604570704546845, 16.43372961628045559, -17.33313991065496751 ) ) ;
#26119 = AXIS2_PLACEMENT_3D ( 'NONE', #21924, #8028, #22386 ) ;
#26120 = ORIENTED_EDGE ( 'NONE', *, *, #20481, .F. ) ;
#26121 = CARTESIAN_POINT ( 'NONE',  ( 32.21775685856648153, -9.560954865089090760, -16.93152350858319366 ) ) ;
#26122 = CARTESIAN_POINT ( 'NONE',  ( 28.01381056668970260, -10.10121741814351459, -18.82353034625045041 ) ) ;
#26123 = CARTESIAN_POINT ( 'NONE',  ( 16.30094628073386076, 10.97451324635404291, -15.74372407192620216 ) ) ;
#26124 = ORIENTED_EDGE ( 'NONE', *, *, #12896, .T. ) ;
#26125 = VECTOR ( 'NONE', #19487, 1000.000000000000000 ) ;
#26126 = LINE ( 'NONE', #16947, #17899 ) ;
#26127 = ADVANCED_FACE ( 'NONE', ( #23078 ), #11452, .T. ) ;
#26128 = CARTESIAN_POINT ( 'NONE',  ( 33.97319001242765779, -11.13623552147873141, -19.50814438409551954 ) ) ;
#26129 = APPLICATION_PROTOCOL_DEFINITION ( 'draft international standard', 'automotive_design', 1998, #15530 ) ;
#26130 = CARTESIAN_POINT ( 'NONE',  ( 18.67986154365276619, -0.9315889389632653339, -17.94220784458306994 ) ) ;
#26131 = AXIS2_PLACEMENT_3D ( 'NONE', #22882, #1985, #14444 ) ;
#26132 = CARTESIAN_POINT ( 'NONE',  ( 26.86129341093661793, -9.458291044957649163, -14.14057404834478682 ) ) ;
#26133 = AXIS2_PLACEMENT_3D ( 'NONE', #6653, #23434, #13663 ) ;
#26134 = FACE_BOUND ( 'NONE', #2824, .T. ) ;
#26135 = CARTESIAN_POINT ( 'NONE',  ( 174.7287565553229456, -1.999999999999968470, -33.82050807568879947 ) ) ;
#26136 = CARTESIAN_POINT ( 'NONE',  ( 176.1922820468853388, -9.999999999999994671, -30.91696583120936026 ) ) ;
#26137 = PLANE ( 'NONE',  #8726 ) ;
#26138 = CARTESIAN_POINT ( 'NONE',  ( 8.469702402841419307E-15, 60.00000000000000711, 12.49999999999999112 ) ) ;
#26139 = AXIS2_PLACEMENT_3D ( 'NONE', #11674, #23138, #11520 ) ;
#26140 = CARTESIAN_POINT ( 'NONE',  ( 12.27341590537944249, 9.504120828508773045, -15.31263355901650947 ) ) ;
#26141 = CARTESIAN_POINT ( 'NONE',  ( 146.1922820468854241, -10.00000000000000355, -10.74328820663507678 ) ) ;
#26142 = EDGE_CURVE ( 'NONE', #25250, #4687, #11311, .T. ) ;
#26143 = DIRECTION ( 'NONE',  ( 1.000000000000000000, 2.891205793294675861E-16, 0.000000000000000000 ) ) ;
#26144 = EDGE_LOOP ( 'NONE', ( #20381, #8411 ) ) ;
#26145 = AXIS2_PLACEMENT_3D ( 'NONE', #15012, #3438, #12731 ) ;
#26146 = CARTESIAN_POINT ( 'NONE',  ( 11.97192087863669663, 8.579774655713777065, -15.53257280409644991 ) ) ;
#26147 = EDGE_CURVE ( 'NONE', #18723, #10809, #1884, .T. ) ;
#26148 = VERTEX_POINT ( 'NONE', #9157 ) ;
#26149 = AXIS2_PLACEMENT_3D ( 'NONE', #10129, #19441, #28957 ) ;
#26150 = CARTESIAN_POINT ( 'NONE',  ( 16.42253358145367415, 4.166353156564198024, -16.06924993952044289 ) ) ;
#26151 = CARTESIAN_POINT ( 'NONE',  ( 129.5152310637605524, -10.00000000000000888, -30.37205893520530964 ) ) ;
#26152 = DIRECTION ( 'NONE',  ( -2.698458740408365879E-16, 1.000000000000000000, 0.000000000000000000 ) ) ;
#26154 = EDGE_LOOP ( 'NONE', ( #5990, #11873, #10708, #13847, #8995 ) ) ;
#26153 = CARTESIAN_POINT ( 'NONE',  ( 139.5152310637605524, -4.999999999999980460, -4.391296821672111328 ) ) ;
#26155 = ORIENTED_EDGE ( 'NONE', *, *, #3478, .T. ) ;
#26156 = CARTESIAN_POINT ( 'NONE',  ( 2.500000000000000444, -2.357898499370430834, 3.469446951953614189E-15 ) ) ;
#26157 = CARTESIAN_POINT ( 'NONE',  ( 11.16343636398553052, 17.19402509784177369, -16.95964061678045454 ) ) ;
#26158 = ORIENTED_EDGE ( 'NONE', *, *, #5049, .F. ) ;
#26159 = CARTESIAN_POINT ( 'NONE',  ( 33.23735339574943026, -11.79161913663336314, -18.04114522998021997 ) ) ;
#26160 = CARTESIAN_POINT ( 'NONE',  ( 20.23291344124205793, 5.521974472852556381, -14.51730806008046137 ) ) ;
#26161 = FACE_OUTER_BOUND ( 'NONE', #8219, .T. ) ;
#26162 = CARTESIAN_POINT ( 'NONE',  ( 10.14999423553203606, 11.42343090068832190, -16.62569685487721571 ) ) ;
#26163 = CARTESIAN_POINT ( 'NONE',  ( 24.76964776845370864, -3.801875552749832909, -18.97459646659829247 ) ) ;
#26164 = ORIENTED_EDGE ( 'NONE', *, *, #230, .T. ) ;
#26165 = CARTESIAN_POINT ( 'NONE',  ( 148.6922820468853672, -4.999999999999976907, 2.247092850131519715 ) ) ;
#26166 = PRESENTATION_STYLE_ASSIGNMENT (( #28183 ) ) ;
#26167 = CARTESIAN_POINT ( 'NONE',  ( 20.73027244251523626, 3.305903845835247434, -19.25852547563239625 ) ) ;
#26168 = CARTESIAN_POINT ( 'NONE',  ( 17.81918496738754953, 9.416330548141603529, -16.00206777915198586 ) ) ;
#26169 = VECTOR ( 'NONE', #3863, 1000.000000000000000 ) ;
#26170 = CARTESIAN_POINT ( 'NONE',  ( 133.7287565553229172, -4.999999999999982236, -36.50000000000000711 ) ) ;
#26171 = VERTEX_POINT ( 'NONE', #27243 ) ;
#26172 = LINE ( 'NONE', #5405, #22441 ) ;
#26173 = AXIS2_PLACEMENT_3D ( 'NONE', #8744, #30181, #13776 ) ;
#26174 =( GEOMETRIC_REPRESENTATION_CONTEXT ( 3 ) GLOBAL_UNCERTAINTY_ASSIGNED_CONTEXT ( ( #1897 ) ) GLOBAL_UNIT_ASSIGNED_CONTEXT ( ( #9281, #9585, #30119 ) ) REPRESENTATION_CONTEXT ( 'NONE', 'WORKASPACE' ) );
#26175 = CARTESIAN_POINT ( 'NONE',  ( 8.500000000000088818, 17.32050807568872486, -30.00000000000000711 ) ) ;
#26176 = DIRECTION ( 'NONE',  ( -0.5877852522924731371, -1.586114251531760235E-16, 0.8090169943749474513 ) ) ;
#26177 = DIRECTION ( 'NONE',  ( -0.9510565162951536422, -2.566386769018988816E-16, -0.3090169943749472292 ) ) ;
#26178 = CARTESIAN_POINT ( 'NONE',  ( 134.7287565553230024, -4.999999999999981348, -16.50000000000000000 ) ) ;
#26179 = CARTESIAN_POINT ( 'NONE',  ( 9.641384570184822422, 17.66873631484086715, -17.89388817125738385 ) ) ;
#26180 = CARTESIAN_POINT ( 'NONE',  ( 26.67280208910032258, -8.806626608708889137, -18.22016464309510653 ) ) ;
#26181 = CARTESIAN_POINT ( 'NONE',  ( 24.00718893345771932, -1.002666751694005765, -18.91818096615087796 ) ) ;
#26182 = EDGE_CURVE ( 'NONE', #24619, #2471, #25247, .T. ) ;
#26184 = ORIENTED_EDGE ( 'NONE', *, *, #29061, .T. ) ;
#26183 = CARTESIAN_POINT ( 'NONE',  ( 35.54859390953724585, -23.18451583373416014, -18.19919658220850422 ) ) ;
#26185 = CARTESIAN_POINT ( 'NONE',  ( 131.1922820468854241, -10.00000000000000888, -22.25671179336495697 ) ) ;
#26186 = CARTESIAN_POINT ( 'NONE',  ( 12.55500454421123457, 8.595009676161804890, -15.08633542003848049 ) ) ;
#26187 = ADVANCED_FACE ( 'NONE', ( #27398 ), #6248, .T. ) ;
#26188 = CIRCLE ( 'NONE', #27665, 5.000000000000000000 ) ;
#26189 = DIRECTION ( 'NONE',  ( -2.698458740408365879E-16, 1.000000000000000000, 0.000000000000000000 ) ) ;
#26190 = DIRECTION ( 'NONE',  ( 0.000000000000000000, 0.000000000000000000, 1.000000000000000000 ) ) ;
#26191 = EDGE_CURVE ( 'NONE', #16627, #20965, #24923, .T. ) ;
#26192 = CARTESIAN_POINT ( 'NONE',  ( 19.91209246711783010, 5.411768277715644615, -14.29674560697521457 ) ) ;
#26193 = ORIENTED_EDGE ( 'NONE', *, *, #29204, .T. ) ;
#26194 = LINE ( 'NONE', #14711, #23696 ) ;
#26195 = CARTESIAN_POINT ( 'NONE',  ( 10.61946839964472034, 17.09587585246520902, -16.05247762654136068 ) ) ;
#26196 = CIRCLE ( 'NONE', #10572, 3.000000000000002665 ) ;
#26197 = CARTESIAN_POINT ( 'NONE',  ( 141.1922820468854241, -10.00000000000000533, -2.083034168790677043 ) ) ;
#26198 = FACE_OUTER_BOUND ( 'NONE', #19734, .T. ) ;
#26199 = CARTESIAN_POINT ( 'NONE',  ( 17.36512755686010934, 0.5347363583120325892, -15.24149349723765390 ) ) ;
#26200 = CARTESIAN_POINT ( 'NONE',  ( 16.80873327975549003, 11.45062080556171757, -15.01659013532395370 ) ) ;
#26201 = EDGE_LOOP ( 'NONE', ( #24495, #9652, #12237, #18664, #5462 ) ) ;
#26202 = CARTESIAN_POINT ( 'NONE',  ( 35.37764311538968087, -21.41652447078215005, -19.89511094362359955 ) ) ;
#26203 = CARTESIAN_POINT ( 'NONE',  ( 23.48045015178454165, 1.263488895044508897, -17.26779756161726098 ) ) ;
#26204 = CARTESIAN_POINT ( 'NONE',  ( 19.81827328964134338, 3.502454073897792952, -18.79004964864563476 ) ) ;
#26205 = CARTESIAN_POINT ( 'NONE',  ( 26.70980024742295456, -9.230482666323300833, -19.13350686062700134 ) ) ;
#26206 = PRESENTATION_LAYER_ASSIGNMENT (  '', '', ( #28653 ) ) ;
#26207 = EDGE_LOOP ( 'NONE', ( #4982, #919, #15308, #10684 ) ) ;
#26208 = LINE ( 'NONE', #16880, #24537 ) ;
#26210 = ORIENTED_EDGE ( 'NONE', *, *, #21958, .F. ) ;
#26209 = CARTESIAN_POINT ( 'NONE',  ( 13.87499999999999822, 0.000000000000000000, 0.000000000000000000 ) ) ;
#26211 = AXIS2_PLACEMENT_3D ( 'NONE', #29743, #11642, #15921 ) ;
#26212 = DIRECTION ( 'NONE',  ( -2.698458740408365879E-16, 1.000000000000000000, 0.000000000000000000 ) ) ;
#26213 = LINE ( 'NONE', #7132, #7312 ) ;
#26214 = ADVANCED_FACE ( 'NONE', ( #29858 ), #29702, .T. ) ;
#26215 = CARTESIAN_POINT ( 'NONE',  ( 33.49783966318349115, -10.45910432307822902, -18.51641766868578287 ) ) ;
#26216 = AXIS2_PLACEMENT_3D ( 'NONE', #5521, #7948, #24140 ) ;
#26217 = CARTESIAN_POINT ( 'NONE',  ( 9.641350810849047548, 17.66889113945805789, -17.97192418671891190 ) ) ;
#26218 = EDGE_CURVE ( 'NONE', #2461, #19125, #8716, .T. ) ;
#26219 = LINE ( 'NONE', #5301, #16130 ) ;
#26220 = LINE ( 'NONE', #11852, #12915 ) ;
#26221 = EDGE_CURVE ( 'NONE', #13500, #25744, #25725, .T. ) ;
#26222 = EDGE_CURVE ( 'NONE', #15024, #29186, #20168, .T. ) ;
#26223 = CARTESIAN_POINT ( 'NONE',  ( 11.99569818778800645, 9.464409628959467469, -16.70471015293584216 ) ) ;
#26224 = FACE_OUTER_BOUND ( 'NONE', #26536, .T. ) ;
#26225 = EDGE_CURVE ( 'NONE', #22156, #22605, #18329, .T. ) ;
#26226 = DIRECTION ( 'NONE',  ( -2.698458740408365879E-16, 1.000000000000000000, 0.000000000000000000 ) ) ;
#26227 = VERTEX_POINT ( 'NONE', #25363 ) ;
#26228 = DIRECTION ( 'NONE',  ( 1.000000000000000000, 0.000000000000000000, 0.000000000000000000 ) ) ;
#26229 = VECTOR ( 'NONE', #18476, 1000.000000000000000 ) ;
#26230 = CYLINDRICAL_SURFACE ( 'NONE', #10249, 13.00000000000000178 ) ;
#26231 = EDGE_LOOP ( 'NONE', ( #24469, #5313, #20187, #24758 ) ) ;
#26232 = VERTEX_POINT ( 'NONE', #29549 ) ;
#26233 = CARTESIAN_POINT ( 'NONE',  ( 11.29844335826449964, 8.819016302236921234, -17.20546268888528374 ) ) ;
#26234 = AXIS2_PLACEMENT_3D ( 'NONE', #7791, #15249, #3668 ) ;
#26235 = CARTESIAN_POINT ( 'NONE',  ( 26.11288949521356528, -6.777652795969290267, -18.96966820991230662 ) ) ;
#26236 = CARTESIAN_POINT ( 'NONE',  ( 19.50876870223950377, -1.661710298099399630, -15.95382585723518432 ) ) ;
#26237 = CARTESIAN_POINT ( 'NONE',  ( 120.0000000000000000, 20.00000000000000355, -17.99999999999998934 ) ) ;
#26238 = LINE ( 'NONE', #17355, #15997 ) ;
#26239 = CARTESIAN_POINT ( 'NONE',  ( 15.00000000000000000, 4.735455214955320607E-16, 5.000000000000000000 ) ) ;
#26240 = VECTOR ( 'NONE', #7805, 1000.000000000000000 ) ;
#26241 = VERTEX_POINT ( 'NONE', #22932 ) ;
#26242 = DIRECTION ( 'NONE',  ( -2.698458740408365879E-16, 1.000000000000000000, 0.000000000000000000 ) ) ;
#26243 = ADVANCED_FACE ( 'NONE', ( #2034 ), #27687, .T. ) ;
#26244 = PLANE ( 'NONE',  #19132 ) ;
#26245 = FACE_OUTER_BOUND ( 'NONE', #4632, .T. ) ;
#26246 = FACE_OUTER_BOUND ( 'NONE', #18504, .T. ) ;
#26247 = CARTESIAN_POINT ( 'NONE',  ( 10.47175433613752027, 16.45341039028688002, -17.33491556667247835 ) ) ;
#26248 = PLANE ( 'NONE',  #2391 ) ;
#26249 = CARTESIAN_POINT ( 'NONE',  ( 31.63980255171021483, -10.89810845426378982, -15.52824638758754183 ) ) ;
#26250 = VECTOR ( 'NONE', #18900, 1000.000000000000000 ) ;
#26251 = VERTEX_POINT ( 'NONE', #8566 ) ;
#26252 = CARTESIAN_POINT ( 'NONE',  ( 13.37763225631166542, 7.625080029534266224, -15.70945042905673006 ) ) ;
#26253 = EDGE_CURVE ( 'NONE', #9664, #25774, #4458, .T. ) ;
#26254 = CARTESIAN_POINT ( 'NONE',  ( 157.0152310637605240, -1.999999999999974021, -15.61832212156129707 ) ) ;
#26255 = CARTESIAN_POINT ( 'NONE',  ( 19.12501085131992085, -2.578449613843157184, -15.80510918775627438 ) ) ;
#26256 = EDGE_CURVE ( 'NONE', #24657, #25565, #26126, .T. ) ;
#26257 = CARTESIAN_POINT ( 'NONE',  ( 12.82970573826865390, 9.552301347437191836, -16.14209238882153130 ) ) ;
#26258 = LINE ( 'NONE', #21360, #17513 ) ;
#26259 = VECTOR ( 'NONE', #15134, 1000.000000000000000 ) ;
#26260 = ADVANCED_FACE ( 'NONE', ( #4604 ), #14041, .T. ) ;
#26261 = ORIENTED_EDGE ( 'NONE', *, *, #8492, .F. ) ;
#26262 = CARTESIAN_POINT ( 'NONE',  ( 11.14863080475985591, 10.75631295387255548, -15.99499920034263489 ) ) ;
#26263 = DIRECTION ( 'NONE',  ( 1.000000000000000000, -0.000000000000000000, -0.000000000000000000 ) ) ;
#26264 = EDGE_LOOP ( 'NONE', ( #9622, #5039, #18687, #16761, #17644 ) ) ;
#26265 = CARTESIAN_POINT ( 'NONE',  ( 9.917205744531459644, 16.40378525026516243, -16.50423678068149869 ) ) ;
#26266 = DIRECTION ( 'NONE',  ( -2.698458740408365879E-16, 1.000000000000000000, 0.000000000000000000 ) ) ;
#26267 = ORIENTED_EDGE ( 'NONE', *, *, #20242, .T. ) ;
#26268 = LINE ( 'NONE', #21820, #29137 ) ;
#26269 = ORIENTED_EDGE ( 'NONE', *, *, #8452, .T. ) ;
#26270 = CARTESIAN_POINT ( 'NONE',  ( 11.99569818778800645, 9.464409628959467469, -16.70471015293584216 ) ) ;
#26271 = VERTEX_POINT ( 'NONE', #23834 ) ;
#26272 = CARTESIAN_POINT ( 'NONE',  ( 34.10649047503919462, -12.21345526111254287, -20.89408644300621987 ) ) ;
#26273 = CARTESIAN_POINT ( 'NONE',  ( 15.95367323521391256, 9.281262803959288377, -20.14168370736028280 ) ) ;
#26274 = CARTESIAN_POINT ( 'NONE',  ( 16.07247723200118372, 10.90037199175087324, -15.55898442674143745 ) ) ;
#26275 = LINE ( 'NONE', #772, #11120 ) ;
#26276 = DIRECTION ( 'NONE',  ( -0.5877852522924731371, -1.586114251531760728E-16, -0.8090169943749474513 ) ) ;
#26277 = APPLICATION_PROTOCOL_DEFINITION ( 'draft international standard', 'automotive_design', 1998, #26477 ) ;
#26278 = ORIENTED_EDGE ( 'NONE', *, *, #24952, .F. ) ;
#26279 = CARTESIAN_POINT ( 'NONE',  ( 19.60537025999656890, 4.505197036469223981, -15.34927506990110047 ) ) ;
#26280 = AXIS2_PLACEMENT_3D ( 'NONE', #16706, #23893, #5561 ) ;
#26281 = CARTESIAN_POINT ( 'NONE',  ( 15.44629794785920218, 3.545610805586186132, -16.71614555938632307 ) ) ;
#26282 = VECTOR ( 'NONE', #14554, 1000.000000000000000 ) ;
#26283 = LINE ( 'NONE', #12516, #15883 ) ;
#26284 = EDGE_CURVE ( 'NONE', #16077, #11753, #16452, .T. ) ;
#26285 = FACE_BOUND ( 'NONE', #3319, .T. ) ;
#26286 = LINE ( 'NONE', #787, #10633 ) ;
#26287 = DIRECTION ( 'NONE',  ( 1.000000000000000000, 4.440892098500622217E-16, 0.000000000000000000 ) ) ;
#26288 = LINE ( 'NONE', #2791, #21907 ) ;
#26289 = PLANE ( 'NONE',  #7555 ) ;
#26290 = CARTESIAN_POINT ( 'NONE',  ( 12.26883957244698387, 9.531649408071682927, -15.31402716519172635 ) ) ;
#26291 = CARTESIAN_POINT ( 'NONE',  ( 142.2287565553230309, -1.999999999999978018, -12.16987298107780369 ) ) ;
#26292 = ORIENTED_EDGE ( 'NONE', *, *, #25040, .T. ) ;
#26293 = AXIS2_PLACEMENT_3D ( 'NONE', #12826, #1401, #28916 ) ;
#26294 = CARTESIAN_POINT ( 'NONE',  ( 6.686525924292798351, -5.377136764700186866, -4.683279549040149092 ) ) ;
#26295 = ORIENTED_EDGE ( 'NONE', *, *, #19479, .F. ) ;
#26296 = CARTESIAN_POINT ( 'NONE',  ( 12.49428694376680049, 8.568214790255201052, -15.13472557389765072 ) ) ;
#26297 = ORIENTED_EDGE ( 'NONE', *, *, #10143, .T. ) ;
#26298 = CARTESIAN_POINT ( 'NONE',  ( 16.67011857490315307, 4.279483903030143921, -15.63504347475558198 ) ) ;
#26299 = DIRECTION ( 'NONE',  ( 0.3090169943749475623, 8.338696094058001131E-17, 0.9510565162951536422 ) ) ;
#26300 = FACE_OUTER_BOUND ( 'NONE', #9911, .T. ) ;
#26301 = LINE ( 'NONE', #26604, #1012 ) ;
#26302 = CIRCLE ( 'NONE', #6796, 13.00000000000000178 ) ;
#26303 = VERTEX_POINT ( 'NONE', #19089 ) ;
#26304 = FACE_OUTER_BOUND ( 'NONE', #2696, .T. ) ;
#26305 = CARTESIAN_POINT ( 'NONE',  ( 12.86106464449595777, 9.514195438118767001, -16.12106201145810047 ) ) ;
#26306 = EDGE_LOOP ( 'NONE', ( #5843, #9920, #8541, #12542 ) ) ;
#26307 = CLOSED_SHELL ( 'NONE', ( #16615, #4018, #3547, #13859, #6951, #268, #1934, #2109, #10311, #21062, #12513, #23140, #6266, #2937, #4402, #27516, #24992, #4197, #11283, #7118, #22035, #2145, #2887, #21477, #21932, #24700, #19105, #13104 ) ) ;
#26308 = CARTESIAN_POINT ( 'NONE',  ( 34.62340031318386480, -17.02811109401968181, -19.03596318374462726 ) ) ;
#26309 = CARTESIAN_POINT ( 'NONE',  ( 14.18486973814142793, 6.324582201221724098, -17.68508340245422872 ) ) ;
#26310 = CARTESIAN_POINT ( 'NONE',  ( 154.7287565553229456, -10.00000000000000178, -7.839745962155603820 ) ) ;
#26311 = CARTESIAN_POINT ( 'NONE',  ( 26.29067154119281824, -12.76617647537077538, -18.64558906701574514 ) ) ;
#26312 = ORIENTED_EDGE ( 'NONE', *, *, #19479, .T. ) ;
#26313 = DIRECTION ( 'NONE',  ( 0.000000000000000000, -0.000000000000000000, -1.000000000000000000 ) ) ;
#26314 = SURFACE_STYLE_USAGE ( .BOTH. , #16988 ) ;
#26315 = CARTESIAN_POINT ( 'NONE',  ( 20.61437924707763258, -4.384239709691692966, -16.09784705243023240 ) ) ;
#26316 = CARTESIAN_POINT ( 'NONE',  ( 16.31265859067239532, 4.319332383768222705, -17.78589364095596892 ) ) ;
#26317 = EDGE_LOOP ( 'NONE', ( #8613, #29348, #3599, #21026 ) ) ;
#26318 = CARTESIAN_POINT ( 'NONE',  ( 151.1922820468853672, -10.00000000000000178, -4.936203717676158398 ) ) ;
#26319 = ORIENTED_EDGE ( 'NONE', *, *, #29711, .F. ) ;
#26320 = EDGE_CURVE ( 'NONE', #11833, #14224, #7492, .T. ) ;
#26321 = CARTESIAN_POINT ( 'NONE',  ( 173.6922820468852819, -1.999999999999970468, -9.266330736598359152 ) ) ;
#26322 = AXIS2_PLACEMENT_3D ( 'NONE', #4282, #13585, #20145 ) ;
#26323 = EDGE_CURVE ( 'NONE', #4416, #6999, #23524, .T. ) ;
#26324 = VECTOR ( 'NONE', #20410, 1000.000000000000000 ) ;
#26325 = PLANE ( 'NONE',  #20632 ) ;
#26326 = VECTOR ( 'NONE', #24668, 999.9999999999998863 ) ;
#26327 = CARTESIAN_POINT ( 'NONE',  ( 8.000000000000000000, -4.618802153517027165, -4.285468820183664818 ) ) ;
#26328 = CARTESIAN_POINT ( 'NONE',  ( 171.1922820468853388, -9.999999999999996447, -22.25671179336496053 ) ) ;
#26329 = DIRECTION ( 'NONE',  ( 0.5877852522924731371, 0.000000000000000000, 0.8090169943749474513 ) ) ;
#26330 = CARTESIAN_POINT ( 'NONE',  ( 11.49350937636955372, 9.187954247928445284, -15.85136552863131421 ) ) ;
#26331 = CARTESIAN_POINT ( 'NONE',  ( 29.11570147443254797, -8.594497869595446815, -15.09001435577217087 ) ) ;
#26332 = CARTESIAN_POINT ( 'NONE',  ( 24.27430760268559595, -10.23567508289028716, -17.26834523416827949 ) ) ;
#26334 = ORIENTED_EDGE ( 'NONE', *, *, #12799, .T. ) ;
#26333 = CARTESIAN_POINT ( 'NONE',  ( 34.70640263809442416, -19.40099657226499019, -21.14569589167440000 ) ) ;
#26335 = CARTESIAN_POINT ( 'NONE',  ( 172.7287565553229456, -9.999999999999971578, 0.5000000000000029976 ) ) ;
#26336 = CARTESIAN_POINT ( 'NONE',  ( 152.0152310637604671, -1.999999999999976241, -0.06116980274991495881 ) ) ;
#26337 = CARTESIAN_POINT ( 'NONE',  ( 161.1922820468853956, -1.999999999999973577, -28.06379628232387446 ) ) ;
#26338 = CARTESIAN_POINT ( 'NONE',  ( 25.00000000000000000, 0.000000000000000000, 0.000000000000000000 ) ) ;
#26339 = CARTESIAN_POINT ( 'NONE',  ( 146.1922820468853956, -10.00000000000000355, -2.083034168790677043 ) ) ;
#26340 = DIRECTION ( 'NONE',  ( 0.000000000000000000, -2.775557561562890735E-17, 1.000000000000000000 ) ) ;
#26341 = CARTESIAN_POINT ( 'NONE',  ( 17.33713706444265412, 0.9871066061555996418, -18.79342181739402307 ) ) ;
#26343 = ORIENTED_EDGE ( 'NONE', *, *, #1837, .T. ) ;
#26342 = COLOUR_RGB ( '', 0.72549020, 0.75294118, 0.79215686) ;
#26344 = CARTESIAN_POINT ( 'NONE',  ( 167.0152310637605524, -4.999999999999971578, -32.93883019725009120 ) ) ;
#26345 = CARTESIAN_POINT ( 'NONE',  ( 12.27009251048667160, 9.509012028593735621, -15.31479730457434307 ) ) ;
#26346 = AXIS2_PLACEMENT_3D ( 'NONE', #804, #659, #7518 ) ;
#26347 = LINE ( 'NONE', #14562, #24203 ) ;
#26348 = CARTESIAN_POINT ( 'NONE',  ( 166.1922820468853672, -1.999999999999971800, -22.25671179336496053 ) ) ;
#26349 = AXIS2_PLACEMENT_3D ( 'NONE', #9206, #20810, #16084 ) ;
#26350 = CARTESIAN_POINT ( 'NONE',  ( 22.89472691350227507, 1.279074496056108901, -19.72372301458170796 ) ) ;
#26351 = CARTESIAN_POINT ( 'NONE',  ( 26.88742137321887427, -10.86886578961255978, -19.57440296808016100 ) ) ;
#26352 = ORIENTED_EDGE ( 'NONE', *, *, #24389, .T. ) ;
#26353 = CARTESIAN_POINT ( 'NONE',  ( 35.54287943964028784, -22.15884374752674546, -18.65915260879160797 ) ) ;
#26354 =( LENGTH_UNIT ( ) NAMED_UNIT ( * ) SI_UNIT ( .MILLI., .METRE. ) );
#26355 = CARTESIAN_POINT ( 'NONE',  ( 28.41550859958678643, -4.728095322062062067, -17.81194336819277524 ) ) ;
#26356 = CARTESIAN_POINT ( 'NONE',  ( 20.29079399015155616, 4.720006093641750944, -15.95989367155712202 ) ) ;
#26357 = EDGE_LOOP ( 'NONE', ( #21356, #14027, #4516, #3850, #1019 ) ) ;
#26358 = ORIENTED_EDGE ( 'NONE', *, *, #27487, .T. ) ;
#26359 = VECTOR ( 'NONE', #13983, 1000.000000000000000 ) ;
#26360 = ADVANCED_FACE ( 'NONE', ( #32 ), #16798, .T. ) ;
#26361 = EDGE_CURVE ( 'NONE', #14364, #19566, #14497, .T. ) ;
#26362 = VECTOR ( 'NONE', #26189, 1000.000000000000000 ) ;
#26363 = EDGE_CURVE ( 'NONE', #6624, #16563, #14340, .T. ) ;
#26364 = ADVANCED_FACE ( 'NONE', ( #23220 ), #9917, .T. ) ;
#26365 = CARTESIAN_POINT ( 'NONE',  ( 174.7287565553228887, -4.999999999999970690, -16.50000000000000000 ) ) ;
#26367 = EDGE_LOOP ( 'NONE', ( #19851, #23871 ) ) ;
#26366 = FACE_OUTER_BOUND ( 'NONE', #1358, .T. ) ;
#26368 = DIRECTION ( 'NONE',  ( -0.9510565162951536422, -2.566386769018988323E-16, 0.3090169943749475623 ) ) ;
#26369 = CARTESIAN_POINT ( 'NONE',  ( 173.6922820468853104, -9.999999999999994671, -15.07341522555727664 ) ) ;
#26370 = DIRECTION ( 'NONE',  ( -0.8090169943749474513, -2.183098979609982436E-16, 0.5877852522924731371 ) ) ;
#26371 = CARTESIAN_POINT ( 'NONE',  ( 35.34711162051457478, -16.78689235204268115, -20.22678452305727603 ) ) ;
#26372 = CARTESIAN_POINT ( 'NONE',  ( 10.17605321708455257, 15.21667774575863419, -16.39719424528293246 ) ) ;
#26373 = CARTESIAN_POINT ( 'NONE',  ( 174.7287565553229456, -9.999999999999994671, -33.82050807568879947 ) ) ;
#26374 = LINE ( 'NONE', #426, #3671 ) ;
#26375 = CARTESIAN_POINT ( 'NONE',  ( 12.84373479294319864, 8.511860559062048637, -16.13004233893675377 ) ) ;
#26376 = CYLINDRICAL_SURFACE ( 'NONE', #25862, 2.928571428571432378 ) ;
#26377 = ORIENTED_EDGE ( 'NONE', *, *, #28242, .F. ) ;
#26378 = FACE_OUTER_BOUND ( 'NONE', #18359, .T. ) ;
#26379 = VECTOR ( 'NONE', #19489, 999.9999999999998863 ) ;
#26380 = ORIENTED_EDGE ( 'NONE', *, *, #5670, .F. ) ;
#26381 = AXIS2_PLACEMENT_3D ( 'NONE', #12839, #22151, #3995 ) ;
#26382 = FACE_OUTER_BOUND ( 'NONE', #15737, .T. ) ;
#26383 = CARTESIAN_POINT ( 'NONE',  ( -2.000000000000008882, 3.464101615137750390, -2.450000000000000622 ) ) ;
#26384 = CARTESIAN_POINT ( 'NONE',  ( 25.00000000000000000, 2.516649172247811061E-16, -2.055000000000000160 ) ) ;
#26385 = ORIENTED_EDGE ( 'NONE', *, *, #7945, .F. ) ;
#26386 = ORIENTED_EDGE ( 'NONE', *, *, #783, .T. ) ;
#26387 = CARTESIAN_POINT ( 'NONE',  ( 11.22373969136065242, 9.091953032947756697, -17.24166845096988609 ) ) ;
#26388 = PRESENTATION_LAYER_ASSIGNMENT (  '', '', ( #2445 ) ) ;
#26389 = CARTESIAN_POINT ( 'NONE',  ( 24.01770293978927384, -9.123702295727731837, -14.45939194930751448 ) ) ;
#26390 = CARTESIAN_POINT ( 'NONE',  ( 20.97149233804390533, -0.06858483505933390956, -19.21322127741759189 ) ) ;
#26391 = DIRECTION ( 'NONE',  ( 0.5877852522924731371, 0.000000000000000000, 0.8090169943749474513 ) ) ;
#26392 = DIRECTION ( 'NONE',  ( -0.9510565162951536422, 0.000000000000000000, -0.3090169943749472292 ) ) ;
#26393 = CARTESIAN_POINT ( 'NONE',  ( 164.5152310637604671, -1.999999999999972244, -11.28819510263909542 ) ) ;
#26394 = ADVANCED_FACE ( 'NONE', ( #7049 ), #18940, .T. ) ;
#26395 = ADVANCED_FACE ( 'NONE', ( #9621 ), #16339, .T. ) ;
#26396 = CARTESIAN_POINT ( 'NONE',  ( 139.7287565553230309, -10.00000000000000533, -7.839745962155603820 ) ) ;
#26397 = LINE ( 'NONE', #7758, #6002 ) ;
#26398 = DIRECTION ( 'NONE',  ( 0.3090169943749472292, 8.338696094057992503E-17, -0.9510565162951536422 ) ) ;
#26399 = CONICAL_SURFACE ( 'NONE', #5917, 8.000000000000007105, 1.047197551196596077 ) ;
#26400 = CARTESIAN_POINT ( 'NONE',  ( 158.6922820468853388, -4.999999999999975131, -6.413161187712876909 ) ) ;
#26401 = LINE ( 'NONE', #17223, #23595 ) ;
#26402 = CARTESIAN_POINT ( 'NONE',  ( 10.73134732381016576, 15.26288385841099249, -17.22756371135774245 ) ) ;
#26403 = CARTESIAN_POINT ( 'NONE',  ( 35.12509383387676820, -20.28195432802065312, -20.22992657050740917 ) ) ;
#26404 = ORIENTED_EDGE ( 'NONE', *, *, #19402, .F. ) ;
#26405 = CARTESIAN_POINT ( 'NONE',  ( 13.37841584274036855, 7.625425322794393779, -15.70882597216490240 ) ) ;
#26406 = CARTESIAN_POINT ( 'NONE',  ( 26.31132954256896639, -3.159408024760113509, -14.81636702655834803 ) ) ;
#26407 = CARTESIAN_POINT ( 'NONE',  ( 12.86479781618563045, 9.514843269526567227, -16.11816302316177030 ) ) ;
#26408 = FACE_BOUND ( 'NONE', #3867, .T. ) ;
#26409 = ORIENTED_EDGE ( 'NONE', *, *, #1549, .T. ) ;
#26410 = ORIENTED_EDGE ( 'NONE', *, *, #13817, .T. ) ;
#26411 = ORIENTED_EDGE ( 'NONE', *, *, #24318, .F. ) ;
#26412 = CARTESIAN_POINT ( 'NONE',  ( 11.47079713067724782, 9.278817116560638567, -15.86177209170659275 ) ) ;
#26413 = CARTESIAN_POINT ( 'NONE',  ( 136.1922820468854241, -1.999999999999980016, -19.40354224447947473 ) ) ;
#26414 = CARTESIAN_POINT ( 'NONE',  ( 12.39803340617553928, 8.535179507765855433, -15.21071672276548625 ) ) ;
#26415 = DIRECTION ( 'NONE',  ( -1.000000000000000000, 0.000000000000000000, 0.000000000000000000 ) ) ;
#26416 = ORIENTED_EDGE ( 'NONE', *, *, #19365, .T. ) ;
#26417 = PLANE ( 'NONE',  #17855 ) ;
#26418 = ORIENTED_EDGE ( 'NONE', *, *, #22496, .T. ) ;
#26419 = CARTESIAN_POINT ( 'NONE',  ( 12.02786405831828986, 9.316892843345049968, -16.69140843421181231 ) ) ;
#26420 = VERTEX_POINT ( 'NONE', #9318 ) ;
#26421 = CARTESIAN_POINT ( 'NONE',  ( 30.78206665311622459, -10.11802168058175511, -15.10569088962643036 ) ) ;
#26422 = CARTESIAN_POINT ( 'NONE',  ( 27.89048517759004753, -11.43816616845083445, -12.79876095355805177 ) ) ;
#26423 = CARTESIAN_POINT ( 'NONE',  ( 16.78426473046523526, 10.16049046829612479, -19.50779498702920378 ) ) ;
#26424 = CARTESIAN_POINT ( 'NONE',  ( 25.00000000000001066, 55.00000000000000711, 29.99999999999998579 ) ) ;
#26425 = ORIENTED_EDGE ( 'NONE', *, *, #21482, .T. ) ;
#26426 = VERTEX_POINT ( 'NONE', #21078 ) ;
#26427 = CARTESIAN_POINT ( 'NONE',  ( 137.0152310637606092, -10.00000000000000533, -32.93883019725009120 ) ) ;
#26428 = APPLICATION_PROTOCOL_DEFINITION ( 'draft international standard', 'automotive_design', 1998, #16700 ) ;
#26429 = EDGE_LOOP ( 'NONE', ( #19785, #27377, #23482, #24646 ) ) ;
#26430 = CARTESIAN_POINT ( 'NONE',  ( 22.11273855634006935, 3.201273238686522138, -15.95510540678940181 ) ) ;
#26431 = CARTESIAN_POINT ( 'NONE',  ( 15.41431293496917121, 3.575304669039410133, -17.09800041271234150 ) ) ;
#26432 = ADVANCED_FACE ( 'NONE', ( #21376 ), #18643, .T. ) ;
#26433 = EDGE_CURVE ( 'NONE', #21693, #7797, #185, .T. ) ;
#26434 = ADVANCED_FACE ( 'NONE', ( #9772 ), #18788, .T. ) ;
#26435 = LINE ( 'NONE', #19388, #16391 ) ;
#26436 = EDGE_CURVE ( 'NONE', #6491, #29341, #25818, .T. ) ;
#26437 = CARTESIAN_POINT ( 'NONE',  ( 1.318516776095787435, 3.857556137907067750, 4.982961509259709006E-15 ) ) ;
#26438 = VECTOR ( 'NONE', #13896, 1000.000000000000000 ) ;
#26439 = DIRECTION ( 'NONE',  ( 0.000000000000000000, 0.000000000000000000, 1.000000000000000000 ) ) ;
#26440 = FACE_OUTER_BOUND ( 'NONE', #26696, .T. ) ;
#26441 = FACE_OUTER_BOUND ( 'NONE', #9463, .T. ) ;
#26442 = DIRECTION ( 'NONE',  ( -1.000000000000000000, -4.440892098500622217E-16, 0.000000000000000000 ) ) ;
#26443 = CARTESIAN_POINT ( 'NONE',  ( 12.01759036229752553, 10.68391031264169122, -15.41792755180196473 ) ) ;
#26444 = DIRECTION ( 'NONE',  ( 0.3090169943749472292, 8.338696094057992503E-17, -0.9510565162951536422 ) ) ;
#26445 = PLANE ( 'NONE',  #22703 ) ;
#26446 = ORIENTED_EDGE ( 'NONE', *, *, #27767, .F. ) ;
#26447 = CARTESIAN_POINT ( 'NONE',  ( 11.48890098693651396, 9.204103201752445784, -15.85365151319587440 ) ) ;
#26448 = VERTEX_POINT ( 'NONE', #26576 ) ;
#26449 = VECTOR ( 'NONE', #6568, 1000.000000000000000 ) ;
#26450 = CARTESIAN_POINT ( 'NONE',  ( 16.24840684054896656, 4.149509756678782857, -16.79736725456322688 ) ) ;
#26451 = DIRECTION ( 'NONE',  ( -0.8090169943749474513, -2.183098979609982436E-16, 0.5877852522924731371 ) ) ;
#26452 = CARTESIAN_POINT ( 'NONE',  ( 136.1922820468854241, -4.999999999999980460, -13.59645775552055547 ) ) ;
#26453 = ORIENTED_EDGE ( 'NONE', *, *, #16728, .T. ) ;
#26454 = CYLINDRICAL_SURFACE ( 'NONE', #9244, 4.250000000000000000 ) ;
#26455 = EDGE_LOOP ( 'NONE', ( #28105, #16369, #5222, #8507, #2435 ) ) ;
#26456 = FACE_OUTER_BOUND ( 'NONE', #25318, .T. ) ;
#26457 = VERTEX_POINT ( 'NONE', #10069 ) ;
#26458 = CARTESIAN_POINT ( 'NONE',  ( 12.83227841057820484, 9.540504573332061256, -16.14102835882348330 ) ) ;
#26459 = ORIENTED_EDGE ( 'NONE', *, *, #26147, .F. ) ;
#26460 = CARTESIAN_POINT ( 'NONE',  ( 36.51492826578181194, -21.03327392953103825, -18.93061234292109063 ) ) ;
#26461 = CARTESIAN_POINT ( 'NONE',  ( 16.79143122783437292, 7.330551994622505063, -14.54187356113185103 ) ) ;
#26462 = ORIENTED_EDGE ( 'NONE', *, *, #14909, .F. ) ;
#26463 = ORIENTED_EDGE ( 'NONE', *, *, #19476, .T. ) ;
#26464 = PLANE ( 'NONE',  #7701 ) ;
#26465 = VECTOR ( 'NONE', #5624, 1000.000000000000000 ) ;
#26466 = CARTESIAN_POINT ( 'NONE',  ( 18.00441060066494003, 9.543425513107552050, -19.87907960298149490 ) ) ;
#26467 = EDGE_LOOP ( 'NONE', ( #27881, #13144, #3188, #20197 ) ) ;
#26468 = CARTESIAN_POINT ( 'NONE',  ( 136.1922820468854241, -10.00000000000000533, -2.083034168790677043 ) ) ;
#26469 =( NAMED_UNIT ( * ) SI_UNIT ( $, .STERADIAN. ) SOLID_ANGLE_UNIT ( ) );
#26470 = CARTESIAN_POINT ( 'NONE',  ( 26.86433939054618492, -2.362129714094441724, -16.96571632802953644 ) ) ;
#26471 = CARTESIAN_POINT ( 'NONE',  ( 18.18253756980838531, -1.899343836538245789, -17.94647550410194370 ) ) ;
#26472 = ORIENTED_EDGE ( 'NONE', *, *, #14439, .T. ) ;
#26473 = DIRECTION ( 'NONE',  ( -2.698458740408365879E-16, 1.000000000000000000, 0.000000000000000000 ) ) ;
#26475 = VERTEX_POINT ( 'NONE', #10679 ) ;
#26474 = EDGE_CURVE ( 'NONE', #12566, #25860, #29193, .T. ) ;
#26476 = CARTESIAN_POINT ( 'NONE',  ( 143.6922820468854241, -10.00000000000000355, -6.413161187712876909 ) ) ;
#26477 = APPLICATION_CONTEXT ( 'automotive_design' ) ;
#26478 = LINE ( 'NONE', #19428, #18685 ) ;
#26479 = LINE ( 'NONE', #2988, #14898 ) ;
#26480 = DIRECTION ( 'NONE',  ( -0.5877852522924731371, -1.586114251531760235E-16, 0.8090169943749474513 ) ) ;
#26481 = CARTESIAN_POINT ( 'NONE',  ( 13.00000000000000178, -2.870178842070716726E-15, 23.00000000000000000 ) ) ;
#26482 = AXIS2_PLACEMENT_3D ( 'NONE', #13086, #12784, #15528 ) ;
#26483 = CARTESIAN_POINT ( 'NONE',  ( 11.65548303173490652, 8.849831895876286936, -15.75351705932409985 ) ) ;
#26484 = CARTESIAN_POINT ( 'NONE',  ( 25.51035504519657593, -9.958856436819656821, -16.28203429854516315 ) ) ;
#26485 = CARTESIAN_POINT ( 'NONE',  ( 26.20148740379470453, -2.166401353139026487, -14.75472287570676322 ) ) ;
#26487 = VERTEX_POINT ( 'NONE', #3088 ) ;
#26486 = CARTESIAN_POINT ( 'NONE',  ( 31.63980255171021483, -10.89810845426378982, -15.52824638758754183 ) ) ;
#26488 = CARTESIAN_POINT ( 'NONE',  ( 169.5152310637604671, -9.999999999999996447, -11.28819510263909542 ) ) ;
#26489 = CARTESIAN_POINT ( 'NONE',  ( 161.1922820468853388, -1.999999999999973133, -10.74328820663507678 ) ) ;
#26490 = DIRECTION ( 'NONE',  ( 1.000000000000000000, 2.698458740408365879E-16, -1.110223024625156540E-16 ) ) ;
#26491 = CARTESIAN_POINT ( 'NONE',  ( 167.0152310637605240, -1.999999999999970468, -34.70218595412750773 ) ) ;
#26492 = CARTESIAN_POINT ( 'NONE',  ( -20.00000000000017053, 34.64101615137744972, 4.999999999999998224 ) ) ;
#26493 = DIRECTION ( 'NONE',  ( -0.5877852522924731371, -1.586114251531760235E-16, 0.8090169943749474513 ) ) ;
#26494 = CARTESIAN_POINT ( 'NONE',  ( 23.66601916330066402, 2.199037240492611733, -18.57254039386976885 ) ) ;
#26495 = ORIENTED_EDGE ( 'NONE', *, *, #2108, .T. ) ;
#26496 = DIRECTION ( 'NONE',  ( 0.8191520442889943521, 3.637765840953626539E-16, 0.5735764363510424957 ) ) ;
#26497 = CARTESIAN_POINT ( 'NONE',  ( 12.26681336913932974, 9.540941834721429871, -15.31486507153535648 ) ) ;
#26498 = EDGE_CURVE ( 'NONE', #16948, #17144, #3375, .T. ) ;
#26499 = DIRECTION ( 'NONE',  ( 0.000000000000000000, 0.000000000000000000, -1.000000000000000000 ) ) ;
#26500 = DIRECTION ( 'NONE',  ( -1.110223024625156540E-16, 0.000000000000000000, -1.000000000000000000 ) ) ;
#26501 = CARTESIAN_POINT ( 'NONE',  ( 25.31619048431776875, -0.2099727537683927225, -15.56338435260822628 ) ) ;
#26502 = CARTESIAN_POINT ( 'NONE',  ( 17.45108151888110726, 3.014897074772306507, -13.47014999590450479 ) ) ;
#26503 = ORIENTED_EDGE ( 'NONE', *, *, #1931, .T. ) ;
#26504 = CARTESIAN_POINT ( 'NONE',  ( 34.75406370242679799, -18.61511248754081294, -20.11778113987843852 ) ) ;
#26505 = FILL_AREA_STYLE ('',( #8313 ) ) ;
#26506 = CARTESIAN_POINT ( 'NONE',  ( 26.73315660230872837, -4.509142541826837380, -13.49646658189591619 ) ) ;
#26507 = CARTESIAN_POINT ( 'NONE',  ( 24.91205307904067112, 1.131441846345163427, -15.76301496618838627 ) ) ;
#26508 = VECTOR ( 'NONE', #10611, 1000.000000000000000 ) ;
#26509 = ADVANCED_FACE ( 'NONE', ( #1233 ), #26734, .T. ) ;
#26510 = CARTESIAN_POINT ( 'NONE',  ( 23.22413189157496305, -7.367447486509826504, -15.63851824576001981 ) ) ;
#26511 = ORIENTED_EDGE ( 'NONE', *, *, #295, .T. ) ;
#26512 = FACE_OUTER_BOUND ( 'NONE', #4219, .T. ) ;
#26513 = VERTEX_POINT ( 'NONE', #17541 ) ;
#26514 = ORIENTED_EDGE ( 'NONE', *, *, #1379, .F. ) ;
#26515 = DIRECTION ( 'NONE',  ( 0.000000000000000000, 0.000000000000000000, 1.000000000000000000 ) ) ;
#26516 = CARTESIAN_POINT ( 'NONE',  ( -31.74999999999995737, 0.000000000000000000, 0.000000000000000000 ) ) ;
#26517 = DIRECTION ( 'NONE',  ( 0.5877852522924731371, 0.000000000000000000, 0.8090169943749474513 ) ) ;
#26518 = CARTESIAN_POINT ( 'NONE',  ( 18.47844294452917424, 10.16049799425131361, -18.92511192449534718 ) ) ;
#26519 = CARTESIAN_POINT ( 'NONE',  ( 35.88208498122789791, -19.19024427843809733, -20.38849413606966010 ) ) ;
#26520 = CARTESIAN_POINT ( 'NONE',  ( 9.926830210242822972, 16.35964622367879784, -16.50025672554925293 ) ) ;
#26521 = CONICAL_SURFACE ( 'NONE', #27051, 4.187999999999997947, 0.7853981633974482790 ) ;
#26522 = CARTESIAN_POINT ( 'NONE',  ( 173.6922820468853388, -4.999999999999970690, -26.58683881228715862 ) ) ;
#26523 = CARTESIAN_POINT ( 'NONE',  ( 96.69761215121324938, -4.999999999999991118, 70.25492758442437946 ) ) ;
#26524 = CARTESIAN_POINT ( 'NONE',  ( 12.00785540763395254, 9.408655069060824161, -16.69968271487400813 ) ) ;
#26525 = CARTESIAN_POINT ( 'NONE',  ( 104.5111766707794203, -4.999999999999988454, 75.93181450320298609 ) ) ;
#26526 = DIRECTION ( 'NONE',  ( -0.5877852522924731371, -1.586114251531760235E-16, 0.8090169943749474513 ) ) ;
#26527 = EDGE_CURVE ( 'NONE', #2080, #23514, #14941, .T. ) ;
#26528 = EDGE_CURVE ( 'NONE', #26028, #29734, #26899, .T. ) ;
#26529 = ORIENTED_EDGE ( 'NONE', *, *, #29988, .F. ) ;
#26530 = DIRECTION ( 'NONE',  ( 0.000000000000000000, 0.000000000000000000, 1.000000000000000000 ) ) ;
#26531 = CARTESIAN_POINT ( 'NONE',  ( -4.000000000000001776, 2.309401076758532678, -2.092734410091829034 ) ) ;
#26532 = EDGE_CURVE ( 'NONE', #21981, #5728, #5359, .T. ) ;
#26533 = DIRECTION ( 'NONE',  ( -2.698458740408365879E-16, 1.000000000000000000, 0.000000000000000000 ) ) ;
#26534 = ORIENTED_EDGE ( 'NONE', *, *, #7572, .F. ) ;
#26535 = B_SPLINE_CURVE_WITH_KNOTS ( 'NONE', 3,
 ( #9553, #11996, #714, #17042, #9703, #16742 ),
 .UNSPECIFIED., .F., .F.,
 ( 4, 2, 4 ),
 ( 0.006456566858647387955, 0.007625406818786661239, 0.008794246778925934524 ),
 .UNSPECIFIED. ) ;
#26536 = EDGE_LOOP ( 'NONE', ( #16640, #24114, #18574, #19380 ) ) ;
#26537 = CARTESIAN_POINT ( 'NONE',  ( 11.86544027865023843, 7.919735734555668039, -16.84125344233394372 ) ) ;
#26538 = ORIENTED_EDGE ( 'NONE', *, *, #12270, .F. ) ;
#26539 = CARTESIAN_POINT ( 'NONE',  ( 25.72097854023329688, -11.95459465090917917, -18.51508836554082293 ) ) ;
#26540 = CARTESIAN_POINT ( 'NONE',  ( 19.39248696316839116, -1.610358169686434193, -16.91126230894791860 ) ) ;
#26541 = CARTESIAN_POINT ( 'NONE',  ( 103.4180702440655324, -4.999999999999989342, -75.13762619655935282 ) ) ;
#26542 = CARTESIAN_POINT ( 'NONE',  ( 3.999999999999998224, 2.309401076758477167, -2.450000000000000178 ) ) ;
#26543 = DIRECTION ( 'NONE',  ( 1.000000000000000000, 0.000000000000000000, 0.000000000000000000 ) ) ;
#26544 = VECTOR ( 'NONE', #22216, 999.9999999999998863 ) ;
#26545 = VERTEX_POINT ( 'NONE', #12815 ) ;
#26546 = CARTESIAN_POINT ( 'NONE',  ( 144.5152310637606092, -1.999999999999977129, -28.60870317832789311 ) ) ;
#26547 = LINE ( 'NONE', #21951, #8907 ) ;
#26548 = LINE ( 'NONE', #17069, #18488 ) ;
#26549 = PLANE ( 'NONE',  #10260 ) ;
#26550 = LINE ( 'NONE', #17072, #22129 ) ;
#26551 = VECTOR ( 'NONE', #17973, 1000.000000000000000 ) ;
#26552 = CARTESIAN_POINT ( 'NONE',  ( 12.06596557120094992, 9.177570865404522493, -16.67295095431955332 ) ) ;
#26553 = CARTESIAN_POINT ( 'NONE',  ( 35.54859390953723874, -22.18451583373416014, -15.00000000000000000 ) ) ;
#26554 = VERTEX_POINT ( 'NONE', #12662 ) ;
#26555 = CARTESIAN_POINT ( 'NONE',  ( 9.109746387114286748, 16.19414013429083710, -17.05597298747021640 ) ) ;
#26556 = CARTESIAN_POINT ( 'NONE',  ( 25.77659985377941254, -6.250509680199615836, -13.67467641272277312 ) ) ;
#26557 = CARTESIAN_POINT ( 'NONE',  ( 12.83236877538120524, 9.540106609504201529, -16.14098973436422568 ) ) ;
#26558 = FACE_BOUND ( 'NONE', #29275, .T. ) ;
#26559 = EDGE_LOOP ( 'NONE', ( #11606, #23260, #27304, #22724 ) ) ;
#26560 = EDGE_CURVE ( 'NONE', #15160, #25802, #22810, .T. ) ;
#26561 = VERTEX_POINT ( 'NONE', #21980 ) ;
#26562 = LINE ( 'NONE', #17377, #29718 ) ;
#26563 = EDGE_CURVE ( 'NONE', #10204, #22806, #28745, .T. ) ;
#26564 = CIRCLE ( 'NONE', #15819, 4.250000000000000000 ) ;
#26565 = CARTESIAN_POINT ( 'NONE',  ( 11.50832337395308436, 9.139936167900076569, -15.84372008594036885 ) ) ;
#26566 = LINE ( 'NONE', #21971, #3787 ) ;
#26567 = EDGE_CURVE ( 'NONE', #22102, #2770, #12965, .T. ) ;
#26568 = EDGE_LOOP ( 'NONE', ( #9947, #6670, #18707 ) ) ;
#26569 = DIRECTION ( 'NONE',  ( -0.8090169943749474513, -2.183098979609982436E-16, -0.5877852522924731371 ) ) ;
#26570 = VERTEX_POINT ( 'NONE', #12506 ) ;
#26571 = CARTESIAN_POINT ( 'NONE',  ( 12.72883512080982804, 8.524354266104470668, -16.21679389071614352 ) ) ;
#26572 = VERTEX_POINT ( 'NONE', #28902 ) ;
#26573 = CARTESIAN_POINT ( 'NONE',  ( 19.13824544459052035, 4.841912194177635520, -12.94453987625427160 ) ) ;
#26574 = CARTESIAN_POINT ( 'NONE',  ( 27.89048517759004753, -11.43816616845083445, -12.79876095355805177 ) ) ;
#26575 = ORIENTED_EDGE ( 'NONE', *, *, #16024, .F. ) ;
#26576 = CARTESIAN_POINT ( 'NONE',  ( 152.0152310637605524, -4.999999999999976907, -26.04193191628311155 ) ) ;
#26577 = ORIENTED_EDGE ( 'NONE', *, *, #8617, .T. ) ;
#26578 = CARTESIAN_POINT ( 'NONE',  ( 36.54859390953724585, -22.18451583373416014, -17.22552805718784441 ) ) ;
#26579 = SHAPE_DEFINITION_REPRESENTATION ( #12487, #24148 ) ;
#26580 = ORIENTED_EDGE ( 'NONE', *, *, #17873, .F. ) ;
#26581 = CARTESIAN_POINT ( 'NONE',  ( 19.42159491456138554, 2.195880709831018684, -14.63272625841335106 ) ) ;
#26582 = CARTESIAN_POINT ( 'NONE',  ( 15.87806330829146617, 7.947701475055697351, -19.83831759000646855 ) ) ;
#26583 = DIRECTION ( 'NONE',  ( 0.8191520442889902442, 4.640937770007129962E-16, -0.5735764363510482688 ) ) ;
#26584 = LINE ( 'NONE', #28909, #25967 ) ;
#26585 = VECTOR ( 'NONE', #19245, 1000.000000000000000 ) ;
#26586 = LINE ( 'NONE', #11501, #25743 ) ;
#26587 = DIRECTION ( 'NONE',  ( 0.000000000000000000, 0.000000000000000000, -1.000000000000000000 ) ) ;
#26588 = CARTESIAN_POINT ( 'NONE',  ( 13.77718166750865869, 8.859676595473324312, -15.39100258941132182 ) ) ;
#26589 = CARTESIAN_POINT ( 'NONE',  ( 93.84789618117305565, -4.999999999999992006, 68.18448773945412711 ) ) ;
#26590 = CARTESIAN_POINT ( 'NONE',  ( 12.27644674946102832, 9.496504630232381672, -15.31090095340427304 ) ) ;
#26591 = FACE_OUTER_BOUND ( 'NONE', #14152, .T. ) ;
#26592 = VERTEX_POINT ( 'NONE', #22280 ) ;
#26593 = CARTESIAN_POINT ( 'NONE',  ( 0.000000000000000000, 0.000000000000000000, -15.00000000000000000 ) ) ;
#26594 = VERTEX_POINT ( 'NONE', #15092 ) ;
#26595 = CARTESIAN_POINT ( 'NONE',  ( 11.47327446659168615, 9.267463859335506982, -15.86074700677745852 ) ) ;
#26596 = ORIENTED_EDGE ( 'NONE', *, *, #26108, .F. ) ;
#26597 = EDGE_CURVE ( 'NONE', #10096, #27716, #17099, .T. ) ;
#26598 = CARTESIAN_POINT ( 'NONE',  ( 10.76353862942338147, 8.717528283631100550, -16.36374602157236779 ) ) ;
#26599 = LINE ( 'NONE', #26151, #16580 ) ;
#26600 = DIRECTION ( 'NONE',  ( -1.000000000000000000, 0.000000000000000000, 0.000000000000000000 ) ) ;
#26601 = EDGE_CURVE ( 'NONE', #16501, #21693, #10371, .T. ) ;
#26602 = EDGE_CURVE ( 'NONE', #20364, #12263, #19989, .T. ) ;
#26603 = VERTEX_POINT ( 'NONE', #29359 ) ;
#26604 = CARTESIAN_POINT ( 'NONE',  ( 141.1922820468854525, -10.00000000000000533, -22.25671179336495697 ) ) ;
#26605 = ORIENTED_EDGE ( 'NONE', *, *, #487, .T. ) ;
#26606 = CARTESIAN_POINT ( 'NONE',  ( 139.5152310637606092, -1.999999999999978684, -19.94844914048349338 ) ) ;
#26607 = EDGE_CURVE ( 'NONE', #25583, #27966, #7934, .T. ) ;
#26608 = ORIENTED_EDGE ( 'NONE', *, *, #6856, .T. ) ;
#26609 = CARTESIAN_POINT ( 'NONE',  ( 12.18385343395297049, 12.51426234204957844, -16.40917503585457737 ) ) ;
#26610 = ORIENTED_EDGE ( 'NONE', *, *, #10863, .T. ) ;
#26612 = CARTESIAN_POINT ( 'NONE',  ( 34.52649160559821695, -12.12091213808323964, -18.92441241263726326 ) ) ;
#26611 = AXIS2_PLACEMENT_3D ( 'NONE', #4846, #3183, #7741 ) ;
#26613 = CARTESIAN_POINT ( 'NONE',  ( 19.11618317516819587, 7.271703427217982352, -19.10559232466456692 ) ) ;
#26614 = ORIENTED_EDGE ( 'NONE', *, *, #12374, .F. ) ;
#26615 = AXIS2_PLACEMENT_3D ( 'NONE', #29765, #15795, #11072 ) ;
#26616 = LINE ( 'NONE', #811, #20847 ) ;
#26617 = CARTESIAN_POINT ( 'NONE',  ( 19.14398323884976350, 7.495936751868839565, -14.71076302495156263 ) ) ;
#26618 = DIRECTION ( 'NONE',  ( 0.5877852522924731371, 0.000000000000000000, 0.8090169943749474513 ) ) ;
#26619 = CARTESIAN_POINT ( 'NONE',  ( -4.000000000000008882, 6.928203230275508773, -5.000000000000000888 ) ) ;
#26620 = ORIENTED_EDGE ( 'NONE', *, *, #14950, .T. ) ;
#26621 = SURFACE_STYLE_FILL_AREA ( #17286 ) ;
#26622 = CARTESIAN_POINT ( 'NONE',  ( 19.79269262995316936, -1.159804626089355084, -18.29502107036499581 ) ) ;
#26623 = CARTESIAN_POINT ( 'NONE',  ( 18.89783927354708837, -1.194421563772924078, -19.46960211947776287 ) ) ;
#26624 = VERTEX_POINT ( 'NONE', #3522 ) ;
#26625 = ORIENTED_EDGE ( 'NONE', *, *, #5290, .T. ) ;
#26626 = EDGE_LOOP ( 'NONE', ( #16790, #18282 ) ) ;
#26627 = VECTOR ( 'NONE', #17337, 1000.000000000000000 ) ;
#26628 = DIRECTION ( 'NONE',  ( 0.5877852522924731371, 1.586114251531760728E-16, -0.8090169943749474513 ) ) ;
#26629 = VECTOR ( 'NONE', #29183, 1000.000000000000000 ) ;
#26630 = DIRECTION ( 'NONE',  ( 1.000000000000000000, 2.698458740408365879E-16, -1.110223024625156540E-16 ) ) ;
#26631 = DIRECTION ( 'NONE',  ( 0.5877852522924731371, 1.586114251531760728E-16, -0.8090169943749474513 ) ) ;
#26632 = CARTESIAN_POINT ( 'NONE',  ( 0.000000000000000000, 0.000000000000000000, -2.450000000000000622 ) ) ;
#26633 = VECTOR ( 'NONE', #25566, 1000.000000000000000 ) ;
#26634 = LINE ( 'NONE', #16850, #30035 ) ;
#26635 = AXIS2_PLACEMENT_3D ( 'NONE', #14703, #24046, #17012 ) ;
#26636 = CARTESIAN_POINT ( 'NONE',  ( 11.92109019680886206, 8.606374460406147620, -15.56934379943068336 ) ) ;
#26637 = CARTESIAN_POINT ( 'NONE',  ( 27.28761988882141765, -9.265112451392095494, -14.04413049427448001 ) ) ;
#26638 = CARTESIAN_POINT ( 'NONE',  ( 22.98083118076628040, -7.181321033737746440, -13.97658420854277850 ) ) ;
#26639 = ORIENTED_EDGE ( 'NONE', *, *, #21098, .T. ) ;
#26640 = CARTESIAN_POINT ( 'NONE',  ( 0.000000000000000000, 0.000000000000000000, 0.000000000000000000 ) ) ;
#26641 = CARTESIAN_POINT ( 'NONE',  ( 0.000000000000000000, 0.000000000000000000, -5.000000000000000888 ) ) ;
#26642 = CARTESIAN_POINT ( 'NONE',  ( 1.214306433183764966E-14, 4.618802153517016507, -0.3572655899081716435 ) ) ;
#26643 = CARTESIAN_POINT ( 'NONE',  ( 160.0000000000000000, -10.00000000000000000, -186.4312945166758482 ) ) ;
#26644 = EDGE_CURVE ( 'NONE', #8141, #22102, #17390, .T. ) ;
#26645 = CARTESIAN_POINT ( 'NONE',  ( 141.1922820468854525, -4.999999999999978684, -28.06379628232387446 ) ) ;
#26646 = FILL_AREA_STYLE ('',( #22348 ) ) ;
#26647 = CARTESIAN_POINT ( 'NONE',  ( 20.22088415693689356, -1.238650738454883493, -19.72259765018230482 ) ) ;
#26648 = ORIENTED_EDGE ( 'NONE', *, *, #1762, .T. ) ;
#26649 = CYLINDRICAL_SURFACE ( 'NONE', #14418, 4.000000000000003553 ) ;
#26650 = EDGE_CURVE ( 'NONE', #9309, #17686, #26275, .T. ) ;
#26651 = CARTESIAN_POINT ( 'NONE',  ( 10.75323949831978432, 16.48238454209313630, -15.94078111022350619 ) ) ;
#26652 = CARTESIAN_POINT ( 'NONE',  ( 4.250000000000003553, 1.887379141862766119E-15, -5.000000000000000888 ) ) ;
#26653 = LINE ( 'NONE', #21899, #17121 ) ;
#26654 = VECTOR ( 'NONE', #13521, 1000.000000000000000 ) ;
#26655 = CARTESIAN_POINT ( 'NONE',  ( 24.52797215547132836, -1.897736678990579184, -19.26084780660264073 ) ) ;
#26656 = LINE ( 'NONE', #10598, #24749 ) ;
#26657 = CARTESIAN_POINT ( 'NONE',  ( 20.63001478507949926, 2.108136148055946180, -20.13827832349858937 ) ) ;
#26658 = ORIENTED_EDGE ( 'NONE', *, *, #21002, .T. ) ;
#26659 = FACE_OUTER_BOUND ( 'NONE', #20442, .T. ) ;
#26660 = SHAPE_REPRESENTATION_RELATIONSHIP ( 'NONE' , 'NONE' ,  #24148, #29596 ) ;
#26661 = CARTESIAN_POINT ( 'NONE',  ( 31.26470888135608206, -7.466309307788507432, -16.51192723299172727 ) ) ;
#26662 = AXIS2_PLACEMENT_3D ( 'NONE', #21853, #3549, #12841 ) ;
#26663 = CARTESIAN_POINT ( 'NONE',  ( 19.75542110462093959, -4.861139154975066212, -17.07234110396024818 ) ) ;
#26664 = AXIS2_PLACEMENT_3D ( 'NONE', #11287, #3829, #6267 ) ;
#26665 = ORIENTED_EDGE ( 'NONE', *, *, #2351, .T. ) ;
#26666 = CARTESIAN_POINT ( 'NONE',  ( 25.07290406138036687, -9.006318079059196791, -17.79994936451110732 ) ) ;
#26667 = PRODUCT_DEFINITION_SHAPE ( 'NONE', 'NONE',  #735 ) ;
#26668 = ORIENTED_EDGE ( 'NONE', *, *, #22109, .T. ) ;
#26669 = DIRECTION ( 'NONE',  ( -2.698458740408365879E-16, 1.000000000000000000, 0.000000000000000000 ) ) ;
#26670 = EDGE_LOOP ( 'NONE', ( #22200, #8292, #3669, #19610 ) ) ;
#26671 = ADVANCED_FACE ( 'NONE', ( #14643 ), #5771, .T. ) ;
#26672 = ORIENTED_EDGE ( 'NONE', *, *, #29517, .F. ) ;
#26673 = CARTESIAN_POINT ( 'NONE',  ( 152.0152310637604955, -1.999999999999975797, -8.721423840594312082 ) ) ;
#26674 = CARTESIAN_POINT ( 'NONE',  ( 172.0152310637604103, -9.999999999999996447, -8.721423840594312082 ) ) ;
#26675 = DIRECTION ( 'NONE',  ( -2.698458740408365879E-16, 1.000000000000000000, 0.000000000000000000 ) ) ;
#26676 = AXIS2_PLACEMENT_3D ( 'NONE', #18071, #16379, #22968 ) ;
#26677 = CARTESIAN_POINT ( 'NONE',  ( 15.17188473929424930, 6.803351907998973935, -20.50413427079521256 ) ) ;
#26678 = CARTESIAN_POINT ( 'NONE',  ( 33.54536560287652946, -10.49856191242287373, -18.63199441812703583 ) ) ;
#26679 = AXIS2_PLACEMENT_3D ( 'NONE', #4417, #16449, #18444 ) ;
#26680 = CARTESIAN_POINT ( 'NONE',  ( 11.40798482813988635, 9.566882342703072695, -15.88774718835883348 ) ) ;
#26681 = AXIS2_PLACEMENT_3D ( 'NONE', #8340, #19773, #17340 ) ;
#26682 = DIRECTION ( 'NONE',  ( -2.698458740408365879E-16, 1.000000000000000000, 0.000000000000000000 ) ) ;
#26683 = LINE ( 'NONE', #26523, #14879 ) ;
#26684 = CARTESIAN_POINT ( 'NONE',  ( 9.661887760751893595, 16.25480508276471525, -17.91458275280492884 ) ) ;
#26685 = PLANE ( 'NONE',  #13 ) ;
#26686 = LINE ( 'NONE', #28995, #23752 ) ;
#26687 = ORIENTED_EDGE ( 'NONE', *, *, #15969, .T. ) ;
#26688 = DIRECTION ( 'NONE',  ( 1.110223024625156540E-16, 2.995891024602366092E-32, 1.000000000000000000 ) ) ;
#26689 = LINE ( 'NONE', #15047, #14165 ) ;
#26690 = ORIENTED_EDGE ( 'NONE', *, *, #3171, .T. ) ;
#26691 = CARTESIAN_POINT ( 'NONE',  ( 13.00000000000001243, 55.00000000000000711, 23.00000000000000000 ) ) ;
#26692 = ORIENTED_EDGE ( 'NONE', *, *, #106, .T. ) ;
#26693 = ORIENTED_EDGE ( 'NONE', *, *, #5155, .T. ) ;
#26694 = ORIENTED_EDGE ( 'NONE', *, *, #9375, .F. ) ;
#26695 = CARTESIAN_POINT ( 'NONE',  ( 11.23176012633392595, 9.056260211165422902, -17.23826859254635835 ) ) ;
#26696 = EDGE_LOOP ( 'NONE', ( #28214, #10591, #13233, #8807 ) ) ;
#26697 = CARTESIAN_POINT ( 'NONE',  ( 32.47832896513632761, -9.914179286496517918, -13.92895715894296771 ) ) ;
#26698 = CARTESIAN_POINT ( 'NONE',  ( 26.88053589187069292, -12.95240298029966119, -14.33176627689639382 ) ) ;
#26699 = AXIS2_PLACEMENT_3D ( 'NONE', #2360, #4928, #21406 ) ;
#26700 = LINE ( 'NONE', #1200, #17947 ) ;
#26701 = LINE ( 'NONE', #28707, #12102 ) ;
#26702 = CARTESIAN_POINT ( 'NONE',  ( 173.6922820468853104, -1.999999999999970024, -17.92658477444275889 ) ) ;
#26703 = AXIS2_PLACEMENT_3D ( 'NONE', #23258, #8604, #27429 ) ;
#26704 = ORIENTED_EDGE ( 'NONE', *, *, #18656, .F. ) ;
#26705 = DIRECTION ( 'NONE',  ( -2.698458740408365879E-16, 1.000000000000000000, 0.000000000000000000 ) ) ;
#26706 = EDGE_CURVE ( 'NONE', #888, #16025, #11278, .T. ) ;
#26707 = CARTESIAN_POINT ( 'NONE',  ( 31.84774147790582433, -10.54213090804960018, -15.00000000011102763 ) ) ;
#26708 = B_SPLINE_CURVE_WITH_KNOTS ( 'NONE', 3,
 ( #11842, #25584, #27620, #4830, #23151, #7127 ),
 .UNSPECIFIED., .F., .F.,
 ( 4, 2, 4 ),
 ( 0.01291313371729458509, 0.01525081363757310911, 0.01758849355785163313 ),
 .UNSPECIFIED. ) ;
#26709 = EDGE_CURVE ( 'NONE', #8269, #29449, #20433, .T. ) ;
#26710 = CARTESIAN_POINT ( 'NONE',  ( 162.0152310637605240, -1.999999999999971800, -34.70218595412750773 ) ) ;
#26711 = DIRECTION ( 'NONE',  ( -2.698458740408365879E-16, 1.000000000000000000, 0.000000000000000000 ) ) ;
#26712 = B_SPLINE_CURVE_WITH_KNOTS ( 'NONE', 3,
 ( #9680, #16717, #18846, #12278, #694, #21596 ),
 .UNSPECIFIED., .F., .F.,
 ( 4, 2, 4 ),
 ( 0.002336974151641584615, 0.003500975885716457563, 0.004664977619791330077 ),
 .UNSPECIFIED. ) ;
#26713 = CARTESIAN_POINT ( 'NONE',  ( 13.12468173219994760, 8.571325198882655982, -15.91105655537220009 ) ) ;
#26714 = CARTESIAN_POINT ( 'NONE',  ( 35.54859390953724585, -22.18451583373416014, -17.78191007148576475 ) ) ;
#26715 = ORIENTED_EDGE ( 'NONE', *, *, #8459, .T. ) ;
#26716 = CARTESIAN_POINT ( 'NONE',  ( 9.113844519079130180, 16.17534557870975576, -17.05418121134841414 ) ) ;
#26717 = AXIS2_PLACEMENT_3D ( 'NONE', #1840, #15839, #8527 ) ;
#26718 = CARTESIAN_POINT ( 'NONE',  ( 24.95482030053459965, -6.624749414579512496, -13.76522253407564733 ) ) ;
#26719 = CARTESIAN_POINT ( 'NONE',  ( 12.76739998655820685, 9.838043466917183011, -16.16785800888773394 ) ) ;
#26720 = FACE_BOUND ( 'NONE', #11431, .T. ) ;
#26721 = ORIENTED_EDGE ( 'NONE', *, *, #30020, .T. ) ;
#26722 = AXIS2_PLACEMENT_3D ( 'NONE', #27082, #3858, #29232 ) ;
#26723 = FACE_OUTER_BOUND ( 'NONE', #2366, .T. ) ;
#26724 = CARTESIAN_POINT ( 'NONE',  ( 12.49742530276927610, 8.569573706352677789, -15.13222638044318735 ) ) ;
#26725 = DIRECTION ( 'NONE',  ( -0.9510565162951536422, 0.000000000000000000, -0.3090169943749472292 ) ) ;
#26726 = ORIENTED_EDGE ( 'NONE', *, *, #10661, .F. ) ;
#26727 = DIRECTION ( 'NONE',  ( -0.5877852522924731371, 0.000000000000000000, 0.8090169943749474513 ) ) ;
#26728 = EDGE_LOOP ( 'NONE', ( #6260, #29188, #8056, #9819 ) ) ;
#26729 = CARTESIAN_POINT ( 'NONE',  ( 12.84373479294319864, 8.511860559062048637, -16.13004233893675377 ) ) ;
#26730 = ORIENTED_EDGE ( 'NONE', *, *, #27431, .T. ) ;
#26731 = AXIS2_PLACEMENT_3D ( 'NONE', #44, #18654, #18798 ) ;
#26732 = CARTESIAN_POINT ( 'NONE',  ( 14.66608887309643272, 3.149405488550426568, -18.09902814372540192 ) ) ;
#26733 = CARTESIAN_POINT ( 'NONE',  ( 19.32227194923075331, 0.3423946635036635433, -13.32047942220886583 ) ) ;
#26734 = CYLINDRICAL_SURFACE ( 'NONE', #29680, 2.000000000000000000 ) ;
#26735 = ORIENTED_EDGE ( 'NONE', *, *, #28526, .F. ) ;
#26736 = CARTESIAN_POINT ( 'NONE',  ( 36.54460969663918490, -22.16661687567949457, -18.62492107750662029 ) ) ;
#26737 = APPLICATION_PROTOCOL_DEFINITION ( 'draft international standard', 'automotive_design', 1998, #13575 ) ;
#26738 = VERTEX_POINT ( 'NONE', #3822 ) ;
#26739 = CARTESIAN_POINT ( 'NONE',  ( 17.12833724908345800, 9.171387755021909172, -19.38714867094073213 ) ) ;
#26740 = VECTOR ( 'NONE', #27444, 1000.000000000000000 ) ;
#26741 = ORIENTED_EDGE ( 'NONE', *, *, #20160, .T. ) ;
#26742 = DIRECTION ( 'NONE',  ( -1.110223024625156540E-16, 0.000000000000000000, -1.000000000000000000 ) ) ;
#26743 = EDGE_CURVE ( 'NONE', #2635, #13495, #22897, .T. ) ;
#26744 = FACE_BOUND ( 'NONE', #8231, .T. ) ;
#26745 = EDGE_CURVE ( 'NONE', #10204, #846, #18439, .T. ) ;
#26746 = VECTOR ( 'NONE', #292, 1000.000000000000000 ) ;
#26747 = EDGE_CURVE ( 'NONE', #13010, #16269, #16003, .T. ) ;
#26748 = EDGE_CURVE ( 'NONE', #23709, #22459, #22343, .T. ) ;
#26749 = FACE_OUTER_BOUND ( 'NONE', #25953, .T. ) ;
#26750 = CARTESIAN_POINT ( 'NONE',  ( 33.35202879388211983, -12.33251541790028760, -19.68467382345759376 ) ) ;
#26751 = CARTESIAN_POINT ( 'NONE',  ( 134.5152310637605524, -10.00000000000000533, -21.71180489736090991 ) ) ;
#26752 = ORIENTED_EDGE ( 'NONE', *, *, #9628, .F. ) ;
#26753 = DIRECTION ( 'NONE',  ( 0.9510565162951536422, 2.566386769018988816E-16, 0.3090169943749472292 ) ) ;
#26754 = CARTESIAN_POINT ( 'NONE',  ( 12.26073475921635669, 9.568819114670704451, -15.31737879056614737 ) ) ;
#26755 = CARTESIAN_POINT ( 'NONE',  ( -5.000000000000000000, 0.000000000000000000, 23.00000000000000000 ) ) ;
#26756 = EDGE_LOOP ( 'NONE', ( #5653, #18699, #12507, #2727 ) ) ;
#26757 = DIRECTION ( 'NONE',  ( -0.9510565162951536422, -2.566386769018988323E-16, 0.3090169943749475623 ) ) ;
#26758 = ORIENTED_EDGE ( 'NONE', *, *, #10987, .F. ) ;
#26759 = CARTESIAN_POINT ( 'NONE',  ( 12.50162201464318557, 8.571418981294288031, -15.12888223836978341 ) ) ;
#26760 = ORIENTED_EDGE ( 'NONE', *, *, #18897, .F. ) ;
#26761 = CARTESIAN_POINT ( 'NONE',  ( 12.00353595525870887, 7.537035219234042849, -15.50727442731917272 ) ) ;
#26762 = DIRECTION ( 'NONE',  ( -0.9510565162951536422, -2.566386769018988816E-16, -0.3090169943749472292 ) ) ;
#26763 = CARTESIAN_POINT ( 'NONE',  ( 0.000000000000000000, 0.000000000000000000, -2.424599999999998978 ) ) ;
#26764 = ORIENTED_EDGE ( 'NONE', *, *, #19480, .T. ) ;
#26765 = EDGE_LOOP ( 'NONE', ( #16574, #5091, #13676, #11548, #15983 ) ) ;
#26766 = CARTESIAN_POINT ( 'NONE',  ( 151.1922820468854241, -10.00000000000000178, -22.25671179336496053 ) ) ;
#26767 = ORIENTED_EDGE ( 'NONE', *, *, #861, .F. ) ;
#26768 = CARTESIAN_POINT ( 'NONE',  ( 12.86616790684404421, 9.515247448762703897, -16.11708638872277177 ) ) ;
#26769 = VERTEX_POINT ( 'NONE', #6560 ) ;
#26770 = VECTOR ( 'NONE', #9671, 1000.000000000000000 ) ;
#26771 = CARTESIAN_POINT ( 'NONE',  ( 33.81279548071420038, -11.10283711904122050, -17.43625070980107594 ) ) ;
#26772 = CARTESIAN_POINT ( 'NONE',  ( 19.38992137333195842, 2.881095379261479739, -20.30776781288435373 ) ) ;
#26773 = ORIENTED_EDGE ( 'NONE', *, *, #9800, .F. ) ;
#26774 = CARTESIAN_POINT ( 'NONE',  ( 420.0000000000002274, 34.64101615137744972, 14.00000000000000178 ) ) ;
#26775 = CARTESIAN_POINT ( 'NONE',  ( 13.93479307118181509, 9.207276677253689812, -14.11477394318545286 ) ) ;
#26776 = DIRECTION ( 'NONE',  ( -0.5877852522924731371, -1.586114251531760235E-16, 0.8090169943749474513 ) ) ;
#26777 = FACE_OUTER_BOUND ( 'NONE', #11778, .T. ) ;
#26778 = ADVANCED_FACE ( 'NONE', ( #11132 ), #13717, .T. ) ;
#26779 = VECTOR ( 'NONE', #22378, 1000.000000000000000 ) ;
#26780 = CARTESIAN_POINT ( 'NONE',  ( 24.70156281743647142, 0.04986695427254615731, -17.03102378627558977 ) ) ;
#26781 = CARTESIAN_POINT ( 'NONE',  ( 22.70908579165946506, -0.2254420654732764706, -12.61778515557981528 ) ) ;
#26782 = EDGE_LOOP ( 'NONE', ( #23819, #18399, #17421, #25936 ) ) ;
#26783 = PLANE ( 'NONE',  #6923 ) ;
#26784 = ADVANCED_FACE ( 'NONE', ( #22589 ), #10824, .T. ) ;
#26785 = CARTESIAN_POINT ( 'NONE',  ( 136.1922820468854241, -1.999999999999980016, -28.06379628232387446 ) ) ;
#26786 = ADVANCED_FACE ( 'NONE', ( #27050 ), #24790, .T. ) ;
#26787 = EDGE_CURVE ( 'NONE', #1603, #16074, #8682, .T. ) ;
#26788 = CARTESIAN_POINT ( 'NONE',  ( 174.5152310637604387, -9.999999999999994671, -11.28819510263909542 ) ) ;
#26789 = EDGE_CURVE ( 'NONE', #23064, #2741, #15516, .T. ) ;
#26790 = LINE ( 'NONE', #829, #1826 ) ;
#26791 = AXIS2_PLACEMENT_3D ( 'NONE', #26632, #22034, #5712 ) ;
#26792 = DIRECTION ( 'NONE',  ( 0.3090169943749472292, 8.338696094057992503E-17, -0.9510565162951536422 ) ) ;
#26793 = CARTESIAN_POINT ( 'NONE',  ( 158.6922820468854241, -4.999999999999974243, -32.39392330124607611 ) ) ;
#26794 = CARTESIAN_POINT ( 'NONE',  ( 10.82443827553465177, 12.24310121783546634, -16.12906421532448675 ) ) ;
#26795 = AXIS2_PLACEMENT_3D ( 'NONE', #3568, #13865, #13016 ) ;
#26796 = CARTESIAN_POINT ( 'NONE',  ( 15.44629794785920218, 3.545610805586186132, -16.71614555938632307 ) ) ;
#26797 = CARTESIAN_POINT ( 'NONE',  ( 24.19195398915606532, -10.47609993289601427, -15.85356615136800151 ) ) ;
#26798 = VERTEX_POINT ( 'NONE', #4272 ) ;
#26799 = DIRECTION ( 'NONE',  ( 1.000000000000000000, 0.000000000000000000, 0.000000000000000000 ) ) ;
#26800 = PLANE ( 'NONE',  #15026 ) ;
#26801 = DIRECTION ( 'NONE',  ( 0.000000000000000000, 0.000000000000000000, 1.000000000000000000 ) ) ;
#26802 = DIRECTION ( 'NONE',  ( -2.698458740408365879E-16, 1.000000000000000000, 0.000000000000000000 ) ) ;
#26803 = DIRECTION ( 'NONE',  ( 1.000000000000000000, 2.168404344971006896E-16, 0.000000000000000000 ) ) ;
#26804 = CARTESIAN_POINT ( 'NONE',  ( 131.1922820468854241, -1.999999999999981792, -19.40354224447947118 ) ) ;
#26806 = ORIENTED_EDGE ( 'NONE', *, *, #22532, .T. ) ;
#26805 = CARTESIAN_POINT ( 'NONE',  ( 15.70491959545049987, 3.570626008024105680, -15.63470537622339229 ) ) ;
#26807 = ORIENTED_EDGE ( 'NONE', *, *, #783, .F. ) ;
#26808 = CARTESIAN_POINT ( 'NONE',  ( 4.175000000000003375, 1.854072451124011344E-15, -0.5776712190230064436 ) ) ;
#26809 = CARTESIAN_POINT ( 'NONE',  ( 12.27631119714397201, 9.497383584800669354, -15.31093738554958428 ) ) ;
#26810 = DIRECTION ( 'NONE',  ( -1.000000000000000000, -4.440892098500622217E-16, 0.000000000000000000 ) ) ;
#26811 = DIRECTION ( 'NONE',  ( 0.9510565162951535312, 2.566386769018988816E-16, -0.3090169943749475623 ) ) ;
#26812 = CARTESIAN_POINT ( 'NONE',  ( 19.40121574091639189, 1.432572567346982240, -13.43353846741550406 ) ) ;
#26813 = DIRECTION ( 'NONE',  ( 2.908569913943825554E-16, -1.000000000000000000, -0.000000000000000000 ) ) ;
#26814 = CARTESIAN_POINT ( 'NONE',  ( 22.56790106455553868, 4.272635385308135803, -18.10442882813315535 ) ) ;
#26815 = EDGE_LOOP ( 'NONE', ( #10307, #3356, #17688, #16625, #26124 ) ) ;
#26816 = LINE ( 'NONE', #6034, #12018 ) ;
#26817 = FILL_AREA_STYLE_COLOUR ( '', #6385 ) ;
#26818 = VECTOR ( 'NONE', #22578, 1000.000000000000114 ) ;
#26819 = CARTESIAN_POINT ( 'NONE',  ( 24.92984004655564334, -8.306894832562658593, -19.61321747044761921 ) ) ;
#26820 = CARTESIAN_POINT ( 'NONE',  ( 24.74990718239607546, -5.907774739380937667, -20.30682099139976060 ) ) ;
#26821 = AXIS2_PLACEMENT_3D ( 'NONE', #28874, #1064, #17514 ) ;
#26822 = CARTESIAN_POINT ( 'NONE',  ( 25.90632082398269276, -12.28056132945115841, -15.12647891527467969 ) ) ;
#26823 = ADVANCED_FACE ( 'NONE', ( #6105 ), #20281, .T. ) ;
#26824 = EDGE_CURVE ( 'NONE', #28903, #22806, #28227, .T. ) ;
#26825 = ORIENTED_EDGE ( 'NONE', *, *, #8936, .T. ) ;
#26826 = EDGE_CURVE ( 'NONE', #20048, #10103, #22442, .T. ) ;
#26827 = CARTESIAN_POINT ( 'NONE',  ( 167.0152310637604387, -9.999999999999998224, 1.702185954127501066 ) ) ;
#26829 = ORIENTED_EDGE ( 'NONE', *, *, #17211, .T. ) ;
#26828 = EDGE_CURVE ( 'NONE', #13148, #15024, #3831, .T. ) ;
#26830 = DIRECTION ( 'NONE',  ( -1.840388255087189623E-16, -1.000000000000000000, 0.000000000000000000 ) ) ;
#26831 = CARTESIAN_POINT ( 'NONE',  ( 158.6922820468853956, -1.999999999999973577, -26.58683881228715862 ) ) ;
#26832 = CARTESIAN_POINT ( 'NONE',  ( 107.1134392459000395, -4.999999999999988454, -77.82246893306485447 ) ) ;
#26833 = CARTESIAN_POINT ( 'NONE',  ( 8.000000000000014211, -3.867591403079187806, -0.4976753153245951355 ) ) ;
#26834 = CARTESIAN_POINT ( 'NONE',  ( 25.61676826379006400, -5.274948970184475172, -14.00514367894158418 ) ) ;
#26835 = DIRECTION ( 'NONE',  ( -0.5877852522924731371, -1.586114251531760235E-16, 0.8090169943749474513 ) ) ;
#26836 = CARTESIAN_POINT ( 'NONE',  ( 33.25614251967556356, -10.36847857886694868, -17.86465469861353483 ) ) ;
#26838 = CARTESIAN_POINT ( 'NONE',  ( 129.5152310637605524, -10.00000000000000888, -21.71180489736090991 ) ) ;
#26837 = VECTOR ( 'NONE', #14142, 1000.000000000000000 ) ;
#26839 = CARTESIAN_POINT ( 'NONE',  ( 9.695397291186985456, 17.42102709130404747, -17.08803885907851594 ) ) ;
#26840 = FACE_OUTER_BOUND ( 'NONE', #404, .T. ) ;
#26841 = CARTESIAN_POINT ( 'NONE',  ( 157.0152310637604387, -4.999999999999975131, -0.06116980274991495881 ) ) ;
#26843 = CARTESIAN_POINT ( 'NONE',  ( 9.661883061612440926, 16.25482663361732705, -17.93331994345748726 ) ) ;
#26842 = VECTOR ( 'NONE', #1555, 1000.000000000000000 ) ;
#26844 = DIRECTION ( 'NONE',  ( 0.3090169943749475623, 8.338696094058001131E-17, 0.9510565162951536422 ) ) ;
#26845 = COLOUR_RGB ( '', 0.31764706, 0.68627451, 0.89019608) ;
#26846 = CARTESIAN_POINT ( 'NONE',  ( 158.6922820468853388, -1.999999999999974465, -9.266330736598359152 ) ) ;
#26847 = ORIENTED_EDGE ( 'NONE', *, *, #26320, .T. ) ;
#26848 = LINE ( 'NONE', #3624, #23691 ) ;
#26849 = DIRECTION ( 'NONE',  ( 0.000000000000000000, 1.000000000000000000, 1.224646799147353207E-16 ) ) ;
#26850 = CARTESIAN_POINT ( 'NONE',  ( 167.0152310637605240, -1.999999999999970912, -24.27857615940569502 ) ) ;
#26851 = VERTEX_POINT ( 'NONE', #8835 ) ;
#26852 = ORIENTED_EDGE ( 'NONE', *, *, #11440, .T. ) ;
#26853 = ORIENTED_EDGE ( 'NONE', *, *, #5049, .T. ) ;
#26854 = CARTESIAN_POINT ( 'NONE',  ( 8.944585005148796952, 16.95159128516397118, -17.91410349795882340 ) ) ;
#26855 = AXIS2_PLACEMENT_3D ( 'NONE', #22045, #28815, #19591 ) ;
#26856 = EDGE_CURVE ( 'NONE', #379, #29186, #6417, .T. ) ;
#26857 = CARTESIAN_POINT ( 'NONE',  ( 13.46306793452363770, 5.846312397186087750, -15.11995136480861746 ) ) ;
#26858 = VECTOR ( 'NONE', #26961, 1000.000000000000000 ) ;
#26859 = CARTESIAN_POINT ( 'NONE',  ( 28.50411217586706769, -6.135108760518566129, -18.55796808427148648 ) ) ;
#26860 = DIRECTION ( 'NONE',  ( 0.5877852522924731371, 1.586114251531760728E-16, -0.8090169943749474513 ) ) ;
#26861 = DIRECTION ( 'NONE',  ( 1.000000000000000000, 2.698458740408365879E-16, -1.110223024625156540E-16 ) ) ;
#26862 = LINE ( 'NONE', #12628, #27472 ) ;
#26863 = VECTOR ( 'NONE', #25152, 1000.000000000000000 ) ;
#26864 = VECTOR ( 'NONE', #30045, 1000.000000000000000 ) ;
#26865 = VERTEX_POINT ( 'NONE', #1690 ) ;
#26866 = EDGE_CURVE ( 'NONE', #2849, #5527, #27508, .T. ) ;
#26867 = CARTESIAN_POINT ( 'NONE',  ( 171.1922820468852819, -1.999999999999971356, -4.936203717676158398 ) ) ;
#26868 = EDGE_CURVE ( 'NONE', #28371, #28447, #19050, .T. ) ;
#26869 = DIRECTION ( 'NONE',  ( -0.5877852522924731371, -1.586114251531760235E-16, 0.8090169943749474513 ) ) ;
#26870 = CYLINDRICAL_SURFACE ( 'NONE', #1512, 5.000000000000000000 ) ;
#26871 = DIRECTION ( 'NONE',  ( -0.5877852522924731371, -1.586114251531760728E-16, -0.8090169943749474513 ) ) ;
#26872 = VECTOR ( 'NONE', #16898, 999.9999999999998863 ) ;
#26873 = CARTESIAN_POINT ( 'NONE',  ( 12.56022695423237145, 8.580358410770909217, -16.34122335808152826 ) ) ;
#26874 = CARTESIAN_POINT ( 'NONE',  ( 35.24964364652129234, -20.84149066036063047, -20.16262864730545346 ) ) ;
#26875 = VERTEX_POINT ( 'NONE', #6868 ) ;
#26876 = AXIS2_PLACEMENT_3D ( 'NONE', #6064, #1048, #10632 ) ;
#26877 = CARTESIAN_POINT ( 'NONE',  ( 9.109039160554445402, 16.19738356544468516, -17.05632368146133615 ) ) ;
#26878 = ORIENTED_EDGE ( 'NONE', *, *, #8792, .T. ) ;
#26879 = CARTESIAN_POINT ( 'NONE',  ( 23.84106988684860440, -4.080291168153947545, -13.50610408985603250 ) ) ;
#26880 = CARTESIAN_POINT ( 'NONE',  ( 10.35864918915110877, 16.97212501191939538, -17.98596209335946128 ) ) ;
#26881 = FACE_BOUND ( 'NONE', #23363, .T. ) ;
#26882 = COLOUR_RGB ( '', 0.66274510, 0.83137255, 0.94901961) ;
#26883 = VERTEX_POINT ( 'NONE', #25778 ) ;
#26884 = LINE ( 'NONE', #20269, #12591 ) ;
#26885 = ORIENTED_EDGE ( 'NONE', *, *, #22323, .F. ) ;
#26886 = CARTESIAN_POINT ( 'NONE',  ( 11.44040408106239326, 9.418203516307107392, -15.87434068686103394 ) ) ;
#26887 = CARTESIAN_POINT ( 'NONE',  ( 164.5152310637604955, -9.999999999999998224, -19.94844914048349693 ) ) ;
#26888 = ORIENTED_EDGE ( 'NONE', *, *, #9404, .T. ) ;
#26889 = LINE ( 'NONE', #10210, #15450 ) ;
#26890 = ORIENTED_EDGE ( 'NONE', *, *, #17404, .T. ) ;
#26891 = CARTESIAN_POINT ( 'NONE',  ( 9.661883061612440926, 16.25482663361732705, -17.91796598306941135 ) ) ;
#26892 = EDGE_CURVE ( 'NONE', #29151, #19118, #444, .T. ) ;
#26893 = ORIENTED_EDGE ( 'NONE', *, *, #485, .F. ) ;
#26894 = CARTESIAN_POINT ( 'NONE',  ( 19.90219557808113038, 2.290409793443704878, -20.93543687874882053 ) ) ;
#26895 = CARTESIAN_POINT ( 'NONE',  ( 16.51977620067554042, 7.986930271725532826, -13.83285890266734519 ) ) ;
#26896 = ORIENTED_EDGE ( 'NONE', *, *, #17209, .F. ) ;
#26897 = VERTEX_POINT ( 'NONE', #4856 ) ;
#26898 = PRODUCT_DEFINITION ( 'UNKNOWN', '', #10719, #17704 ) ;
#26899 = LINE ( 'NONE', #24129, #1866 ) ;
#26900 = VERTEX_POINT ( 'NONE', #13856 ) ;
#26901 = LINE ( 'NONE', #12508, #2568 ) ;
#26902 = VECTOR ( 'NONE', #9383, 1000.000000000000000 ) ;
#26903 = CARTESIAN_POINT ( 'NONE',  ( 15.54217852991911997, 3.796156774867226247, -18.16774540469225485 ) ) ;
#26904 = FACE_OUTER_BOUND ( 'NONE', #6968, .T. ) ;
#26905 = CARTESIAN_POINT ( 'NONE',  ( 1.214306433183764966E-14, 4.618802153517016507, -0.3572655899081716435 ) ) ;
#26906 = ORIENTED_EDGE ( 'NONE', *, *, #9341, .F. ) ;
#26907 = CARTESIAN_POINT ( 'NONE',  ( 159.7287565553228603, -4.999999999999974243, 0.8205080756887861426 ) ) ;
#26908 = CARTESIAN_POINT ( 'NONE',  ( 32.00110207675911767, -10.95298233446834502, -16.54939777171900417 ) ) ;
#26909 = DIRECTION ( 'NONE',  ( 0.000000000000000000, 0.000000000000000000, -1.000000000000000000 ) ) ;
#26910 = DIRECTION ( 'NONE',  ( 0.5877852522924731371, 1.586114251531760728E-16, -0.8090169943749474513 ) ) ;
#26911 = CARTESIAN_POINT ( 'NONE',  ( 12.24518234991790955, 9.516123393600787850, -15.33326918312795328 ) ) ;
#26912 = ORIENTED_EDGE ( 'NONE', *, *, #7405, .T. ) ;
#26913 = CARTESIAN_POINT ( 'NONE',  ( 4.000000000000008882, -6.928203230275510549, -5.000000000000000888 ) ) ;
#26914 = ORIENTED_EDGE ( 'NONE', *, *, #19998, .T. ) ;
#26915 = CIRCLE ( 'NONE', #24386, 4.000000000000000000 ) ;
#26916 = DIRECTION ( 'NONE',  ( -0.5877852522924731371, 0.000000000000000000, 0.8090169943749474513 ) ) ;
#26917 = ORIENTED_EDGE ( 'NONE', *, *, #27131, .F. ) ;
#26918 = CARTESIAN_POINT ( 'NONE',  ( 12.33231149932895221, 7.515762311178675326, -15.25793818847554562 ) ) ;
#26919 = DIRECTION ( 'NONE',  ( -0.8090169943749474513, -2.183098979609982436E-16, -0.5877852522924731371 ) ) ;
#26920 = CYLINDRICAL_SURFACE ( 'NONE', #1838, 5.000000000000000888 ) ;
#26921 = VERTEX_POINT ( 'NONE', #16763 ) ;
#26922 = ORIENTED_EDGE ( 'NONE', *, *, #12759, .T. ) ;
#26923 = LINE ( 'NONE', #20016, #1315 ) ;
#26924 = ORIENTED_EDGE ( 'NONE', *, *, #17959, .F. ) ;
#26925 = CARTESIAN_POINT ( 'NONE',  ( 12.83220575256047802, 9.540835953717470730, -16.14105854569320542 ) ) ;
#26926 = EDGE_CURVE ( 'NONE', #8342, #20109, #5165, .T. ) ;
#26927 = EDGE_CURVE ( 'NONE', #8651, #11101, #18452, .T. ) ;
#26928 = CARTESIAN_POINT ( 'NONE',  ( 35.28777801271252912, -15.52033788203570985, -19.16652784865743442 ) ) ;
#26929 = CARTESIAN_POINT ( 'NONE',  ( 20.14386580841007657, 1.771853782379294140, -13.30505882909219295 ) ) ;
#26930 = EDGE_LOOP ( 'NONE', ( #17836, #29336, #13561, #27909 ) ) ;
#26932 = EDGE_CURVE ( 'NONE', #13701, #7028, #14302, .T. ) ;
#26931 = PRODUCT_DEFINITION_SHAPE ( 'NONE', 'NONE',  #580 ) ;
#26933 = VERTEX_POINT ( 'NONE', #25474 ) ;
#26934 = DIRECTION ( 'NONE',  ( -2.698458740408365879E-16, 1.000000000000000000, 0.000000000000000000 ) ) ;
#26935 = EDGE_CURVE ( 'NONE', #7167, #27514, #20879, .T. ) ;
#26936 = CARTESIAN_POINT ( 'NONE',  ( 17.25677449038176547, 8.733363079223632752, -20.54546673180767158 ) ) ;
#26937 = DIRECTION ( 'NONE',  ( -2.698458740408365879E-16, 1.000000000000000000, 0.000000000000000000 ) ) ;
#26938 = CARTESIAN_POINT ( 'NONE',  ( 137.2287565553230309, -10.00000000000000533, -29.49038105676660138 ) ) ;
#26939 = ORIENTED_EDGE ( 'NONE', *, *, #3644, .T. ) ;
#26940 = CARTESIAN_POINT ( 'NONE',  ( 22.42023978564754927, -3.655767601918122445, -13.54521809681785172 ) ) ;
#26941 = CARTESIAN_POINT ( 'NONE',  ( 16.80134558234102471, 1.491865220098682387, -17.16076555717535257 ) ) ;
#26942 = CIRCLE ( 'NONE', #22068, 2.055000000000000160 ) ;
#26943 = ORIENTED_EDGE ( 'NONE', *, *, #1109, .T. ) ;
#26944 = VERTEX_POINT ( 'NONE', #12019 ) ;
#26945 = DIRECTION ( 'NONE',  ( 0.9510565162951536422, 0.000000000000000000, -0.3090169943749475623 ) ) ;
#26946 = FACE_OUTER_BOUND ( 'NONE', #662, .T. ) ;
#26947 = CARTESIAN_POINT ( 'NONE',  ( 156.1922820468853388, -10.00000000000000178, -2.083034168790677043 ) ) ;
#26948 = DIRECTION ( 'NONE',  ( 1.000000000000000000, 2.698458740408365879E-16, -1.110223024625156540E-16 ) ) ;
#26949 = PLANE ( 'NONE',  #6309 ) ;
#26950 = VECTOR ( 'NONE', #16205, 1000.000000000000000 ) ;
#26951 = CARTESIAN_POINT ( 'NONE',  ( 0.000000000000000000, 0.000000000000000000, -4.974599999999998801 ) ) ;
#26952 = CARTESIAN_POINT ( 'NONE',  ( 11.22348983819090407, 9.093098897663914215, -17.24177177356946800 ) ) ;
#26953 = CARTESIAN_POINT ( 'NONE',  ( 12.50481220565295004, 8.572828783776230921, -15.12633959982445653 ) ) ;
#26954 = CARTESIAN_POINT ( 'NONE',  ( 26.02348467347448491, -3.622150272347476108, -19.21400332953221124 ) ) ;
#26955 = ORIENTED_EDGE ( 'NONE', *, *, #2938, .F. ) ;
#26956 = DIRECTION ( 'NONE',  ( -0.9510565162951536422, -2.566386769018988323E-16, 0.3090169943749475623 ) ) ;
#26957 = FACE_OUTER_BOUND ( 'NONE', #12196, .T. ) ;
#26958 = ORIENTED_EDGE ( 'NONE', *, *, #18976, .T. ) ;
#26959 = CARTESIAN_POINT ( 'NONE',  ( -4.000000000000020428, -6.928203230275511437, -5.000000000000000888 ) ) ;
#26960 = AXIS2_PLACEMENT_3D ( 'NONE', #6526, #23008, #17952 ) ;
#26961 = DIRECTION ( 'NONE',  ( -1.110223024625156540E-16, 0.000000000000000000, -1.000000000000000000 ) ) ;
#26962 = DIRECTION ( 'NONE',  ( 0.5877852522924731371, 1.586114251531760728E-16, 0.8090169943749474513 ) ) ;
#26963 = CARTESIAN_POINT ( 'NONE',  ( 25.23810427664335165, -6.496417100615061280, -13.69959235629456629 ) ) ;
#26964 = ORIENTED_EDGE ( 'NONE', *, *, #18035, .F. ) ;
#26965 = DIRECTION ( 'NONE',  ( -1.000000000000000000, 0.000000000000000000, 0.000000000000000000 ) ) ;
#26966 = CARTESIAN_POINT ( 'NONE',  ( 11.36920530384750805, 13.65748684056475426, -15.68605758175906040 ) ) ;
#26967 = ADVANCED_FACE ( 'NONE', ( #144 ), #29794, .T. ) ;
#26968 = CARTESIAN_POINT ( 'NONE',  ( 32.58918748260075660, -11.04229556371213583, -18.21152344180378080 ) ) ;
#26969 = CARTESIAN_POINT ( 'NONE',  ( 0.000000000000000000, 0.000000000000000000, 4.999999999999998224 ) ) ;
#26970 = EDGE_CURVE ( 'NONE', #14514, #24876, #28095, .T. ) ;
#26971 = EDGE_CURVE ( 'NONE', #11270, #22429, #2735, .T. ) ;
#26972 = CARTESIAN_POINT ( 'NONE',  ( 26.84970692451943819, -5.812874930055231815, -14.04107299160273037 ) ) ;
#26973 = LINE ( 'NONE', #6031, #25707 ) ;
#26974 = EDGE_CURVE ( 'NONE', #6553, #22761, #9728, .T. ) ;
#26975 = CARTESIAN_POINT ( 'NONE',  ( 16.44673144568935541, 3.517958023484313301, -20.47440421422559353 ) ) ;
#26976 = VERTEX_POINT ( 'NONE', #21336 ) ;
#26977 = DIRECTION ( 'NONE',  ( -0.9510565162951536422, -2.566386769018988816E-16, -0.3090169943749472292 ) ) ;
#26978 = CARTESIAN_POINT ( 'NONE',  ( 27.97271982581976957, -5.335442005784750918, -18.83880583778296725 ) ) ;
#26979 = VECTOR ( 'NONE', #4575, 1000.000000000000000 ) ;
#26980 = CARTESIAN_POINT ( 'NONE',  ( 24.47917272657372223, 1.093256025350008542, -14.89707007128618699 ) ) ;
#26981 = CARTESIAN_POINT ( 'NONE',  ( 25.24878800877705487, -9.370948223588685622, -14.18615728435988288 ) ) ;
#26982 = AXIS2_PLACEMENT_3D ( 'NONE', #18421, #16428, #16271 ) ;
#26983 = DIRECTION ( 'NONE',  ( -2.698458740408365879E-16, 1.000000000000000000, 0.000000000000000000 ) ) ;
#26984 = ORIENTED_EDGE ( 'NONE', *, *, #12170, .T. ) ;
#26985 = CARTESIAN_POINT ( 'NONE',  ( 5.272361329723610268, -5.000000000000015987, 16.22665966652977332 ) ) ;
#26986 = FACE_OUTER_BOUND ( 'NONE', #9459, .T. ) ;
#26987 = CARTESIAN_POINT ( 'NONE',  ( 175.7287565553229456, -4.999999999999970690, -2.233642730705313717 ) ) ;
#26988 = CARTESIAN_POINT ( 'NONE',  ( 177.2287565553228319, -9.999999999999994671, -3.509618943233403510 ) ) ;
#26989 = CARTESIAN_POINT ( 'NONE',  ( 25.59007283008577005, -3.201708215360036913, -15.56755918271449168 ) ) ;
#26990 = CARTESIAN_POINT ( 'NONE',  ( 18.35279563442798079, 9.979516425631709708, -19.26739628155305439 ) ) ;
#26991 = EDGE_CURVE ( 'NONE', #26068, #23525, #15003, .T. ) ;
#26992 = CARTESIAN_POINT ( 'NONE',  ( 32.68023997084922883, -9.631188006280016367, -18.23865791264771730 ) ) ;
#26993 = CARTESIAN_POINT ( 'NONE',  ( 130.7287565553229456, -9.999999999999982236, 3.500000000000003109 ) ) ;
#26994 = CARTESIAN_POINT ( 'NONE',  ( 9.675370519060759733, 17.51287242109451014, -17.23928541814325399 ) ) ;
#26995 = DIRECTION ( 'NONE',  ( -2.698458740408365879E-16, 1.000000000000000000, 0.000000000000000000 ) ) ;
#26996 = CARTESIAN_POINT ( 'NONE',  ( 13.77718166750865869, 8.859676595473324312, -15.39100258941132182 ) ) ;
#26997 = CARTESIAN_POINT ( 'NONE',  ( 9.661883073086391605, 16.25482658099627642, -17.91571305590050400 ) ) ;
#26998 = CARTESIAN_POINT ( 'NONE',  ( 4.000000000000000000, 1.776356839400248887E-15, 1.699999999999996625 ) ) ;
#26999 = DIRECTION ( 'NONE',  ( 1.000000000000000000, 4.440892098500622217E-16, 0.000000000000000000 ) ) ;
#27000 = CARTESIAN_POINT ( 'NONE',  ( 11.21346931060482000, 10.45895530107994098, -15.96818619734747458 ) ) ;
#27001 = ORIENTED_EDGE ( 'NONE', *, *, #5158, .F. ) ;
#27002 = CARTESIAN_POINT ( 'NONE',  ( 174.7287565553228887, -9.999999999999994671, -16.50000000000000355 ) ) ;
#27003 = CARTESIAN_POINT ( 'NONE',  ( 427.0000000000002274, 34.64101615137744972, 12.00000000000000178 ) ) ;
#27004 = ADVANCED_FACE ( 'NONE', ( #14456 ), #9273, .T. ) ;
#27005 = EDGE_CURVE ( 'NONE', #3964, #9294, #27952, .T. ) ;
#27006 = DIRECTION ( 'NONE',  ( 1.000000000000000000, 4.440892098500622217E-16, 0.000000000000000000 ) ) ;
#27007 = VECTOR ( 'NONE', #25868, 1000.000000000000000 ) ;
#27008 = ORIENTED_EDGE ( 'NONE', *, *, #8413, .F. ) ;
#27009 = EDGE_CURVE ( 'NONE', #15637, #15011, #11868, .T. ) ;
#27010 = ORIENTED_EDGE ( 'NONE', *, *, #2111, .F. ) ;
#27011 = EDGE_CURVE ( 'NONE', #2723, #12166, #16299, .T. ) ;
#27012 = CARTESIAN_POINT ( 'NONE',  ( 8.944584683310379702, 16.95159276115599667, -17.92279151347708677 ) ) ;
#27013 = CARTESIAN_POINT ( 'NONE',  ( 31.86596522828317291, -10.28264332119880820, -18.16914504201997360 ) ) ;
#27014 = ORIENTED_EDGE ( 'NONE', *, *, #28327, .F. ) ;
#27015 = CARTESIAN_POINT ( 'NONE',  ( 30.36731020202829612, -7.149780978071095028, -17.08985122409953306 ) ) ;
#27016 = CARTESIAN_POINT ( 'NONE',  ( 24.79209089726652948, -9.725099617967893906, -18.44766554224525734 ) ) ;
#27017 = CARTESIAN_POINT ( 'NONE',  ( 111.1215651223918144, -4.999999999999986677, -80.73454283993487479 ) ) ;
#27018 = DIRECTION ( 'NONE',  ( 0.5877852522924731371, 0.000000000000000000, 0.8090169943749474513 ) ) ;
#27019 = CARTESIAN_POINT ( 'NONE',  ( 0.000000000000000000, 0.000000000000000000, -2.424599999999998978 ) ) ;
#27020 = VECTOR ( 'NONE', #22144, 1000.000000000000000 ) ;
#27021 = EDGE_LOOP ( 'NONE', ( #18128, #12693, #10051, #20689, #11342 ) ) ;
#27022 = PLANE ( 'NONE',  #17675 ) ;
#27023 = CARTESIAN_POINT ( 'NONE',  ( 167.0152310637604955, -9.999999999999996447, -26.04193191628311155 ) ) ;
#27024 =( NAMED_UNIT ( * ) PLANE_ANGLE_UNIT ( ) SI_UNIT ( $, .RADIAN. ) );
#27025 = DIRECTION ( 'NONE',  ( 0.9510565162951536422, 0.000000000000000000, -0.3090169943749475623 ) ) ;
#27026 = VECTOR ( 'NONE', #9359, 1000.000000000000000 ) ;
#27027 = CARTESIAN_POINT ( 'NONE',  ( 13.14084490070201738, 8.578467993704791184, -15.89817422466314945 ) ) ;
#27028 = CARTESIAN_POINT ( 'NONE',  ( 33.57416420788476330, -12.34692739235205217, -18.69991813917680190 ) ) ;
#27029 = ORIENTED_EDGE ( 'NONE', *, *, #23052, .F. ) ;
#27030 = CARTESIAN_POINT ( 'NONE',  ( 9.371932165391852365, 14.99172273419688750, -16.94745289082924344 ) ) ;
#27031 = ORIENTED_EDGE ( 'NONE', *, *, #14574, .T. ) ;
#27032 = CARTESIAN_POINT ( 'NONE',  ( 26.36224721256908410, -8.875037662531589433, -13.49479840426202948 ) ) ;
#27033 = CARTESIAN_POINT ( 'NONE',  ( 12.88201729092779857, 9.522117202545773651, -16.10446439827067167 ) ) ;
#27034 = FACE_BOUND ( 'NONE', #5803, .T. ) ;
#27035 = VECTOR ( 'NONE', #13703, 1000.000000000000000 ) ;
#27036 = EDGE_LOOP ( 'NONE', ( #21463, #5000, #4793, #19250, #25480 ) ) ;
#27037 = CARTESIAN_POINT ( 'NONE',  ( 149.5152310637606092, -1.999999999999975353, -28.60870317832789667 ) ) ;
#27038 = EDGE_CURVE ( 'NONE', #14791, #5616, #7160, .T. ) ;
#27039 = CARTESIAN_POINT ( 'NONE',  ( 12.44984726620633353, 8.550925603015029353, -15.16996558791898231 ) ) ;
#27040 = DIRECTION ( 'NONE',  ( 0.3090169943749472292, 8.338696094057992503E-17, -0.9510565162951536422 ) ) ;
#27041 = ORIENTED_EDGE ( 'NONE', *, *, #14749, .T. ) ;
#27042 = EDGE_CURVE ( 'NONE', #4884, #17347, #9576, .T. ) ;
#27043 = CARTESIAN_POINT ( 'NONE',  ( -7.999999999999998224, -3.098204225878192997, -0.3157906771918777000 ) ) ;
#27044 = ORIENTED_EDGE ( 'NONE', *, *, #25176, .T. ) ;
#27045 = EDGE_CURVE ( 'NONE', #5490, #18869, #906, .T. ) ;
#27046 = CARTESIAN_POINT ( 'NONE',  ( 13.12468173219994760, 8.571325198882655982, -15.91105655537220009 ) ) ;
#27047 = VERTEX_POINT ( 'NONE', #22095 ) ;
#27048 = CARTESIAN_POINT ( 'NONE',  ( 13.25083620024415332, 6.663885870737293438, -17.30077526834593016 ) ) ;
#27049 = CARTESIAN_POINT ( 'NONE',  ( 16.89391627328321732, 8.154734282165337689, -13.86877251323280014 ) ) ;
#27050 = FACE_OUTER_BOUND ( 'NONE', #21332, .T. ) ;
#27051 = AXIS2_PLACEMENT_3D ( 'NONE', #1736, #20325, #29714 ) ;
#27052 = ORIENTED_EDGE ( 'NONE', *, *, #26892, .F. ) ;
#27053 = DIRECTION ( 'NONE',  ( -2.698458740408365879E-16, 1.000000000000000000, 0.000000000000000000 ) ) ;
#27054 = CARTESIAN_POINT ( 'NONE',  ( 25.36810815240369621, -0.9165050883202133791, -18.11329069065276443 ) ) ;
#27055 = FACE_OUTER_BOUND ( 'NONE', #26429, .T. ) ;
#27056 = CARTESIAN_POINT ( 'NONE',  ( 167.0152310637604955, -9.999999999999996447, -15.61832212156129707 ) ) ;
#27057 = ORIENTED_EDGE ( 'NONE', *, *, #16658, .F. ) ;
#27058 = EDGE_CURVE ( 'NONE', #23159, #1963, #26700, .T. ) ;
#27059 = DIRECTION ( 'NONE',  ( -2.698458740408365879E-16, 1.000000000000000000, 0.000000000000000000 ) ) ;
#27060 = CARTESIAN_POINT ( 'NONE',  ( 33.29928106196997817, -12.14339677642331772, -19.64090527578606427 ) ) ;
#27061 = PLANE ( 'NONE',  #9207 ) ;
#27062 = ORIENTED_EDGE ( 'NONE', *, *, #26856, .F. ) ;
#27063 = ORIENTED_EDGE ( 'NONE', *, *, #21856, .T. ) ;
#27064 = PLANE ( 'NONE',  #29574 ) ;
#27065 = VECTOR ( 'NONE', #13975, 1000.000000000000000 ) ;
#27066 = CARTESIAN_POINT ( 'NONE',  ( 12.27916258238306746, 9.531139938431367753, -15.30618633255685879 ) ) ;
#27067 = CARTESIAN_POINT ( 'NONE',  ( 35.28941737075538043, -22.02017293461823755, -20.69856730472309891 ) ) ;
#27068 = DIRECTION ( 'NONE',  ( 2.908569913943826047E-16, -1.000000000000000000, 6.826925868028107924E-18 ) ) ;
#27069 = ORIENTED_EDGE ( 'NONE', *, *, #3608, .F. ) ;
#27070 = LINE ( 'NONE', #24757, #2967 ) ;
#27071 = VERTEX_POINT ( 'NONE', #24093 ) ;
#27072 = CARTESIAN_POINT ( 'NONE',  ( 10.64844024921564092, 9.137493944846720950, -16.41957189434499753 ) ) ;
#27073 = FACE_OUTER_BOUND ( 'NONE', #6422, .T. ) ;
#27074 = FACE_OUTER_BOUND ( 'NONE', #19678, .T. ) ;
#27075 = EDGE_CURVE ( 'NONE', #27415, #25465, #16907, .T. ) ;
#27076 = DIRECTION ( 'NONE',  ( 0.5877852522924731371, 1.586114251531760728E-16, -0.8090169943749474513 ) ) ;
#27077 = ORIENTED_EDGE ( 'NONE', *, *, #11949, .F. ) ;
#27078 = CARTESIAN_POINT ( 'NONE',  ( 12.86924247997729687, 9.516471784987144744, -16.11464614809275631 ) ) ;
#27079 = CARTESIAN_POINT ( 'NONE',  ( 34.34130860390597206, -11.59244310827663149, -18.69197402374579653 ) ) ;
#27080 = CARTESIAN_POINT ( 'NONE',  ( 19.71807001554888217, -1.708786246101231532, -19.21472004699903380 ) ) ;
#27081 = VERTEX_POINT ( 'NONE', #17354 ) ;
#27082 = CARTESIAN_POINT ( 'NONE',  ( 0.000000000000000000, 0.000000000000000000, -5.000000000000000888 ) ) ;
#27083 = CARTESIAN_POINT ( 'NONE',  ( -4.000000000000005329, 2.309401076758490934, -0.3572655899081616515 ) ) ;
#27084 = PLANE ( 'NONE',  #3274 ) ;
#27085 =( NAMED_UNIT ( * ) SI_UNIT ( $, .STERADIAN. ) SOLID_ANGLE_UNIT ( ) );
#27086 = CARTESIAN_POINT ( 'NONE',  ( 30.76698452600511402, -8.440788201038053273, -16.67119366161266925 ) ) ;
#27087 = CARTESIAN_POINT ( 'NONE',  ( 20.64663396976543552, 5.620433075351431995, -17.27584747705915902 ) ) ;
#27088 = VECTOR ( 'NONE', #11024, 1000.000000000000000 ) ;
#27089 = EDGE_LOOP ( 'NONE', ( #23408, #18442, #13340, #15844, #18778 ) ) ;
#27090 = VERTEX_POINT ( 'NONE', #21795 ) ;
#27091 = LINE ( 'NONE', #8574, #23026 ) ;
#27092 = CARTESIAN_POINT ( 'NONE',  ( -6.499999999999960032, -11.25833024919772463, -14.99999999999999822 ) ) ;
#27093 = CARTESIAN_POINT ( 'NONE',  ( 130.7287565553229456, -4.999999999999983125, 3.500000000000003109 ) ) ;
#27094 = VECTOR ( 'NONE', #18880, 1000.000000000000000 ) ;
#27095 = ADVANCED_FACE ( 'NONE', ( #23956 ), #5774, .T. ) ;
#27096 = DIRECTION ( 'NONE',  ( -2.698458740408365879E-16, 1.000000000000000000, 0.000000000000000000 ) ) ;
#27097 = CARTESIAN_POINT ( 'NONE',  ( 144.5152310637605808, -1.999999999999977129, -30.37205893520530964 ) ) ;
#27098 = EDGE_CURVE ( 'NONE', #14702, #11968, #29156, .T. ) ;
#27099 = FACE_OUTER_BOUND ( 'NONE', #10179, .T. ) ;
#27100 = CARTESIAN_POINT ( 'NONE',  ( 11.68823183152383471, 8.106166304734948369, -16.96230016324342671 ) ) ;
#27101 = CARTESIAN_POINT ( 'NONE',  ( 12.50016782010997751, 8.570776461014483871, -15.13004124836345632 ) ) ;
#27102 = CARTESIAN_POINT ( 'NONE',  ( 154.7287565553229172, -10.00000000000000178, 0.8205080756887930260 ) ) ;
#27103 = VERTEX_POINT ( 'NONE', #28706 ) ;
#27104 = CARTESIAN_POINT ( 'NONE',  ( 20.00000000000017053, 27.64101615137744972, 12.00000000000000178 ) ) ;
#27105 = CARTESIAN_POINT ( 'NONE',  ( 172.7287565553229740, -9.999999999999971578, 8.500000000000003553 ) ) ;
#27106 = ORIENTED_EDGE ( 'NONE', *, *, #1135, .F. ) ;
#27107 = CARTESIAN_POINT ( 'NONE',  ( 9.641350810849047548, 17.66889113945805789, -17.91928203681695564 ) ) ;
#27108 = VECTOR ( 'NONE', #29209, 1000.000000000000000 ) ;
#27109 = CARTESIAN_POINT ( 'NONE',  ( 133.6922820468854241, -10.00000000000000711, -26.58683881228715506 ) ) ;
#27110 = CARTESIAN_POINT ( 'NONE',  ( 14.65125771044925784, -5.000000000000013323, -45.09193465436170101 ) ) ;
#27111 = CARTESIAN_POINT ( 'NONE',  ( 23.84106988684860440, -4.080291168153947545, -13.50610408985603250 ) ) ;
#27112 = ORIENTED_EDGE ( 'NONE', *, *, #15930, .T. ) ;
#27113 = DIRECTION ( 'NONE',  ( -0.9510565162951536422, -2.566386769018988816E-16, -0.3090169943749472292 ) ) ;
#27114 = CARTESIAN_POINT ( 'NONE',  ( 11.05541531668977662, 17.68942339022145305, -17.98596209335946128 ) ) ;
#27115 = DIRECTION ( 'NONE',  ( -0.5877852522924731371, -1.586114251531760235E-16, 0.8090169943749474513 ) ) ;
#27116 = FACE_OUTER_BOUND ( 'NONE', #10843, .T. ) ;
#27117 = CARTESIAN_POINT ( 'NONE',  ( 23.21730923944814506, -4.364887171357101359, -13.63095412955673247 ) ) ;
#27118 = CARTESIAN_POINT ( 'NONE',  ( 172.7287565553229456, -4.999999999999970690, -36.50000000000000711 ) ) ;
#27119 = CARTESIAN_POINT ( 'NONE',  ( 20.66677465483945397, 4.408179161683285052, -13.64328152160912033 ) ) ;
#27120 = ORIENTED_EDGE ( 'NONE', *, *, #20617, .T. ) ;
#27121 = CARTESIAN_POINT ( 'NONE',  ( 47.87499999999999289, 0.000000000000000000, 0.000000000000000000 ) ) ;
#27122 = VECTOR ( 'NONE', #6362, 1000.000000000000000 ) ;
#27123 = SURFACE_STYLE_USAGE ( .BOTH. , #4495 ) ;
#27124 = CARTESIAN_POINT ( 'NONE',  ( 18.51594006248351931, 7.284897756227690202, -14.24483590514913089 ) ) ;
#27125 = CARTESIAN_POINT ( 'NONE',  ( 24.79321154704742725, 0.1008434151899674086, -19.04223803188042652 ) ) ;
#27126 = VECTOR ( 'NONE', #23625, 1000.000000000000000 ) ;
#27127 = ORIENTED_EDGE ( 'NONE', *, *, #23808, .F. ) ;
#27128 = CARTESIAN_POINT ( 'NONE',  ( 26.07968421886551980, -9.001936657367064498, -13.61655714643126913 ) ) ;
#27129 = VECTOR ( 'NONE', #27113, 1000.000000000000000 ) ;
#27130 = DIRECTION ( 'NONE',  ( 0.9510565162951535312, 2.566386769018988816E-16, -0.3090169943749475623 ) ) ;
#27131 = EDGE_CURVE ( 'NONE', #12245, #9455, #25746, .T. ) ;
#27132 = DIRECTION ( 'NONE',  ( 1.000000000000000000, 0.000000000000000000, 0.000000000000000000 ) ) ;
#27133 = LINE ( 'NONE', #19544, #3335 ) ;
#27134 = EDGE_CURVE ( 'NONE', #12148, #7328, #19641, .T. ) ;
#27135 = DIRECTION ( 'NONE',  ( 0.000000000000000000, 0.000000000000000000, 1.000000000000000000 ) ) ;
#27136 = EDGE_CURVE ( 'NONE', #3561, #19213, #10482, .T. ) ;
#27137 = FACE_OUTER_BOUND ( 'NONE', #9013, .T. ) ;
#27138 = CARTESIAN_POINT ( 'NONE',  ( 24.61983070264756890, -3.485318192270607351, -14.59657465048590907 ) ) ;
#27139 = CARTESIAN_POINT ( 'NONE',  ( 134.5152310637605808, -10.00000000000000533, -28.60870317832789311 ) ) ;
#27140 = CARTESIAN_POINT ( 'NONE',  ( 36.54859390953724585, -22.18451583373416014, -16.94733705004010460 ) ) ;
#27141 = CYLINDRICAL_SURFACE ( 'NONE', #17326, 5.000000000000000888 ) ;
#27142 = CARTESIAN_POINT ( 'NONE',  ( 11.92109019680886206, 8.606374460406147620, -15.56934379943068336 ) ) ;
#27143 = VECTOR ( 'NONE', #22695, 1000.000000000000000 ) ;
#27144 = CARTESIAN_POINT ( 'NONE',  ( 168.6922820468853388, -4.999999999999972466, -17.92658477444275889 ) ) ;
#27145 = CARTESIAN_POINT ( 'NONE',  ( 13.40933447225908992, 7.914523595725266425, -14.40541938743684902 ) ) ;
#27146 = CARTESIAN_POINT ( 'NONE',  ( 9.661930010240627809, 16.25461132122415364, -17.91197252329769185 ) ) ;
#27147 = CARTESIAN_POINT ( 'NONE',  ( 2.644994884459111351, -7.710515798486395234, -4.917753204360269415 ) ) ;
#27148 = VERTEX_POINT ( 'NONE', #10333 ) ;
#27149 = DIRECTION ( 'NONE',  ( 2.908569913943825554E-16, -1.000000000000000000, 0.000000000000000000 ) ) ;
#27150 = CARTESIAN_POINT ( 'NONE',  ( 9.921764701973689426, 16.38287729030320250, -16.50235149140834778 ) ) ;
#27151 = EDGE_LOOP ( 'NONE', ( #26409, #27995, #8732, #9806, #28217, #16567 ) ) ;
#27152 = VECTOR ( 'NONE', #22153, 1000.000000000000000 ) ;
#27153 = CARTESIAN_POINT ( 'NONE',  ( 146.1922820468854525, -1.999999999999977129, -30.91696583120935671 ) ) ;
#27154 = FACE_OUTER_BOUND ( 'NONE', #2637, .T. ) ;
#27155 = CIRCLE ( 'NONE', #2276, 3.000000000000002665 ) ;
#27156 = FACE_OUTER_BOUND ( 'NONE', #25992, .T. ) ;
#27157 = ORIENTED_EDGE ( 'NONE', *, *, #16690, .F. ) ;
#27158 = EDGE_LOOP ( 'NONE', ( #22604, #22772, #2333, #29230 ) ) ;
#27159 = CARTESIAN_POINT ( 'NONE',  ( 8.944716491630211763, 16.95098827139963049, -17.88239910762268181 ) ) ;
#27160 = CARTESIAN_POINT ( 'NONE',  ( 32.08869746025642655, -10.33200466608398216, -18.78962723441388150 ) ) ;
#27161 = VERTEX_POINT ( 'NONE', #17506 ) ;
#27162 = CARTESIAN_POINT ( 'NONE',  ( 22.38244025736702625, 4.876565640102752397, -15.59977576251379539 ) ) ;
#27163 = CARTESIAN_POINT ( 'NONE',  ( 28.92999000670439713, -5.550862855971650411, -17.57004703619191943 ) ) ;
#27164 = CARTESIAN_POINT ( 'NONE',  ( 104.5764801505170851, -4.999999999999988454, -75.97926025845912079 ) ) ;
#27165 = PLANE ( 'NONE',  #24819 ) ;
#27166 = LINE ( 'NONE', #4235, #11810 ) ;
#27167 = CARTESIAN_POINT ( 'NONE',  ( 22.33718609693395862, 3.185771058179875492, -16.53122240148476152 ) ) ;
#27168 = ADVANCED_FACE ( 'NONE', ( #24243 ), #9881, .T. ) ;
#27169 = VECTOR ( 'NONE', #28788, 1000.000000000000000 ) ;
#27170 = EDGE_CURVE ( 'NONE', #29723, #6582, #5927, .T. ) ;
#27171 = EDGE_LOOP ( 'NONE', ( #13911, #5584, #10676, #1920 ) ) ;
#27172 = DIRECTION ( 'NONE',  ( -2.698458740408365879E-16, 1.000000000000000000, 0.000000000000000000 ) ) ;
#27173 = EDGE_LOOP ( 'NONE', ( #25651, #4145, #1903, #17814 ) ) ;
#27174 = LINE ( 'NONE', #13388, #17998 ) ;
#27175 = AXIS2_PLACEMENT_3D ( 'NONE', #17830, #25173, #15393 ) ;
#27176 = ORIENTED_EDGE ( 'NONE', *, *, #13073, .F. ) ;
#27177 = EDGE_CURVE ( 'NONE', #21061, #17086, #3194, .T. ) ;
#27178 = CARTESIAN_POINT ( 'NONE',  ( 5.000000000000000000, 6.123233995736766282E-16, 18.00000000000000000 ) ) ;
#27180 = FACE_OUTER_BOUND ( 'NONE', #26231, .T. ) ;
#27179 = VECTOR ( 'NONE', #299, 999.9999999999998863 ) ;
#27181 = ADVANCED_FACE ( 'NONE', ( #19343 ), #3632, .T. ) ;
#27182 = EDGE_CURVE ( 'NONE', #29771, #29222, #3343, .T. ) ;
#27183 = ORIENTED_EDGE ( 'NONE', *, *, #16870, .F. ) ;
#27184 = ADVANCED_FACE ( 'NONE', ( #19193 ), #10028, .T. ) ;
#27185 = CARTESIAN_POINT ( 'NONE',  ( 12.03623766312057519, 9.280706639558555793, -16.68777662621714342 ) ) ;
#27186 = CARTESIAN_POINT ( 'NONE',  ( 35.35024494905714221, -20.29343902266242239, -19.25407150246939736 ) ) ;
#27187 = VECTOR ( 'NONE', #27549, 1000.000000000000000 ) ;
#27188 = VERTEX_POINT ( 'NONE', #14755 ) ;
#27189 = CARTESIAN_POINT ( 'NONE',  ( 9.117643650280985668, 16.15792227874146292, -17.05261013695411165 ) ) ;
#27190 = ORIENTED_EDGE ( 'NONE', *, *, #8991, .F. ) ;
#27191 = CARTESIAN_POINT ( 'NONE',  ( 26.08768104250457753, -11.87935956797728210, -17.28510650846989805 ) ) ;
#27192 = CARTESIAN_POINT ( 'NONE',  ( 12.88542016133816048, 9.523620991859985452, -16.10175225048900671 ) ) ;
#27193 = CARTESIAN_POINT ( 'NONE',  ( 176.1922820468852535, -1.999999999999970024, -4.936203717676158398 ) ) ;
#27194 = ORIENTED_EDGE ( 'NONE', *, *, #7321, .T. ) ;
#27195 = LINE ( 'NONE', #12805, #6129 ) ;
#27196 = CIRCLE ( 'NONE', #16906, 5.000000000000000888 ) ;
#27197 = CYLINDRICAL_SURFACE ( 'NONE', #11214, 5.000000000000000888 ) ;
#27198 = CARTESIAN_POINT ( 'NONE',  ( 151.1922820468854525, -10.00000000000000178, -30.91696583120936026 ) ) ;
#27199 = ORIENTED_EDGE ( 'NONE', *, *, #21041, .T. ) ;
#27200 = VERTEX_POINT ( 'NONE', #894 ) ;
#27201 = CARTESIAN_POINT ( 'NONE',  ( 168.6922820468853672, -9.999999999999996447, -26.58683881228715862 ) ) ;
#27202 = ORIENTED_EDGE ( 'NONE', *, *, #9126, .T. ) ;
#27203 = CARTESIAN_POINT ( 'NONE',  ( 13.13744203029165369, 8.576964204390579383, -15.90088637244482150 ) ) ;
#27204 = AXIS2_PLACEMENT_3D ( 'NONE', #20274, #20576, #8676 ) ;
#27205 = CARTESIAN_POINT ( 'NONE',  ( 14.98730560944732559, 2.974898859484017333, -15.20016081292634169 ) ) ;
#27206 = CARTESIAN_POINT ( 'NONE',  ( 20.25609397779747312, 2.611002146465201346, -20.92159891259701610 ) ) ;
#27207 = DIRECTION ( 'NONE',  ( -0.000000000000000000, 0.000000000000000000, 1.000000000000000000 ) ) ;
#27208 = ORIENTED_EDGE ( 'NONE', *, *, #27730, .T. ) ;
#27209 = FACE_OUTER_BOUND ( 'NONE', #22230, .T. ) ;
#27210 = ITEM_DEFINED_TRANSFORMATION ( 'NONE', 'NONE', #11691,  #13190 ) ;
#27211 = VERTEX_POINT ( 'NONE', #21944 ) ;
#27212 = CARTESIAN_POINT ( 'NONE',  ( 25.55230692589818631, -0.5649882819070038975, -17.32853901032857280 ) ) ;
#27213 = CARTESIAN_POINT ( 'NONE',  ( 0.8120000000000002771, -1.387778780781445429E-16, 5.000000000000000000 ) ) ;
#27214 = FACE_OUTER_BOUND ( 'NONE', #12014, .T. ) ;
#27215 = EDGE_CURVE ( 'NONE', #10352, #13853, #10185, .T. ) ;
#27216 = VECTOR ( 'NONE', #1223, 1000.000000000000000 ) ;
#27217 = ORIENTED_EDGE ( 'NONE', *, *, #18172, .T. ) ;
#27218 = EDGE_CURVE ( 'NONE', #6733, #18145, #12625, .T. ) ;
#27219 = EDGE_CURVE ( 'NONE', #8035, #23347, #8798, .T. ) ;
#27220 = DIRECTION ( 'NONE',  ( -1.000000000000000000, 0.000000000000000000, 0.000000000000000000 ) ) ;
#27221 = CARTESIAN_POINT ( 'NONE',  ( 33.37634376253905089, -12.42895282922877342, -19.69946502924221932 ) ) ;
#27222 = DIRECTION ( 'NONE',  ( 0.3090169943749472292, 8.338696094057992503E-17, -0.9510565162951536422 ) ) ;
#27223 = VECTOR ( 'NONE', #26008, 1000.000000000000000 ) ;
#27224 = VERTEX_POINT ( 'NONE', #8353 ) ;
#27225 = EDGE_LOOP ( 'NONE', ( #3504, #10693, #11788, #12426 ) ) ;
#27226 = CARTESIAN_POINT ( 'NONE',  ( 172.0152310637604671, -9.999999999999994671, -15.61832212156129707 ) ) ;
#27227 = CARTESIAN_POINT ( 'NONE',  ( 11.05541531668977662, 17.68942339022145305, -17.91752729848688830 ) ) ;
#27228 = CARTESIAN_POINT ( 'NONE',  ( 32.68951927270060764, -11.07419627511998605, -18.48540492261787449 ) ) ;
#27229 = ORIENTED_EDGE ( 'NONE', *, *, #7364, .F. ) ;
#27230 = DIRECTION ( 'NONE',  ( -0.5877852522924731371, 0.000000000000000000, 0.8090169943749474513 ) ) ;
#27231 = CARTESIAN_POINT ( 'NONE',  ( 10.66860827010606094, 9.045000281972594536, -16.41123175006880075 ) ) ;
#27232 = PLANE ( 'NONE',  #9778 ) ;
#27233 = LINE ( 'NONE', #22769, #18386 ) ;
#27234 = ORIENTED_EDGE ( 'NONE', *, *, #19233, .F. ) ;
#27235 = DIRECTION ( 'NONE',  ( 0.000000000000000000, 0.000000000000000000, -1.000000000000000000 ) ) ;
#27236 = ORIENTED_EDGE ( 'NONE', *, *, #23014, .F. ) ;
#27237 = CARTESIAN_POINT ( 'NONE',  ( 12.88542016133816048, 9.523620991859985452, -16.10175225048900671 ) ) ;
#27238 = ORIENTED_EDGE ( 'NONE', *, *, #5119, .F. ) ;
#27239 = CARTESIAN_POINT ( 'NONE',  ( 36.54006368622684420, -21.14619405898047688, -18.64381572867062076 ) ) ;
#27240 = CARTESIAN_POINT ( 'NONE',  ( 20.50636976340433293, -0.9757509181830721356, -19.91080244439677571 ) ) ;
#27241 = EDGE_LOOP ( 'NONE', ( #23202, #14447, #5027, #15676 ) ) ;
#27242 = AXIS2_PLACEMENT_3D ( 'NONE', #322, #13180, #1606 ) ;
#27243 = CARTESIAN_POINT ( 'NONE',  ( 174.7287565553228319, -1.999999999999970024, 0.8205080756887930260 ) ) ;
#27244 = LINE ( 'NONE', #1273, #19440 ) ;
#27245 = PLANE ( 'NONE',  #24222 ) ;
#27246 = EDGE_CURVE ( 'NONE', #1088, #18037, #8502, .T. ) ;
#27247 = VERTEX_POINT ( 'NONE', #1812 ) ;
#27248 = CARTESIAN_POINT ( 'NONE',  ( 25.05301747714807448, -9.477991407908255894, -18.78921932654604632 ) ) ;
#27249 = VECTOR ( 'NONE', #1425, 1000.000000000000000 ) ;
#27250 = CARTESIAN_POINT ( 'NONE',  ( 23.05283280155556724, -4.691836721735100468, -12.69353859562758124 ) ) ;
#27251 = ORIENTED_EDGE ( 'NONE', *, *, #21485, .F. ) ;
#27252 = ORIENTED_EDGE ( 'NONE', *, *, #22670, .F. ) ;
#27253 = FACE_OUTER_BOUND ( 'NONE', #11743, .T. ) ;
#27254 = PLANE ( 'NONE',  #9188 ) ;
#27255 = CARTESIAN_POINT ( 'NONE',  ( 13.00000000000000178, -2.870178842070716726E-15, -18.00000000000000000 ) ) ;
#27256 = EDGE_CURVE ( 'NONE', #7125, #29656, #3788, .T. ) ;
#27257 = DIRECTION ( 'NONE',  ( -1.000000000000000000, 0.000000000000000000, 0.000000000000000000 ) ) ;
#27258 = FACE_OUTER_BOUND ( 'NONE', #21171, .T. ) ;
#27259 = DIRECTION ( 'NONE',  ( 0.3090169943749475623, 8.338696094058001131E-17, 0.9510565162951536422 ) ) ;
#27260 = VECTOR ( 'NONE', #10815, 1000.000000000000000 ) ;
#27261 = UNCERTAINTY_MEASURE_WITH_UNIT (LENGTH_MEASURE( 1.000000000000000082E-05 ), #15008, 'distance_accuracy_value', 'NONE');
#27262 = CARTESIAN_POINT ( 'NONE',  ( 13.10901043280714084, 7.538357286119017786, -15.92110722978107873 ) ) ;
#27263 = CARTESIAN_POINT ( 'NONE',  ( 12.43696608443014284, 8.546664718661613591, -15.18012293544581226 ) ) ;
#27264 = CARTESIAN_POINT ( 'NONE',  ( 30.02037170576755187, -9.505783518442527225, -18.49971606337314967 ) ) ;
#27265 = EDGE_LOOP ( 'NONE', ( #10657, #7634, #24641, #17241 ) ) ;
#27266 = CARTESIAN_POINT ( 'NONE',  ( 0.000000000000000000, 0.000000000000000000, 19.04999999999997229 ) ) ;
#27267 = AXIS2_PLACEMENT_3D ( 'NONE', #25035, #25332, #4423 ) ;
#27268 = DIRECTION ( 'NONE',  ( -2.698458740408366372E-16, 1.000000000000000000, 0.000000000000000000 ) ) ;
#27269 = ORIENTED_EDGE ( 'NONE', *, *, #18942, .T. ) ;
#27270 = CARTESIAN_POINT ( 'NONE',  ( 9.643509238790151983, 17.65899231378470446, -17.74106871770035099 ) ) ;
#27271 = DIRECTION ( 'NONE',  ( -2.698458740408365879E-16, 1.000000000000000000, 0.000000000000000000 ) ) ;
#27272 = CARTESIAN_POINT ( 'NONE',  ( 159.5152310637604955, -9.999999999999998224, -21.71180489736091346 ) ) ;
#27273 = LINE ( 'NONE', #16063, #16662 ) ;
#27275 = EDGE_LOOP ( 'NONE', ( #25952, #13276, #4664, #13935 ) ) ;
#27274 = CARTESIAN_POINT ( 'NONE',  ( 25.36810815240369621, -0.9165050883202133791, -18.11329069065276443 ) ) ;
#27276 = VECTOR ( 'NONE', #22096, 1000.000000000000000 ) ;
#27277 = ORIENTED_EDGE ( 'NONE', *, *, #11861, .T. ) ;
#27278 = CARTESIAN_POINT ( 'NONE',  ( 164.5152310637604671, -1.999999999999972244, -13.05155085951651195 ) ) ;
#27279 = CARTESIAN_POINT ( 'NONE',  ( 11.05541531668977662, 17.68942339022145305, -19.66666666666843000 ) ) ;
#27280 = CARTESIAN_POINT ( 'NONE',  ( 33.06959603162382422, -11.76507887159725030, -17.56762491042838903 ) ) ;
#27281 = CARTESIAN_POINT ( 'NONE',  ( 164.7287565553228887, -9.999999999999998224, 0.8205080756887930260 ) ) ;
#27282 = CARTESIAN_POINT ( 'NONE',  ( 24.95482030053459965, -6.624749414579512496, -13.76522253407564733 ) ) ;
#27283 = CARTESIAN_POINT ( 'NONE',  ( 148.6922820468853956, -10.00000000000000178, -6.413161187712876909 ) ) ;
#27284 = CARTESIAN_POINT ( 'NONE',  ( 23.98539618923253514, -1.204509296099786297, -17.73462021633622143 ) ) ;
#27285 = EDGE_LOOP ( 'NONE', ( #3300, #8866, #27983, #20425, #27349 ) ) ;
#27286 = CARTESIAN_POINT ( 'NONE',  ( 137.2287565553230309, -4.999999999999980460, -20.83012701892219454 ) ) ;
#27287 = EDGE_CURVE ( 'NONE', #18174, #3603, #20104, .T. ) ;
#27288 = CARTESIAN_POINT ( 'NONE',  ( 18.55888777153046121, 10.80885496093247689, -16.87139299526244685 ) ) ;
#27289 = EDGE_CURVE ( 'NONE', #27662, #3793, #10642, .T. ) ;
#27290 = CARTESIAN_POINT ( 'NONE',  ( 25.07031029108804887, -10.85539403410516535, -16.40584363908930499 ) ) ;
#27291 = ORIENTED_EDGE ( 'NONE', *, *, #17916, .T. ) ;
#27292 = CARTESIAN_POINT ( 'NONE',  ( 24.87127057246125972, -9.548149280147088191, -14.79180087847266556 ) ) ;
#27293 = VECTOR ( 'NONE', #19293, 1000.000000000000000 ) ;
#27294 = AXIS2_PLACEMENT_3D ( 'NONE', #20084, #19621, #10619 ) ;
#27295 = FACE_OUTER_BOUND ( 'NONE', #27790, .T. ) ;
#27296 = AXIS2_PLACEMENT_3D ( 'NONE', #23645, #12181, #2744 ) ;
#27297 = LINE ( 'NONE', #26985, #26326 ) ;
#27298 = CARTESIAN_POINT ( 'NONE',  ( 17.99346030888765924, -5.000000000000012434, -55.37817656947992617 ) ) ;
#27299 = CARTESIAN_POINT ( 'NONE',  ( 129.5152310637605524, -10.00000000000000888, -4.391296821672111328 ) ) ;
#27300 = PLANE ( 'NONE',  #29739 ) ;
#27301 = CARTESIAN_POINT ( 'NONE',  ( 25.37470919123784086, -4.075530507763302168, -17.99687124876041011 ) ) ;
#27302 = CARTESIAN_POINT ( 'NONE',  ( 20.01918758985507196, 7.682949113293006782, -15.97060347488303123 ) ) ;
#27304 = ORIENTED_EDGE ( 'NONE', *, *, #20371, .T. ) ;
#27303 = CARTESIAN_POINT ( 'NONE',  ( 31.49515780845362301, -9.451207104696591088, -14.88922074032172205 ) ) ;
#27305 = DIRECTION ( 'NONE',  ( 6.938893903907227392E-16, -0.000000000000000000, 1.000000000000000000 ) ) ;
#27306 = CARTESIAN_POINT ( 'NONE',  ( 11.50832337395308436, 9.139936167900076569, -15.84372008594036885 ) ) ;
#27307 = PLANE ( 'NONE',  #25407 ) ;
#27308 = CARTESIAN_POINT ( 'NONE',  ( 162.0152310637604387, -4.999999999999974243, -8.721423840594312082 ) ) ;
#27309 = CARTESIAN_POINT ( 'NONE',  ( 13.12299649507002464, 8.570581087883812899, -15.91239967140973022 ) ) ;
#27310 = CARTESIAN_POINT ( 'NONE',  ( 24.67409968758932237, -5.000000000000010658, -75.93907040311476919 ) ) ;
#27311 = CARTESIAN_POINT ( 'NONE',  ( 149.5152310637605240, -4.999999999999976907, -2.627941064794695691 ) ) ;
#27312 = CARTESIAN_POINT ( 'NONE',  ( 10.33811693838771717, 18.38618951776012267, -17.92279151347708677 ) ) ;
#27313 = ORIENTED_EDGE ( 'NONE', *, *, #26147, .T. ) ;
#27314 = VECTOR ( 'NONE', #29716, 1000.000000000000114 ) ;
#27315 = LINE ( 'NONE', #17793, #11463 ) ;
#27316 = CARTESIAN_POINT ( 'NONE',  ( 134.5152310637605524, -10.00000000000000533, -13.05155085951650840 ) ) ;
#27317 = CARTESIAN_POINT ( 'NONE',  ( 162.0152310637604955, -9.999999999999998224, -26.04193191628311155 ) ) ;
#27318 = VECTOR ( 'NONE', #11694, 1000.000000000000000 ) ;
#27319 = ORIENTED_EDGE ( 'NONE', *, *, #16270, .T. ) ;
#27320 = CARTESIAN_POINT ( 'NONE',  ( 8.949836677108400806, 16.92750644812532457, -17.70396109330303958 ) ) ;
#27321 = CARTESIAN_POINT ( 'NONE',  ( 32.19500574710832552, -10.39459394146955518, -19.06308269698291014 ) ) ;
#27322 = EDGE_CURVE ( 'NONE', #6582, #4252, #20247, .T. ) ;
#27323 = EDGE_CURVE ( 'NONE', #18221, #4117, #13240, .T. ) ;
#27324 = CARTESIAN_POINT ( 'NONE',  ( 18.39217644224905257, 0.04847210594158309072, -18.71474297224575878 ) ) ;
#27325 = EDGE_CURVE ( 'NONE', #23789, #28630, #25766, .T. ) ;
#27326 = CARTESIAN_POINT ( 'NONE',  ( 27.20456514074317056, -5.347416052021189081, -13.22196079581408235 ) ) ;
#27327 = CARTESIAN_POINT ( 'NONE',  ( 154.5152310637605524, -1.999999999999974021, -30.37205893520531319 ) ) ;
#27328 = ADVANCED_FACE ( 'NONE', ( #13082 ), #24851, .T. ) ;
#27329 = CARTESIAN_POINT ( 'NONE',  ( 149.5152310637605808, -10.00000000000000178, -19.94844914048349693 ) ) ;
#27330 = CARTESIAN_POINT ( 'NONE',  ( 26.10879525372914145, -2.341005984040549937, -13.07697618282131913 ) ) ;
#27331 = ORIENTED_EDGE ( 'NONE', *, *, #16939, .F. ) ;
#27332 = CARTESIAN_POINT ( 'NONE',  ( 167.0152310637604671, -1.999999999999971800, -6.958068083716895558 ) ) ;
#27333 = AXIS2_PLACEMENT_3D ( 'NONE', #11705, #7588, #7140 ) ;
#27334 = EDGE_LOOP ( 'NONE', ( #25622, #29214, #11015, #1600 ) ) ;
#27335 = VECTOR ( 'NONE', #14212, 1000.000000000000000 ) ;
#27336 = DIRECTION ( 'NONE',  ( -0.000000000000000000, -0.000000000000000000, -1.000000000000000000 ) ) ;
#27337 = CARTESIAN_POINT ( 'NONE',  ( 172.2287565553228887, -1.999999999999970024, -12.16987298107780369 ) ) ;
#27338 = VECTOR ( 'NONE', #19924, 1000.000000000000000 ) ;
#27339 = LINE ( 'NONE', #13393, #25355 ) ;
#27340 = CARTESIAN_POINT ( 'NONE',  ( 32.72889690553877529, -10.93821547844579634, -14.37279655741261486 ) ) ;
#27341 = ORIENTED_EDGE ( 'NONE', *, *, #14203, .T. ) ;
#27342 = CARTESIAN_POINT ( 'NONE',  ( 10.66860827010606094, 9.045000281972594536, -16.41123175006880075 ) ) ;
#27343 = ORIENTED_EDGE ( 'NONE', *, *, #21561, .F. ) ;
#27344 = CARTESIAN_POINT ( 'NONE',  ( 25.90632082398269276, -12.28056132945115841, -15.12647891527467969 ) ) ;
#27345 = DIRECTION ( 'NONE',  ( 1.000000000000000000, 0.000000000000000000, 0.000000000000000000 ) ) ;
#27346 = CARTESIAN_POINT ( 'NONE',  ( 12.86835069890237548, 9.516077773083457814, -16.11535690708815594 ) ) ;
#27347 = CARTESIAN_POINT ( 'NONE',  ( 154.5152310637604955, -1.999999999999975353, -2.627941064794695691 ) ) ;
#27348 = ORIENTED_EDGE ( 'NONE', *, *, #3072, .T. ) ;
#27349 = ORIENTED_EDGE ( 'NONE', *, *, #16999, .T. ) ;
#27350 = AXIS2_PLACEMENT_3D ( 'NONE', #10134, #9836, #3000 ) ;
#27351 = DIRECTION ( 'NONE',  ( -2.698458740408365879E-16, 1.000000000000000000, 0.000000000000000000 ) ) ;
#27352 = CARTESIAN_POINT ( 'NONE',  ( 125.7287565553229172, -4.000000000000003553, -33.50000000000000000 ) ) ;
#27353 = DIRECTION ( 'NONE',  ( -0.9510565162951536422, 0.000000000000000000, -0.3090169943749472292 ) ) ;
#27354 = DIRECTION ( 'NONE',  ( 0.5877852522924731371, 1.586114251531760728E-16, -0.8090169943749474513 ) ) ;
#27355 = EDGE_LOOP ( 'NONE', ( #24902, #4746, #5703, #27236 ) ) ;
#27356 = CARTESIAN_POINT ( 'NONE',  ( 13.12278719711289732, 8.570488965836000617, -15.91256645732111430 ) ) ;
#27357 = VECTOR ( 'NONE', #8634, 1000.000000000000000 ) ;
#27358 = CARTESIAN_POINT ( 'NONE',  ( 22.87580194831562252, -0.07614860672512525908, -19.74465839296685132 ) ) ;
#27359 = CARTESIAN_POINT ( 'NONE',  ( 22.64650317123243894, 5.657944777580039997, -17.08144094666319646 ) ) ;
#27360 = EDGE_CURVE ( 'NONE', #21077, #20122, #1509, .T. ) ;
#27361 = VECTOR ( 'NONE', #15177, 1000.000000000000000 ) ;
#27362 = CARTESIAN_POINT ( 'NONE',  ( 176.1922820468852819, -9.999999999999994671, -13.59645775552055902 ) ) ;
#27363 = EDGE_CURVE ( 'NONE', #27772, #1053, #17950, .T. ) ;
#27364 = DIRECTION ( 'NONE',  ( -2.698458740408365879E-16, 1.000000000000000000, 0.000000000000000000 ) ) ;
#27365 = CONTEXT_DEPENDENT_SHAPE_REPRESENTATION ( #23935, #15178 ) ;
#27366 = CARTESIAN_POINT ( 'NONE',  ( 20.39549844898813191, -2.061726703908969505, -13.85117726305786512 ) ) ;
#27367 = EDGE_LOOP ( 'NONE', ( #2252, #12782, #9525, #18636 ) ) ;
#27368 = CARTESIAN_POINT ( 'NONE',  ( 2.099999999999999645, 9.325873406851305473E-16, -2.144516984716112518 ) ) ;
#27369 = VECTOR ( 'NONE', #5004, 999.9999999999998863 ) ;
#27370 = CARTESIAN_POINT ( 'NONE',  ( 147.2287565553230024, -1.999999999999976685, -12.16987298107780369 ) ) ;
#27371 = AXIS2_PLACEMENT_3D ( 'NONE', #17016, #553, #28654 ) ;
#27372 = ORIENTED_EDGE ( 'NONE', *, *, #19029, .F. ) ;
#27373 = CARTESIAN_POINT ( 'NONE',  ( 25.00000000000000000, 0.000000000000000000, 0.000000000000000000 ) ) ;
#27374 = CARTESIAN_POINT ( 'NONE',  ( 35.12509383387676820, -20.28195432802065312, -20.22992657050740917 ) ) ;
#27375 = DIRECTION ( 'NONE',  ( -2.698458740408365879E-16, 1.000000000000000000, 0.000000000000000000 ) ) ;
#27376 = EDGE_LOOP ( 'NONE', ( #3291, #20803, #11170, #12816 ) ) ;
#27377 = ORIENTED_EDGE ( 'NONE', *, *, #16004, .F. ) ;
#27378 = CARTESIAN_POINT ( 'NONE',  ( 14.41923689471965808, -5.000000000000014211, 44.37784800950869624 ) ) ;
#27379 = CARTESIAN_POINT ( 'NONE',  ( 16.01392728624657025, 9.853228751548474662, -15.03783782146776105 ) ) ;
#27380 = CARTESIAN_POINT ( 'NONE',  ( 12.24523703128252983, 9.516147632761573050, -15.33322559543412034 ) ) ;
#27381 = CARTESIAN_POINT ( 'NONE',  ( 33.54145741815126058, -13.16751478770765793, -19.75123935038191192 ) ) ;
#27382 = ORIENTED_EDGE ( 'NONE', *, *, #10991, .F. ) ;
#27383 = DIRECTION ( 'NONE',  ( 1.000000000000000000, 0.000000000000000000, 0.000000000000000000 ) ) ;
#27384 = CARTESIAN_POINT ( 'NONE',  ( 9.641350810849047548, 17.66889113945805789, -17.92015940598198753 ) ) ;
#27385 = LINE ( 'NONE', #1566, #20999 ) ;
#27386 = SURFACE_STYLE_FILL_AREA ( #20459 ) ;
#27387 = EDGE_LOOP ( 'NONE', ( #2197, #13633, #13586, #8254 ) ) ;
#27388 = ORIENTED_EDGE ( 'NONE', *, *, #14397, .F. ) ;
#27389 = DIRECTION ( 'NONE',  ( -0.5877852522924731371, -1.586114251531760728E-16, -0.8090169943749474513 ) ) ;
#27390 = VERTEX_POINT ( 'NONE', #25004 ) ;
#27391 = CARTESIAN_POINT ( 'NONE',  ( 12.87521155010636242, 9.519109623917222152, -16.10988869383489686 ) ) ;
#27392 = AXIS2_PLACEMENT_3D ( 'NONE', #26373, #19624, #12606 ) ;
#27394 = AXIS2_PLACEMENT_3D ( 'NONE', #25353, #4446, #11442 ) ;
#27393 = CARTESIAN_POINT ( 'NONE',  ( 33.33685173283005554, -10.38074443705513161, -18.09276096107157628 ) ) ;
#27395 = CARTESIAN_POINT ( 'NONE',  ( 19.61192361542596529, -2.405681417800469291, -14.70675912396028906 ) ) ;
#27396 = EDGE_CURVE ( 'NONE', #475, #2286, #4087, .T. ) ;
#27397 = ADVANCED_FACE ( 'NONE', ( #1354 ), #19952, .T. ) ;
#27398 = FACE_OUTER_BOUND ( 'NONE', #15666, .T. ) ;
#27399 = ADVANCED_FACE ( 'NONE', ( #21738, #26957, #17160 ), #26800, .F. ) ;
#27400 = FACE_OUTER_BOUND ( 'NONE', #1045, .T. ) ;
#27401 = CARTESIAN_POINT ( 'NONE',  ( 30.68845550234816244, -8.154108532121835395, -15.50657635367809917 ) ) ;
#27402 = CARTESIAN_POINT ( 'NONE',  ( 23.39714218815755231, -8.028440028060597200, -17.83143846932372512 ) ) ;
#27403 = ORIENTED_EDGE ( 'NONE', *, *, #6879, .T. ) ;
#27404 = CYLINDRICAL_SURFACE ( 'NONE', #14721, 8.000000000000000000 ) ;
#27405 = VECTOR ( 'NONE', #23130, 1000.000000000000000 ) ;
#27406 = CARTESIAN_POINT ( 'NONE',  ( 169.5152310637604671, -1.999999999999970468, -21.71180489736091346 ) ) ;
#27407 = DIRECTION ( 'NONE',  ( -2.698458740408365879E-16, 1.000000000000000000, 0.000000000000000000 ) ) ;
#27408 = VECTOR ( 'NONE', #6818, 1000.000000000000000 ) ;
#27409 = DIRECTION ( 'NONE',  ( 0.000000000000000000, 0.000000000000000000, 1.000000000000000000 ) ) ;
#27410 = CARTESIAN_POINT ( 'NONE',  ( 11.24427277393626134, 9.004760228429224966, -17.23264536074314179 ) ) ;
#27411 = CARTESIAN_POINT ( 'NONE',  ( 10.33811689237846743, 18.38618972876440338, -17.91642382710546855 ) ) ;
#27412 = CARTESIAN_POINT ( 'NONE',  ( 172.0152310637604955, -1.999999999999969358, -34.70218595412750773 ) ) ;
#27413 = ORIENTED_EDGE ( 'NONE', *, *, #1515, .F. ) ;
#27414 = CARTESIAN_POINT ( 'NONE',  ( 174.7287565553228603, -1.999999999999969580, -7.839745962155603820 ) ) ;
#27415 = VERTEX_POINT ( 'NONE', #15301 ) ;
#27416 = CARTESIAN_POINT ( 'NONE',  ( 9.641350944112486943, 17.66889052829492002, -17.91441860517739215 ) ) ;
#27417 = LINE ( 'NONE', #25805, #16461 ) ;
#27418 = CARTESIAN_POINT ( 'NONE',  ( 17.88967384018823026, 7.017424582044266224, -15.49508032100559696 ) ) ;
#27419 = CARTESIAN_POINT ( 'NONE',  ( 167.0152310637604671, -1.999999999999971356, -17.38167787843871182 ) ) ;
#27420 = DIRECTION ( 'NONE',  ( -0.9510565162951536422, -2.566386769018988816E-16, -0.3090169943749472292 ) ) ;
#27422 = VERTEX_POINT ( 'NONE', #19442 ) ;
#27421 = CARTESIAN_POINT ( 'NONE',  ( 26.31132954256896639, -3.159408024760113509, -14.81636702655834803 ) ) ;
#27423 = ORIENTED_EDGE ( 'NONE', *, *, #16348, .F. ) ;
#27424 = DIRECTION ( 'NONE',  ( 0.9510565162951536422, 2.566386769018988816E-16, 0.3090169943749472292 ) ) ;
#27425 = CARTESIAN_POINT ( 'NONE',  ( 12.24611073458536836, 9.516504178424655791, -15.33253149294119311 ) ) ;
#27426 = CARTESIAN_POINT ( 'NONE',  ( 33.75544676243647757, -14.12885555826641593, -19.81592319558764004 ) ) ;
#27427 = LINE ( 'NONE', #22356, #28875 ) ;
#27428 = CARTESIAN_POINT ( 'NONE',  ( 27.91615220763155847, -6.225400021157185826, -17.67258836524805332 ) ) ;
#27429 = DIRECTION ( 'NONE',  ( -2.698458740408365879E-16, 1.000000000000000000, 0.000000000000000000 ) ) ;
#27430 = CARTESIAN_POINT ( 'NONE',  ( 23.60892706051935619, -2.861763136178346212, -14.25286661070829908 ) ) ;
#27431 = EDGE_CURVE ( 'NONE', #3757, #14105, #30223, .T. ) ;
#27432 = ORIENTED_EDGE ( 'NONE', *, *, #4643, .F. ) ;
#27433 = ADVANCED_FACE ( 'NONE', ( #839 ), #24633, .T. ) ;
#27434 = DIRECTION ( 'NONE',  ( -0.5877852522924731371, -1.586114251531760235E-16, 0.8090169943749474513 ) ) ;
#27435 = CARTESIAN_POINT ( 'NONE',  ( 30.28780241637438664, -8.987295266975118935, -19.34112676082218840 ) ) ;
#27436 = CARTESIAN_POINT ( 'NONE',  ( 29.37945295281542712, -10.41679561567529433, -17.92877087918597212 ) ) ;
#27437 = ORIENTED_EDGE ( 'NONE', *, *, #11830, .T. ) ;
#27438 = LINE ( 'NONE', #11354, #4887 ) ;
#27439 = PRODUCT ( 'BR-593', 'BR-593', '', ( #5053 ) ) ;
#27440 = AXIS2_PLACEMENT_3D ( 'NONE', #537, #17292, #26945 ) ;
#27441 = DIRECTION ( 'NONE',  ( -0.9510565162951536422, 0.000000000000000000, -0.3090169943749472292 ) ) ;
#27442 = VERTEX_POINT ( 'NONE', #10584 ) ;
#27443 = LINE ( 'NONE', #20078, #15095 ) ;
#27444 = DIRECTION ( 'NONE',  ( -2.698458740408365879E-16, 1.000000000000000000, 0.000000000000000000 ) ) ;
#27445 = CARTESIAN_POINT ( 'NONE',  ( 16.00468163665589572, -5.000000000000013323, -49.25734519086697105 ) ) ;
#27446 = CIRCLE ( 'NONE', #8874, 6.999999999999999112 ) ;
#27447 = CARTESIAN_POINT ( 'NONE',  ( 12.74999999999999822, 0.000000000000000000, 0.000000000000000000 ) ) ;
#27448 = CARTESIAN_POINT ( 'NONE',  ( 23.79992313191835507, -8.927985498448517632, -17.01055530912027791 ) ) ;
#27449 = CARTESIAN_POINT ( 'NONE',  ( 16.38240814442996651, 6.370603895193741373, -13.89573738210111919 ) ) ;
#27450 = EDGE_CURVE ( 'NONE', #28182, #17358, #24336, .T. ) ;
#27452 = ORIENTED_EDGE ( 'NONE', *, *, #307, .F. ) ;
#27451 = CARTESIAN_POINT ( 'NONE',  ( 32.21775685856648153, -9.560954865089090760, -16.93152350858319366 ) ) ;
#27453 = DIRECTION ( 'NONE',  ( -2.698458740408365879E-16, 1.000000000000000000, 0.000000000000000000 ) ) ;
#27454 = CARTESIAN_POINT ( 'NONE',  ( 12.50016782010997751, 8.570776461014483871, -15.13004124836345632 ) ) ;
#27455 = PRODUCT_DEFINITION ( 'UNKNOWN', '', #8752, #25677 ) ;
#27456 = LINE ( 'NONE', #3769, #6392 ) ;
#27457 = LINE ( 'NONE', #6507, #23670 ) ;
#27458 = CARTESIAN_POINT ( 'NONE',  ( 9.708396314890595846, 16.04151092502291931, -17.86831624201546020 ) ) ;
#27459 = DIRECTION ( 'NONE',  ( -0.9510565162951536422, -2.566386769018988816E-16, -0.3090169943749472292 ) ) ;
#27460 = EDGE_LOOP ( 'NONE', ( #21297, #7922, #14823, #19153 ) ) ;
#27461 = CARTESIAN_POINT ( 'NONE',  ( 143.6922820468853956, -4.999999999999978684, 2.247092850131519715 ) ) ;
#27462 = CARTESIAN_POINT ( 'NONE',  ( 12.71834232392635045, 8.667191563245470576, -14.95615232649864090 ) ) ;
#27463 = ORIENTED_EDGE ( 'NONE', *, *, #9296, .F. ) ;
#27464 = CARTESIAN_POINT ( 'NONE',  ( 0.000000000000000000, 0.000000000000000000, -23.00000000000000000 ) ) ;
#27465 = DIRECTION ( 'NONE',  ( 0.5877852522924731371, 1.586114251531760728E-16, 0.8090169943749474513 ) ) ;
#27466 = CARTESIAN_POINT ( 'NONE',  ( 137.0152310637605524, -10.00000000000000533, -0.06116980274991495881 ) ) ;
#27467 = ORIENTED_EDGE ( 'NONE', *, *, #5676, .F. ) ;
#27468 = CARTESIAN_POINT ( 'NONE',  ( 13.81482270056995532, 7.818281081198240834, -15.36100202165747675 ) ) ;
#27469 = CARTESIAN_POINT ( 'NONE',  ( 36.01637063434644404, -20.79351858480864124, -21.36424221831693870 ) ) ;
#27470 = CARTESIAN_POINT ( 'NONE',  ( 21.98221344960014889, 4.819993630401092410, -14.81438138791982162 ) ) ;
#27471 = CARTESIAN_POINT ( 'NONE',  ( 17.37262532792671976, 6.041285449496323068, -14.53661901313261495 ) ) ;
#27472 = VECTOR ( 'NONE', #29158, 1000.000000000000000 ) ;
#27473 = LINE ( 'NONE', #27769, #15712 ) ;
#27474 = CARTESIAN_POINT ( 'NONE',  ( 21.92900763033978251, 0.1816185532145172810, -13.27135403042708717 ) ) ;
#27475 = EDGE_LOOP ( 'NONE', ( #18029, #4147, #3887, #18919 ) ) ;
#27476 = CARTESIAN_POINT ( 'NONE',  ( 15.60617273857451615, -5.000000000000013323, -48.03086091582405714 ) ) ;
#27478 = EDGE_LOOP ( 'NONE', ( #19858, #11744, #7673, #18409 ) ) ;
#27477 = DIRECTION ( 'NONE',  ( 0.3331260486002958765, -0.05059491534325381845, -0.9415238660200613285 ) ) ;
#27479 = CARTESIAN_POINT ( 'NONE',  ( 169.5152310637604955, -4.999999999999971578, -19.94844914048349693 ) ) ;
#27480 = CARTESIAN_POINT ( 'NONE',  ( 0.000000000000000000, 0.000000000000000000, -18.00000000000000000 ) ) ;
#27481 = LINE ( 'NONE', #20855, #5859 ) ;
#27482 = EDGE_CURVE ( 'NONE', #28787, #26475, #12569, .T. ) ;
#27483 = EDGE_CURVE ( 'NONE', #4938, #12612, #3730, .T. ) ;
#27484 = CARTESIAN_POINT ( 'NONE',  ( 34.00275312277798889, -11.14511497259480244, -17.96532559481354596 ) ) ;
#27485 = ORIENTED_EDGE ( 'NONE', *, *, #2008, .T. ) ;
#27486 = CARTESIAN_POINT ( 'NONE',  ( 10.71071464234916348, 8.878904022500222482, -16.39175934796422851 ) ) ;
#27487 = EDGE_CURVE ( 'NONE', #24460, #14791, #19890, .T. ) ;
#27488 = EDGE_LOOP ( 'NONE', ( #1090, #29001, #17391, #18634 ) ) ;
#27489 = AXIS2_PLACEMENT_3D ( 'NONE', #23015, #13538, #4678 ) ;
#27490 = DIRECTION ( 'NONE',  ( 0.9510565162951536422, 2.566386769018988816E-16, 0.3090169943749472292 ) ) ;
#27491 = DIRECTION ( 'NONE',  ( 0.9773680663943724589, 5.871577894680259423E-18, -0.2115458881484709175 ) ) ;
#27492 = CARTESIAN_POINT ( 'NONE',  ( 10.79618582965528439, 14.96552620561766567, -17.20075070836251996 ) ) ;
#27493 = DIRECTION ( 'NONE',  ( 1.110223024625156540E-16, 2.995891024602366092E-32, 1.000000000000000000 ) ) ;
#27494 = ORIENTED_EDGE ( 'NONE', *, *, #9715, .T. ) ;
#27495 = ORIENTED_EDGE ( 'NONE', *, *, #3108, .F. ) ;
#27496 = FACE_OUTER_BOUND ( 'NONE', #10471, .T. ) ;
#27497 = LINE ( 'NONE', #6704, #27845 ) ;
#27499 = ORIENTED_EDGE ( 'NONE', *, *, #9715, .F. ) ;
#27498 = LINE ( 'NONE', #19763, #19360 ) ;
#27500 = ORIENTED_EDGE ( 'NONE', *, *, #17246, .T. ) ;
#27501 = LINE ( 'NONE', #19980, #12501 ) ;
#27502 = ORIENTED_EDGE ( 'NONE', *, *, #6640, .F. ) ;
#27503 = CARTESIAN_POINT ( 'NONE',  ( 13.55939796120610019, 8.763434079353435990, -15.56458004748339619 ) ) ;
#27504 = ORIENTED_EDGE ( 'NONE', *, *, #1169, .T. ) ;
#27505 = CARTESIAN_POINT ( 'NONE',  ( 19.73194482477335399, 0.5267938184197646923, -13.16654652480547583 ) ) ;
#27506 = CARTESIAN_POINT ( 'NONE',  ( 22.00422591904570879, -4.533096263764313072, -16.84388275221259690 ) ) ;
#27507 = CARTESIAN_POINT ( 'NONE',  ( 18.75392633456350922, 0.8452085672475394551, -14.97946080469353447 ) ) ;
#27508 = LINE ( 'NONE', #15850, #3340 ) ;
#27509 = CARTESIAN_POINT ( 'NONE',  ( 161.1922820468853956, -9.999999999999998224, -30.91696583120936026 ) ) ;
#27510 = CARTESIAN_POINT ( 'NONE',  ( 23.36212950203212557, 2.915605996956767587, -15.34809340432955693 ) ) ;
#27511 = VECTOR ( 'NONE', #987, 1000.000000000000000 ) ;
#27512 = CARTESIAN_POINT ( 'NONE',  ( 166.1922820468853104, -9.999999999999998224, -4.936203717676158398 ) ) ;
#27513 = DIRECTION ( 'NONE',  ( 0.5877852522924731371, 0.000000000000000000, 0.8090169943749474513 ) ) ;
#27514 = VERTEX_POINT ( 'NONE', #24047 ) ;
#27515 = DIRECTION ( 'NONE',  ( -0.5877852522924731371, -1.586114251531760728E-16, -0.8090169943749474513 ) ) ;
#27516 = ADVANCED_FACE ( 'NONE', ( #12871 ), #25293, .T. ) ;
#27517 = CARTESIAN_POINT ( 'NONE',  ( 134.7287565553230024, -10.00000000000000711, -7.839745962155602044 ) ) ;
#27518 = CARTESIAN_POINT ( 'NONE',  ( -2.500000000000000444, -8.040613248383173881E-16, -2.450000000000000622 ) ) ;
#27519 = ORIENTED_EDGE ( 'NONE', *, *, #26970, .F. ) ;
#27520 = EDGE_CURVE ( 'NONE', #15766, #28338, #15153, .T. ) ;
#27521 = ORIENTED_EDGE ( 'NONE', *, *, #28913, .T. ) ;
#27522 = DIRECTION ( 'NONE',  ( -0.9510565162951536422, -2.566386769018988323E-16, 0.3090169943749475623 ) ) ;
#27523 = ADVANCED_FACE ( 'NONE', ( #7851 ), #12722, .T. ) ;
#27524 = CARTESIAN_POINT ( 'NONE',  ( 14.33367420948735393, 6.252843122977492563, -16.41390433006782956 ) ) ;
#27525 = CARTESIAN_POINT ( 'NONE',  ( 11.05541531668977662, 17.68942339022145305, -19.66666666666843000 ) ) ;
#27526 = CARTESIAN_POINT ( 'NONE',  ( 35.02155038278115740, -19.81678845073966500, -20.19863594638463411 ) ) ;
#27527 = EDGE_LOOP ( 'NONE', ( #28744, #4345, #12053, #13789 ) ) ;
#27528 = DIRECTION ( 'NONE',  ( -1.110223024625156540E-16, 0.000000000000000000, -1.000000000000000000 ) ) ;
#27529 = VECTOR ( 'NONE', #16916, 1000.000000000000000 ) ;
#27530 = CARTESIAN_POINT ( 'NONE',  ( 12.75517096047518173, 7.625437268557950787, -14.92679923539383680 ) ) ;
#27531 = CARTESIAN_POINT ( 'NONE',  ( 137.2287565553230309, -1.999999999999979572, -12.16987298107780013 ) ) ;
#27532 = DIRECTION ( 'NONE',  ( 6.938893903907227392E-16, -0.000000000000000000, 1.000000000000000000 ) ) ;
#27533 = EDGE_LOOP ( 'NONE', ( #4834, #2700, #23671, #22870 ) ) ;
#27534 = DIRECTION ( 'NONE',  ( 0.5877852522924731371, 0.000000000000000000, 0.8090169943749474513 ) ) ;
#27535 = ORIENTED_EDGE ( 'NONE', *, *, #21763, .T. ) ;
#27536 = CARTESIAN_POINT ( 'NONE',  ( 12.86751881037522871, 9.515731068868671372, -16.11601834121851340 ) ) ;
#27537 = CARTESIAN_POINT ( 'NONE',  ( 33.36027191889437660, -10.38700102556154903, -18.15738432823107473 ) ) ;
#27538 = CARTESIAN_POINT ( 'NONE',  ( 21.16681283796276603, -5.103637247178538061, -17.00692323485822754 ) ) ;
#27539 = ORIENTED_EDGE ( 'NONE', *, *, #9796, .T. ) ;
#27540 = DIRECTION ( 'NONE',  ( 1.000000000000000000, 0.000000000000000000, 0.000000000000000000 ) ) ;
#27541 = LINE ( 'NONE', #33, #6454 ) ;
#27542 = SURFACE_SIDE_STYLE ('',( #6595 ) ) ;
#27543 = CARTESIAN_POINT ( 'NONE',  ( 24.79209089726652948, -9.725099617967893906, -18.44766554224525734 ) ) ;
#27544 = CARTESIAN_POINT ( 'NONE',  ( 25.61803826562323394, -0.4625480611756047078, -19.10237625710802334 ) ) ;
#27545 = ORIENTED_EDGE ( 'NONE', *, *, #7774, .T. ) ;
#27546 = DIRECTION ( 'NONE',  ( -2.698458740408365879E-16, 1.000000000000000000, 0.000000000000000000 ) ) ;
#27547 = VECTOR ( 'NONE', #6499, 1000.000000000000000 ) ;
#27548 = ORIENTED_EDGE ( 'NONE', *, *, #13147, .T. ) ;
#27549 = DIRECTION ( 'NONE',  ( -0.5877852522924731371, -1.586114251531760235E-16, 0.8090169943749474513 ) ) ;
#27550 = CARTESIAN_POINT ( 'NONE',  ( 0.000000000000000000, 0.000000000000000000, 1.700000000000000178 ) ) ;
#27551 = EDGE_CURVE ( 'NONE', #16634, #6979, #3582, .T. ) ;
#27552 = CARTESIAN_POINT ( 'NONE',  ( 8.000000000000001776, 4.336808689942017736E-15, 0.000000000000000000 ) ) ;
#27553 = ADVANCED_FACE ( 'NONE', ( #8143 ), #29261, .T. ) ;
#27554 = EDGE_CURVE ( 'NONE', #13154, #22282, #3145, .T. ) ;
#27555 = CARTESIAN_POINT ( 'NONE',  ( 12.51757296969303290, 8.578467993704791184, -15.11616904564172792 ) ) ;
#27556 = EDGE_CURVE ( 'NONE', #22891, #28379, #28813, .T. ) ;
#27557 = DIRECTION ( 'NONE',  ( -0.000000000000000000, -1.000000000000000000, -0.000000000000000000 ) ) ;
#27558 = ORIENTED_EDGE ( 'NONE', *, *, #897, .T. ) ;
#27559 = PLANE ( 'NONE',  #12002 ) ;
#27560 = EDGE_LOOP ( 'NONE', ( #3927, #8169, #7541, #29190 ) ) ;
#27561 = CARTESIAN_POINT ( 'NONE',  ( 9.879812780108833792, 16.57527415160161510, -16.52987074417163527 ) ) ;
#27562 = CARTESIAN_POINT ( 'NONE',  ( 16.99436549934495133, 9.190724047982882894, -15.08166918603070528 ) ) ;
#27563 = PLANE ( 'NONE',  #11709 ) ;
#27564 = DIRECTION ( 'NONE',  ( -0.9510565162951536422, -2.566386769018988323E-16, 0.3090169943749475623 ) ) ;
#27565 = CARTESIAN_POINT ( 'NONE',  ( 22.97938783112199701, -3.359759438970757017, -19.62490732200095067 ) ) ;
#27566 = ORIENTED_EDGE ( 'NONE', *, *, #4317, .T. ) ;
#27567 = PLANE ( 'NONE',  #18344 ) ;
#27568 = CARTESIAN_POINT ( 'NONE',  ( 12.24525513380350539, 9.516155168367477657, -15.33321120281095773 ) ) ;
#27569 = CARTESIAN_POINT ( 'NONE',  ( 34.96805304670973413, -19.57645325810014114, -20.18246498508359466 ) ) ;
#27570 = CARTESIAN_POINT ( 'NONE',  ( 156.1922820468853672, -10.00000000000000000, -13.59645775552055902 ) ) ;
#27571 = CARTESIAN_POINT ( 'NONE',  ( 25.23810427664335165, -6.496417100615061280, -13.69959235629456629 ) ) ;
#27572 = VECTOR ( 'NONE', #5217, 1000.000000000000000 ) ;
#27573 = FACE_OUTER_BOUND ( 'NONE', #29056, .T. ) ;
#27574 = CARTESIAN_POINT ( 'NONE',  ( 23.40821609032294859, 1.473297984346819245, -16.37969033120859308 ) ) ;
#27575 = EDGE_LOOP ( 'NONE', ( #971, #19698, #13871, #12921, #12847, #2551 ) ) ;
#27576 = CYLINDRICAL_SURFACE ( 'NONE', #820, 5.000000000000000888 ) ;
#27577 = CARTESIAN_POINT ( 'NONE',  ( 15.33641899704135980, 5.898237403637139664, -14.35162154369138676 ) ) ;
#27578 = CARTESIAN_POINT ( 'NONE',  ( 30.58694070296994028, -11.15840821071237698, -14.58880109071565556 ) ) ;
#27579 = ORIENTED_EDGE ( 'NONE', *, *, #21269, .F. ) ;
#27580 = VERTEX_POINT ( 'NONE', #5570 ) ;
#27581 = LINE ( 'NONE', #6637, #532 ) ;
#27582 = DIRECTION ( 'NONE',  ( -0.9510565162951536422, -2.566386769018988323E-16, 0.3090169943749475623 ) ) ;
#27583 = CARTESIAN_POINT ( 'NONE',  ( -0.000000000000000000, 55.00000000000000711, 18.00000000000000000 ) ) ;
#27584 = DIRECTION ( 'NONE',  ( 0.000000000000000000, 0.000000000000000000, -1.000000000000000000 ) ) ;
#27585 = EDGE_CURVE ( 'NONE', #16407, #9840, #14848, .T. ) ;
#27586 = DIRECTION ( 'NONE',  ( -2.698458740408365879E-16, 1.000000000000000000, 0.000000000000000000 ) ) ;
#27587 = AXIS2_PLACEMENT_3D ( 'NONE', #15866, #11294, #14020 ) ;
#27588 = EDGE_CURVE ( 'NONE', #12381, #25113, #11567, .T. ) ;
#27589 = CARTESIAN_POINT ( 'NONE',  ( 174.5152310637604955, -9.999999999999994671, -28.60870317832789667 ) ) ;
#27590 = EDGE_CURVE ( 'NONE', #23064, #705, #7546, .T. ) ;
#27591 = CARTESIAN_POINT ( 'NONE',  ( 27.87740037347163735, -3.310382910926334521, -16.69022314910379734 ) ) ;
#27592 = CARTESIAN_POINT ( 'NONE',  ( 18.25949499138229726, 0.6315596619015936275, -15.69045325149238934 ) ) ;
#27593 = CARTESIAN_POINT ( 'NONE',  ( 36.26977878907645447, -21.93194718998534753, -20.87741241889870736 ) ) ;
#27594 = DIRECTION ( 'NONE',  ( 0.000000000000000000, -1.000000000000000000, 0.000000000000000000 ) ) ;
#27595 = CARTESIAN_POINT ( 'NONE',  ( 11.47395765415086188, 9.264374527449886543, -15.86046114005151075 ) ) ;
#27596 = CARTESIAN_POINT ( 'NONE',  ( 15.00000000000000000, 1.387778780781445429E-16, -5.000000000000000000 ) ) ;
#27597 = DIRECTION ( 'NONE',  ( 1.000000000000000000, 2.698458740408365879E-16, -1.110223024625156540E-16 ) ) ;
#27598 = CARTESIAN_POINT ( 'NONE',  ( 9.675977061968080051, 16.19018975141917593, -17.88172274351348889 ) ) ;
#27599 = CARTESIAN_POINT ( 'NONE',  ( 15.00000000000000000, -1.252609127533332839E-16, 4.513000000000000789 ) ) ;
#27600 = ORIENTED_EDGE ( 'NONE', *, *, #9446, .F. ) ;
#27601 = CARTESIAN_POINT ( 'NONE',  ( 125.7287565553229456, -9.999999999999994671, 0.5000000000000143219 ) ) ;
#27602 = CARTESIAN_POINT ( 'NONE',  ( 11.97192087863669663, 8.579774655713777065, -15.53257280409644991 ) ) ;
#27603 = VECTOR ( 'NONE', #28655, 1000.000000000000000 ) ;
#27604 = ORIENTED_EDGE ( 'NONE', *, *, #27042, .T. ) ;
#27605 = CARTESIAN_POINT ( 'NONE',  ( 154.5152310637605524, -10.00000000000000000, -30.37205893520531319 ) ) ;
#27606 = DIRECTION ( 'NONE',  ( 0.5877852522924731371, 1.586114251531760728E-16, -0.8090169943749474513 ) ) ;
#27607 = CARTESIAN_POINT ( 'NONE',  ( 139.5152310637605808, -1.999999999999978684, -13.05155085951651195 ) ) ;
#27608 = ORIENTED_EDGE ( 'NONE', *, *, #16347, .T. ) ;
#27609 = CARTESIAN_POINT ( 'NONE',  ( 9.436770671236972774, 14.69436508140356246, -16.92063988783295159 ) ) ;
#27610 = CARTESIAN_POINT ( 'NONE',  ( 34.92716911317440065, -20.39278340154575631, -21.20741747040485592 ) ) ;
#27611 = CARTESIAN_POINT ( 'NONE',  ( 15.25645860304719292, 2.347722246533389789, -18.19294613283020112 ) ) ;
#27612 = VECTOR ( 'NONE', #3252, 1000.000000000000000 ) ;
#27613 = CARTESIAN_POINT ( 'NONE',  ( 19.59003110916602708, 6.792398362604423312, -16.15450529561476500 ) ) ;
#27614 = PRESENTATION_LAYER_ASSIGNMENT (  '', '', ( #21227 ) ) ;
#27615 = DIRECTION ( 'NONE',  ( 0.000000000000000000, 0.000000000000000000, 1.000000000000000000 ) ) ;
#27616 = CARTESIAN_POINT ( 'NONE',  ( 24.28706804496593463, -0.4963248009486594392, -19.74393692370418307 ) ) ;
#27617 = EDGE_CURVE ( 'NONE', #22145, #12691, #16498, .T. ) ;
#27618 = EDGE_CURVE ( 'NONE', #19921, #29111, #11138, .T. ) ;
#27619 = ORIENTED_EDGE ( 'NONE', *, *, #26253, .T. ) ;
#27620 = CARTESIAN_POINT ( 'NONE',  ( -7.999999999999998224, 1.572549600175623841, -4.931055444744870009 ) ) ;
#27622 = ORIENTED_EDGE ( 'NONE', *, *, #14651, .F. ) ;
#27621 = CARTESIAN_POINT ( 'NONE',  ( 144.7287565553230309, -1.999999999999977129, -16.50000000000000355 ) ) ;
#27623 = LINE ( 'NONE', #6689, #10919 ) ;
#27624 = VECTOR ( 'NONE', #15390, 1000.000000000000000 ) ;
#27625 = CARTESIAN_POINT ( 'NONE',  ( 175.7287565553229456, -4.999999999999970690, 3.500000000000003109 ) ) ;
#27626 = CARTESIAN_POINT ( 'NONE',  ( 35.30103323675335503, -20.07235686745416103, -19.24079536022738068 ) ) ;
#27627 = VECTOR ( 'NONE', #12131, 1000.000000000000000 ) ;
#27628 = CARTESIAN_POINT ( 'NONE',  ( 10.68833914101186444, 8.961267084878116407, -16.40255713880337751 ) ) ;
#27629 = VERTEX_POINT ( 'NONE', #12115 ) ;
#27630 = VECTOR ( 'NONE', #8442, 1000.000000000000000 ) ;
#27631 = CARTESIAN_POINT ( 'NONE',  ( 29.30346499805017757, -7.722527705200430859, -14.56292402596598556 ) ) ;
#27632 = CARTESIAN_POINT ( 'NONE',  ( 137.0152310637605808, -4.999999999999980460, -1.521174642513229767E-14 ) ) ;
#27633 = CARTESIAN_POINT ( 'NONE',  ( 10.45680941692980959, 16.52194969480735764, -17.34528143170414083 ) ) ;
#27634 = CARTESIAN_POINT ( 'NONE',  ( 13.15390973649967599, 8.859676595473322536, -14.60899741038990562 ) ) ;
#27635 = CARTESIAN_POINT ( 'NONE',  ( 137.0152310637605524, -10.00000000000000533, -0.06116980274991495881 ) ) ;
#27636 = ORIENTED_EDGE ( 'NONE', *, *, #3640, .T. ) ;
#27637 = DIRECTION ( 'NONE',  ( 0.5877852522924731371, 1.586114251531760728E-16, 0.8090169943749474513 ) ) ;
#27638 = CARTESIAN_POINT ( 'NONE',  ( 12.50226005284522657, 8.571700941790735939, -15.12837371066060221 ) ) ;
#27639 = EDGE_LOOP ( 'NONE', ( #7271, #16430, #24416, #27838, #20320 ) ) ;
#27640 = VERTEX_POINT ( 'NONE', #4954 ) ;
#27641 = DIRECTION ( 'NONE',  ( 1.000000000000000000, 2.698458740408365879E-16, -1.110223024625156540E-16 ) ) ;
#27642 = ORIENTED_EDGE ( 'NONE', *, *, #26974, .T. ) ;
#27643 = CARTESIAN_POINT ( 'NONE',  ( 9.661930010240627809, 16.25461132122415364, -17.91197252329769185 ) ) ;
#27644 = CARTESIAN_POINT ( 'NONE',  ( 17.51795708650258732, -0.4494001013054305660, -15.13702969726144509 ) ) ;
#27645 = CARTESIAN_POINT ( 'NONE',  ( 24.91993355315554837, -1.627520125476753510, -17.55906114018776876 ) ) ;
#27646 = CARTESIAN_POINT ( 'NONE',  ( 21.65198393244800812, 4.573788442230395823, -17.29480057625502454 ) ) ;
#27647 = AXIS2_PLACEMENT_3D ( 'NONE', #24839, #1047, #10324 ) ;
#27648 = DIRECTION ( 'NONE',  ( 0.000000000000000000, -1.000000000000000000, -0.000000000000000000 ) ) ;
#27649 = DIRECTION ( 'NONE',  ( -0.8090169943749474513, -2.183098979609982436E-16, 0.5877852522924731371 ) ) ;
#27650 = EDGE_CURVE ( 'NONE', #20619, #3306, #21273, .T. ) ;
#27651 = EDGE_CURVE ( 'NONE', #5801, #21069, #26027, .T. ) ;
#27652 = AXIS2_PLACEMENT_3D ( 'NONE', #19859, #15272, #29070 ) ;
#27653 = EDGE_CURVE ( 'NONE', #22172, #11987, #5410, .T. ) ;
#27654 = CARTESIAN_POINT ( 'NONE',  ( 23.76365953361780470, 2.837943588559999508, -16.54419024451982168 ) ) ;
#27655 = APPLICATION_CONTEXT ( 'automotive_design' ) ;
#27656 = VECTOR ( 'NONE', #8770, 1000.000000000000000 ) ;
#27657 = LINE ( 'NONE', #18907, #21270 ) ;
#27658 = DIRECTION ( 'NONE',  ( -2.698458740408365879E-16, 1.000000000000000000, 0.000000000000000000 ) ) ;
#27659 = CARTESIAN_POINT ( 'NONE',  ( 10.45306510330410177, 16.53912159438435125, -17.34933906371858114 ) ) ;
#27660 = LINE ( 'NONE', #25191, #16476 ) ;
#27661 = CARTESIAN_POINT ( 'NONE',  ( 133.7287565553229456, -4.999999999999982236, 0.5000000000000029976 ) ) ;
#27662 = VERTEX_POINT ( 'NONE', #2671 ) ;
#27663 = ORIENTED_EDGE ( 'NONE', *, *, #12409, .F. ) ;
#27664 = DIRECTION ( 'NONE',  ( -0.9510565162951536422, 0.000000000000000000, -0.3090169943749472292 ) ) ;
#27665 = AXIS2_PLACEMENT_3D ( 'NONE', #2527, #19268, #25861 ) ;
#27666 = CARTESIAN_POINT ( 'NONE',  ( 15.22033579473957410, 7.355362781181614018, -19.64495939069069763 ) ) ;
#27667 = CARTESIAN_POINT ( 'NONE',  ( 11.60030688134799171, 15.19048121717941768, -16.65049206281727479 ) ) ;
#27668 = CARTESIAN_POINT ( 'NONE',  ( 34.54007435814109783, -17.65377171698271752, -20.05309729467257540 ) ) ;
#27669 = ORIENTED_EDGE ( 'NONE', *, *, #28327, .T. ) ;
#27670 = ORIENTED_EDGE ( 'NONE', *, *, #307, .T. ) ;
#27671 = ORIENTED_EDGE ( 'NONE', *, *, #15559, .T. ) ;
#27672 = AXIS2_PLACEMENT_3D ( 'NONE', #176, #5040, #23 ) ;
#27673 = CARTESIAN_POINT ( 'NONE',  ( 9.916775705961365261, 16.40575746196480011, -16.50441451066904364 ) ) ;
#27674 = VECTOR ( 'NONE', #17790, 1000.000000000000000 ) ;
#27675 = CARTESIAN_POINT ( 'NONE',  ( 12.76278909782508997, 7.628803627606831839, -14.92072746316176790 ) ) ;
#27676 = DIRECTION ( 'NONE',  ( -0.7071067811865481278, 0.7071067811865469066, 0.000000000000000000 ) ) ;
#27677 = DIRECTION ( 'NONE',  ( 1.000000000000000000, 2.698458740408365879E-16, -1.110223024625156540E-16 ) ) ;
#27678 = VERTEX_POINT ( 'NONE', #28641 ) ;
#27679 = FACE_OUTER_BOUND ( 'NONE', #28290, .T. ) ;
#27680 = ORIENTED_EDGE ( 'NONE', *, *, #5812, .F. ) ;
#27681 = CARTESIAN_POINT ( 'NONE',  ( 12.87265939729807762, 9.517981781931423413, -16.11192280467173532 ) ) ;
#27682 = AXIS2_PLACEMENT_3D ( 'NONE', #29413, #24625, #15603 ) ;
#27683 = CARTESIAN_POINT ( 'NONE',  ( 35.70376052765831787, -18.38912696963886617, -20.33459093173238941 ) ) ;
#27684 = CARTESIAN_POINT ( 'NONE',  ( 26.85315702054868936, -3.432285194908070380, -17.01323758698984889 ) ) ;
#27685 = ORIENTED_EDGE ( 'NONE', *, *, #23050, .F. ) ;
#27686 = ORIENTED_EDGE ( 'NONE', *, *, #24775, .T. ) ;
#27687 = PLANE ( 'NONE',  #4784 ) ;
#27688 = CARTESIAN_POINT ( 'NONE',  ( 149.7287565553229740, -10.00000000000000178, -7.839745962155603820 ) ) ;
#27689 = ORIENTED_EDGE ( 'NONE', *, *, #10346, .F. ) ;
#27690 = EDGE_CURVE ( 'NONE', #23715, #28996, #9970, .T. ) ;
#27691 = EDGE_CURVE ( 'NONE', #13196, #5499, #831, .T. ) ;
#27692 = CARTESIAN_POINT ( 'NONE',  ( 18.51435942584036454, 8.743714487506315081, -19.56092670885941587 ) ) ;
#27693 = ADVANCED_FACE ( 'NONE', ( #19283 ), #14696, .T. ) ;
#27694 = CARTESIAN_POINT ( 'NONE',  ( 20.69116929084294298, -5.269815114589342819, -18.46063674707264468 ) ) ;
#27695 = CIRCLE ( 'NONE', #16426, 40.00000000000000711 ) ;
#27696 = EDGE_CURVE ( 'NONE', #288, #16032, #10121, .T. ) ;
#27697 = ORIENTED_EDGE ( 'NONE', *, *, #13347, .T. ) ;
#27698 = FACE_OUTER_BOUND ( 'NONE', #21540, .T. ) ;
#27699 = VECTOR ( 'NONE', #4636, 1000.000000000000000 ) ;
#27700 = CARTESIAN_POINT ( 'NONE',  ( -2.000000000000008882, 3.464101615137750390, 0.000000000000000000 ) ) ;
#27701 = AXIS2_PLACEMENT_3D ( 'NONE', #6756, #30165, #4312 ) ;
#27702 = DIRECTION ( 'NONE',  ( -0.5877852522924731371, -1.586114251531760235E-16, 0.8090169943749474513 ) ) ;
#27703 = DIRECTION ( 'NONE',  ( -1.000000000000000000, 0.000000000000000000, 0.000000000000000000 ) ) ;
#27704 = CARTESIAN_POINT ( 'NONE',  ( 10.72892505862787971, 16.59389366189031634, -15.95083598634710320 ) ) ;
#27705 = CARTESIAN_POINT ( 'NONE',  ( 26.64416741123070054, -12.70369174447049332, -17.39020166599120643 ) ) ;
#27706 = VERTEX_POINT ( 'NONE', #14841 ) ;
#27707 = CARTESIAN_POINT ( 'NONE',  ( 157.0152310637605808, -9.999999999999998224, -32.93883019725009120 ) ) ;
#27708 = ORIENTED_EDGE ( 'NONE', *, *, #21164, .T. ) ;
#27709 = CARTESIAN_POINT ( 'NONE',  ( 9.695397291186985456, 17.42102709130404747, -17.08803885907851594 ) ) ;
#27710 = AXIS2_PLACEMENT_3D ( 'NONE', #29131, #10308, #1480 ) ;
#27711 = CARTESIAN_POINT ( 'NONE',  ( 18.48188012193690710, 6.385789046977964567, -18.71539758422269628 ) ) ;
#27712 = LINE ( 'NONE', #57, #14622 ) ;
#27713 = DIRECTION ( 'NONE',  ( 0.000000000000000000, -2.775557561562890735E-17, 1.000000000000000000 ) ) ;
#27715 = ORIENTED_EDGE ( 'NONE', *, *, #14200, .T. ) ;
#27714 = CARTESIAN_POINT ( 'NONE',  ( 26.48263329513011755, -12.06126822337667903, -13.95730679897583038 ) ) ;
#27716 = VERTEX_POINT ( 'NONE', #16551 ) ;
#27717 = CARTESIAN_POINT ( 'NONE',  ( 89.30687414754424935, -4.999999999999992895, 64.88524211141340459 ) ) ;
#27718 = CARTESIAN_POINT ( 'NONE',  ( 12.29957980484737767, 9.540162674316999158, -15.28991344586433421 ) ) ;
#27719 = AXIS2_PLACEMENT_3D ( 'NONE', #15738, #25064, #4152 ) ;
#27720 = CARTESIAN_POINT ( 'NONE',  ( 33.44337896868773186, -12.72690026786775341, -19.72159258799634074 ) ) ;
#27721 = CARTESIAN_POINT ( 'NONE',  ( 14.39533340154967433, 6.572929804808670617, -18.54476805420031837 ) ) ;
#27722 = DIRECTION ( 'NONE',  ( 0.000000000000000000, 0.000000000000000000, 1.000000000000000000 ) ) ;
#27723 = CARTESIAN_POINT ( 'NONE',  ( 21.76348650023563636, -1.483442554740824537, -14.70963264896640155 ) ) ;
#27724 = ORIENTED_EDGE ( 'NONE', *, *, #19578, .T. ) ;
#27725 = CARTESIAN_POINT ( 'NONE',  ( 132.0152310637605808, -10.00000000000000711, -32.93883019725009120 ) ) ;
#27726 =( NAMED_UNIT ( * ) PLANE_ANGLE_UNIT ( ) SI_UNIT ( $, .RADIAN. ) );
#27727 = VECTOR ( 'NONE', #25672, 1000.000000000000000 ) ;
#27728 = CARTESIAN_POINT ( 'NONE',  ( 14.06424326207706699, 5.752694757912038881, -19.02294901845717945 ) ) ;
#27729 = CARTESIAN_POINT ( 'NONE',  ( 25.37029659992048281, -10.87484012800900501, -14.78472363349550811 ) ) ;
#27730 = EDGE_CURVE ( 'NONE', #11670, #2626, #2539, .T. ) ;
#27731 = EDGE_CURVE ( 'NONE', #2212, #5854, #14243, .T. ) ;
#27732 = EDGE_CURVE ( 'NONE', #28465, #16324, #14390, .T. ) ;
#27733 = ORIENTED_EDGE ( 'NONE', *, *, #1837, .F. ) ;
#27734 = DIRECTION ( 'NONE',  ( -2.698458740408365879E-16, 1.000000000000000000, 0.000000000000000000 ) ) ;
#27735 = VECTOR ( 'NONE', #11038, 1000.000000000000000 ) ;
#27736 = LINE ( 'NONE', #14087, #13317 ) ;
#27737 = PLANE ( 'NONE',  #6147 ) ;
#27738 = VECTOR ( 'NONE', #15706, 1000.000000000000000 ) ;
#27739 = LINE ( 'NONE', #8474, #29701 ) ;
#27740 = PLANE ( 'NONE',  #14804 ) ;
#27741 = CARTESIAN_POINT ( 'NONE',  ( 172.7287565553229456, -9.999999999999980460, -41.50000000000000711 ) ) ;
#27742 = AXIS2_PLACEMENT_3D ( 'NONE', #16611, #25932, #5014 ) ;
#27743 = CARTESIAN_POINT ( 'NONE',  ( 25.74978097135661770, 0.6894738977563982241, -15.43585696046938160 ) ) ;
#27744 = CARTESIAN_POINT ( 'NONE',  ( 13.98191416104776685, 5.331502061239655532, -16.22335970869868760 ) ) ;
#27745 = CARTESIAN_POINT ( 'NONE',  ( 34.31408884023914396, -17.63853849290766362, -21.02710884213126263 ) ) ;
#27746 = SURFACE_STYLE_USAGE ( .BOTH. , #9216 ) ;
#27747 = CARTESIAN_POINT ( 'NONE',  ( 11.47748818427356987, 9.248962635895034978, -15.85894168489154765 ) ) ;
#27748 = CARTESIAN_POINT ( 'NONE',  ( 36.04859390953723874, -22.18451583373416014, -15.00000000000000000 ) ) ;
#27749 = CARTESIAN_POINT ( 'NONE',  ( 138.6922820468854525, -10.00000000000000533, -32.39392330124607611 ) ) ;
#27750 = CARTESIAN_POINT ( 'NONE',  ( 9.667846996725693032, 16.22747526696303666, -17.88508502774671882 ) ) ;
#27751 = CARTESIAN_POINT ( 'NONE',  ( -3.318518101603040726, -7.321656987762888313, -4.999999999999986677 ) ) ;
#27752 = ORIENTED_EDGE ( 'NONE', *, *, #18176, .F. ) ;
#27753 = CARTESIAN_POINT ( 'NONE',  ( 25.62901471571457890, -5.000000000000010658, -78.87799666457712533 ) ) ;
#27754 = CARTESIAN_POINT ( 'NONE',  ( 12.48799528366842360, 8.565546312597838607, -15.13973160209665991 ) ) ;
#27755 = ORIENTED_EDGE ( 'NONE', *, *, #819, .F. ) ;
#27756 = DIRECTION ( 'NONE',  ( -0.9510565162951536422, -2.566386769018988816E-16, -0.3090169943749472292 ) ) ;
#27757 = LINE ( 'NONE', #15957, #24433 ) ;
#27758 = DIRECTION ( 'NONE',  ( -0.8090169943749474513, -2.183098979609982436E-16, -0.5877852522924731371 ) ) ;
#27759 = ORIENTED_EDGE ( 'NONE', *, *, #27045, .F. ) ;
#27760 = CARTESIAN_POINT ( 'NONE',  ( 9.101278670497288559, 16.23297416207913813, -17.06093009358445300 ) ) ;
#27761 = CARTESIAN_POINT ( 'NONE',  ( 35.54317590287104167, -23.16017559978188345, -18.72806989825276247 ) ) ;
#27762 = VECTOR ( 'NONE', #17151, 1000.000000000000000 ) ;
#27763 = CARTESIAN_POINT ( 'NONE',  ( 20.51677437365689372, 7.544110930723523012, -19.48516728630390915 ) ) ;
#27764 = EDGE_CURVE ( 'NONE', #13474, #1407, #679, .T. ) ;
#27765 = CARTESIAN_POINT ( 'NONE',  ( 19.16431125762126442, 9.782083453288988650, -17.54400000489614087 ) ) ;
#27766 = EDGE_CURVE ( 'NONE', #18100, #19125, #24037, .T. ) ;
#27767 = EDGE_CURVE ( 'NONE', #4943, #8020, #23732, .T. ) ;
#27768 = CIRCLE ( 'NONE', #14548, 0.4999999999999986677 ) ;
#27769 = CARTESIAN_POINT ( 'NONE',  ( 114.8169341242263215, -4.999999999999985789, -83.41938557644036223 ) ) ;
#27770 = ADVANCED_FACE ( 'NONE', ( #7404 ), #14545, .T. ) ;
#27771 = CARTESIAN_POINT ( 'NONE',  ( 22.91777464530744268, -8.256078323855359002, -14.14386909076557686 ) ) ;
#27772 = VERTEX_POINT ( 'NONE', #21583 ) ;
#27773 = FACE_OUTER_BOUND ( 'NONE', #6395, .T. ) ;
#27775 = ORIENTED_EDGE ( 'NONE', *, *, #22974, .F. ) ;
#27774 = CARTESIAN_POINT ( 'NONE',  ( -4.000000000000020428, -6.928203230275511437, 0.000000000000000000 ) ) ;
#27776 = ORIENTED_EDGE ( 'NONE', *, *, #9472, .F. ) ;
#27777 = DIRECTION ( 'NONE',  ( -2.698458740408365879E-16, 1.000000000000000000, 0.000000000000000000 ) ) ;
#27778 = CYLINDRICAL_SURFACE ( 'NONE', #17543, 4.000000000000003553 ) ;
#27779 = CARTESIAN_POINT ( 'NONE',  ( 35.44226431226860541, -20.70683327756191616, -19.15799893943290755 ) ) ;
#27780 = VECTOR ( 'NONE', #990, 1000.000000000000000 ) ;
#27781 = CARTESIAN_POINT ( 'NONE',  ( 11.38288633050183307, 7.831121701799675705, -15.95859485361821939 ) ) ;
#27782 = ORIENTED_EDGE ( 'NONE', *, *, #11404, .T. ) ;
#27783 = CARTESIAN_POINT ( 'NONE',  ( 0.000000000000000000, 0.000000000000000000, -5.000000000000000888 ) ) ;
#27784 = FACE_OUTER_BOUND ( 'NONE', #6398, .T. ) ;
#27785 = B_SPLINE_CURVE_WITH_KNOTS ( 'NONE', 3,
 ( #20532, #22992, #6509, #13366, #27751, #13668 ),
 .UNSPECIFIED., .F., .F.,
 ( 4, 2, 4 ),
 ( 2.380731630115636932E-07, 0.002336973833157603240, 0.004673709593152193878 ),
 .UNSPECIFIED. ) ;
#27786 = CARTESIAN_POINT ( 'NONE',  ( 10.47401950373780899, 16.44302204293020964, -17.33397781699859053 ) ) ;
#27787 = DIRECTION ( 'NONE',  ( -2.698458740408365879E-16, 1.000000000000000000, 0.000000000000000000 ) ) ;
#27788 = VECTOR ( 'NONE', #14425, 1000.000000000000000 ) ;
#27789 = CARTESIAN_POINT ( 'NONE',  ( 129.5152310637605524, -10.00000000000000888, -4.391296821672111328 ) ) ;
#27790 = EDGE_LOOP ( 'NONE', ( #28934, #22783, #2520, #24689, #2127, #10116 ) ) ;
#27791 = ORIENTED_EDGE ( 'NONE', *, *, #3005, .F. ) ;
#27792 = DIRECTION ( 'NONE',  ( 1.110223024625156540E-16, 2.995891024602366092E-32, 1.000000000000000000 ) ) ;
#27793 = CARTESIAN_POINT ( 'NONE',  ( -2.500000000000002665, -8.040613248383180784E-16, 19.04999999999997229 ) ) ;
#27794 = EDGE_LOOP ( 'NONE', ( #9149, #25443, #5229, #24277 ) ) ;
#27795 = DIRECTION ( 'NONE',  ( -2.698458740408365879E-16, 1.000000000000000000, 0.000000000000000000 ) ) ;
#27796 = ORIENTED_EDGE ( 'NONE', *, *, #5158, .T. ) ;
#27797 = CARTESIAN_POINT ( 'NONE',  ( 9.684081875198721434, 16.15302004482010645, -17.87837111813898616 ) ) ;
#27798 = CARTESIAN_POINT ( 'NONE',  ( 17.49129197179432538, 0.06586305242593921971, -19.15772692538415356 ) ) ;
#27799 = CARTESIAN_POINT ( 'NONE',  ( 22.28228072301589080, -4.238876526682920698, -17.70252831752424427 ) ) ;
#27800 = CARTESIAN_POINT ( 'NONE',  ( 22.98323032518889519, 2.094654362561221284, -17.51695658672324640 ) ) ;
#27801 = CARTESIAN_POINT ( 'NONE',  ( 138.6922820468854241, -10.00000000000000533, -0.6060766987539614181 ) ) ;
#27802 = CARTESIAN_POINT ( 'NONE',  ( 133.6922820468854241, -1.999999999999981348, -9.266330736598357376 ) ) ;
#27803 = EDGE_CURVE ( 'NONE', #4596, #15139, #7435, .T. ) ;
#27804 = CARTESIAN_POINT ( 'NONE',  ( 8.930358392086997554, -5.000000000000015099, 27.48481700440100184 ) ) ;
#27805 = ADVANCED_FACE ( 'NONE', ( #3573 ), #24782, .T. ) ;
#27806 = VECTOR ( 'NONE', #14171, 1000.000000000000114 ) ;
#27807 = CARTESIAN_POINT ( 'NONE',  ( 27.83100014064079275, -5.545984359997562230, -15.13782040115233052 ) ) ;
#27808 = AXIS2_PLACEMENT_3D ( 'NONE', #3613, #873, #3463 ) ;
#27809 = SURFACE_SIDE_STYLE ('',( #13863 ) ) ;
#27810 = LINE ( 'NONE', #13722, #8406 ) ;
#27811 = LINE ( 'NONE', #8279, #21881 ) ;
#27812 = DIRECTION ( 'NONE',  ( -2.698458740408365879E-16, 1.000000000000000000, 0.000000000000000000 ) ) ;
#27813 = DIRECTION ( 'NONE',  ( 0.5877852522924731371, 1.586114251531760728E-16, -0.8090169943749474513 ) ) ;
#27814 = CARTESIAN_POINT ( 'NONE',  ( 10.41412541532089620, 16.71770396712979689, -17.42473314453425814 ) ) ;
#27815 = DIRECTION ( 'NONE',  ( 1.000000000000000000, 4.440892098500622217E-16, 0.000000000000000000 ) ) ;
#27816 = PLANE ( 'NONE',  #28291 ) ;
#27817 = ORIENTED_EDGE ( 'NONE', *, *, #14652, .F. ) ;
#27818 = ORIENTED_EDGE ( 'NONE', *, *, #12725, .F. ) ;
#27819 = LINE ( 'NONE', #9139, #23170 ) ;
#27820 = CARTESIAN_POINT ( 'NONE',  ( 14.73401617531889229, 6.408058468588501810, -15.60580005407095960 ) ) ;
#27821 = CARTESIAN_POINT ( 'NONE',  ( 11.05541802266494855, 17.68941098027438841, -17.91029082024824959 ) ) ;
#27822 = CARTESIAN_POINT ( 'NONE',  ( 33.96943610671532809, -15.09019632882451134, -19.88060704079178720 ) ) ;
#27823 = PRODUCT_DEFINITION_FORMATION_WITH_SPECIFIED_SOURCE ( 'ANY', '', #1575, .NOT_KNOWN. ) ;
#27824 = EDGE_CURVE ( 'NONE', #18145, #10339, #12864, .T. ) ;
#27825 = AXIS2_PLACEMENT_3D ( 'NONE', #1186, #28687, #17492 ) ;
#27826 = ORIENTED_EDGE ( 'NONE', *, *, #13137, .F. ) ;
#27827 = CARTESIAN_POINT ( 'NONE',  ( 9.695397291186985456, 17.42102709130404747, -17.08803885907851594 ) ) ;
#27828 = VECTOR ( 'NONE', #14239, 999.9999999999998863 ) ;
#27829 = CARTESIAN_POINT ( 'NONE',  ( 12.75399582221978889, 7.624919616107145970, -14.92773571455457216 ) ) ;
#27830 = FACE_OUTER_BOUND ( 'NONE', #19457, .T. ) ;
#27831 = CARTESIAN_POINT ( 'NONE',  ( 147.0152310637605524, -10.00000000000000178, -17.38167787843871182 ) ) ;
#27832 = ORIENTED_EDGE ( 'NONE', *, *, #24740, .F. ) ;
#27833 = VECTOR ( 'NONE', #7730, 1000.000000000000000 ) ;
#27834 = ORIENTED_EDGE ( 'NONE', *, *, #25148, .T. ) ;
#27835 = FACE_OUTER_BOUND ( 'NONE', #113, .T. ) ;
#27836 = ORIENTED_EDGE ( 'NONE', *, *, #9629, .F. ) ;
#27837 = CARTESIAN_POINT ( 'NONE',  ( 10.99070134719017311, 14.07345324724201063, -17.12031169937328201 ) ) ;
#27838 = ORIENTED_EDGE ( 'NONE', *, *, #14059, .T. ) ;
#27839 = CARTESIAN_POINT ( 'NONE',  ( 33.24108837279852224, -10.36619216719171632, -17.82210672427467912 ) ) ;
#27840 = CARTESIAN_POINT ( 'NONE',  ( 23.60870351872479844, -7.222488552757559077, -14.83554404960226947 ) ) ;
#27841 = VERTEX_POINT ( 'NONE', #22334 ) ;
#27842 = DIRECTION ( 'NONE',  ( -1.000000000000000000, 0.000000000000000000, 0.000000000000000000 ) ) ;
#27843 = EDGE_LOOP ( 'NONE', ( #14820, #18924, #1261, #5890, #24233 ) ) ;
#27844 = DIRECTION ( 'NONE',  ( 0.5877852522924731371, 1.586114251531760728E-16, -0.8090169943749474513 ) ) ;
#27845 = VECTOR ( 'NONE', #4112, 1000.000000000000000 ) ;
#27846 = CARTESIAN_POINT ( 'NONE',  ( 14.70507544977879100, 5.024503852999842479, -17.88552553980999704 ) ) ;
#27847 = VECTOR ( 'NONE', #2652, 1000.000000000000000 ) ;
#27848 = CARTESIAN_POINT ( 'NONE',  ( 27.00045552667489446, -4.635344809676953837, -19.07524480842047510 ) ) ;
#27849 = ORIENTED_EDGE ( 'NONE', *, *, #1667, .T. ) ;
#27850 = CARTESIAN_POINT ( 'NONE',  ( 129.5152310637605808, -1.999999999999982236, -11.28819510263909187 ) ) ;
#27851 = AXIS2_PLACEMENT_3D ( 'NONE', #4869, #14166, #2601 ) ;
#27852 = LINE ( 'NONE', #6913, #23797 ) ;
#27853 = CARTESIAN_POINT ( 'NONE',  ( 153.6922820468854241, -4.999999999999976907, -26.58683881228715862 ) ) ;
#27854 = CARTESIAN_POINT ( 'NONE',  ( 157.0152310637605524, -9.999999999999998224, -34.70218595412750773 ) ) ;
#27855 = PRODUCT_DEFINITION_CONTEXT ( 'detailed design', #19802, 'design' ) ;
#27856 = CARTESIAN_POINT ( 'NONE',  ( 10.48326151898216452, 17.72053796952357985, -16.40639007392780258 ) ) ;
#27858 = AXIS2_PLACEMENT_3D ( 'NONE', #21785, #3778, #5920 ) ;
#27857 = DIRECTION ( 'NONE',  ( 1.000000000000000000, 0.000000000000000000, 0.000000000000000000 ) ) ;
#27859 = ADVANCED_FACE ( 'NONE', ( #13019 ), #20041, .T. ) ;
#27860 = EDGE_CURVE ( 'NONE', #16811, #1407, #17736, .T. ) ;
#27861 = ORIENTED_EDGE ( 'NONE', *, *, #3570, .T. ) ;
#27862 = CARTESIAN_POINT ( 'NONE',  ( 156.1922820468853956, -4.999999999999975131, -19.40354224447947828 ) ) ;
#27863 = VERTEX_POINT ( 'NONE', #8136 ) ;
#27864 = VECTOR ( 'NONE', #7745, 1000.000000000000000 ) ;
#27865 = CARTESIAN_POINT ( 'NONE',  ( 11.47231678315799464, 9.271847796573304379, -15.86114366194887815 ) ) ;
#27867 = ADVANCED_FACE ( 'NONE', ( #13168 ), #19728, .T. ) ;
#27866 = AXIS2_PLACEMENT_3D ( 'NONE', #2055, #11335, #20194 ) ;
#27868 = CARTESIAN_POINT ( 'NONE',  ( 18.99253871878172717, 7.061292173911923875, -17.66947577672478431 ) ) ;
#27869 = CARTESIAN_POINT ( 'NONE',  ( 14.89669440878228635, -5.000000000000013323, 45.84731114023986720 ) ) ;
#27870 = LINE ( 'NONE', #22651, #11148 ) ;
#27871 = EDGE_CURVE ( 'NONE', #6983, #27422, #1286, .T. ) ;
#27873 = VERTEX_POINT ( 'NONE', #27097 ) ;
#27872 = CARTESIAN_POINT ( 'NONE',  ( 29.30346499805017757, -7.722527705200430859, -14.56292402596598556 ) ) ;
#27874 = ORIENTED_EDGE ( 'NONE', *, *, #17587, .F. ) ;
#27875 = CARTESIAN_POINT ( 'NONE',  ( 3.999999999999980904, -2.309401076758567317, -2.092734410091829034 ) ) ;
#27876 = CARTESIAN_POINT ( 'NONE',  ( 11.27624053946810889, 16.67669076989127674, -16.78450489582619554 ) ) ;
#27877 = CARTESIAN_POINT ( 'NONE',  ( 35.24964364652129234, -20.84149066036063047, -20.16262864730545346 ) ) ;
#27878 = DIRECTION ( 'NONE',  ( 0.000000000000000000, -0.5000000000000012212, -0.8660254037844380415 ) ) ;
#27879 = PLANE ( 'NONE',  #10594 ) ;
#27880 = CARTESIAN_POINT ( 'NONE',  ( 21.93691487550926311, -3.207747311472892271, -17.94368141530714311 ) ) ;
#27881 = ORIENTED_EDGE ( 'NONE', *, *, #15125, .T. ) ;
#27882 = PLANE ( 'NONE',  #13483 ) ;
#27883 = ORIENTED_EDGE ( 'NONE', *, *, #27618, .F. ) ;
#27884 = CARTESIAN_POINT ( 'NONE',  ( 20.51209521231993094, 3.083376493849706801, -19.38174501956431683 ) ) ;
#27885 = CARTESIAN_POINT ( 'NONE',  ( 29.44447141382201139, -6.373630389881236091, -17.32815070419105297 ) ) ;
#27886 = VERTEX_POINT ( 'NONE', #29247 ) ;
#27887 = VECTOR ( 'NONE', #14734, 1000.000000000000000 ) ;
#27888 = CARTESIAN_POINT ( 'NONE',  ( 151.1922820468853956, -10.00000000000000178, -13.59645775552055902 ) ) ;
#27889 = AXIS2_PLACEMENT_3D ( 'NONE', #7563, #16865, #9987 ) ;
#27890 = LINE ( 'NONE', #11805, #12837 ) ;
#27891 = DIRECTION ( 'NONE',  ( 1.000000000000000000, 0.000000000000000000, 0.000000000000000000 ) ) ;
#27892 = LINE ( 'NONE', #13795, #3658 ) ;
#27893 = CARTESIAN_POINT ( 'NONE',  ( 9.641350777746193756, 17.66889129127197577, -17.91630266473768884 ) ) ;
#27894 = CARTESIAN_POINT ( 'NONE',  ( 26.42757832573366983, -5.232593867482060013, -19.46531670327460617 ) ) ;
#27895 = CARTESIAN_POINT ( 'NONE',  ( 20.13607245741800611, 4.456688099076253629, -14.49627829575511129 ) ) ;
#27896 = EDGE_CURVE ( 'NONE', #3964, #7930, #1593, .T. ) ;
#27897 = CARTESIAN_POINT ( 'NONE',  ( 33.02439791605519304, -11.93986616049457261, -20.58189241239533374 ) ) ;
#27898 = DIRECTION ( 'NONE',  ( 0.000000000000000000, 2.775557561562890735E-17, -1.000000000000000000 ) ) ;
#27899 = LINE ( 'NONE', #16558, #8218 ) ;
#27900 = EDGE_CURVE ( 'NONE', #9938, #19629, #10871, .T. ) ;
#27901 = ADVANCED_FACE ( 'NONE', ( #27258 ), #26949, .T. ) ;
#27902 = CARTESIAN_POINT ( 'NONE',  ( 2.500000000000000444, -2.357898499370430834, 3.469446951953614189E-15 ) ) ;
#27903 = DIRECTION ( 'NONE',  ( -0.8090169943749474513, -2.183098979609982436E-16, -0.5877852522924731371 ) ) ;
#27904 = ADVANCED_FACE ( 'NONE', ( #6006 ), #15293, .T. ) ;
#27905 = CARTESIAN_POINT ( 'NONE',  ( 16.79143122783437292, 7.330551994622505063, -14.54187356113185103 ) ) ;
#27906 = ORIENTED_EDGE ( 'NONE', *, *, #15331, .F. ) ;
#27907 = LINE ( 'NONE', #22995, #8085 ) ;
#27908 = CARTESIAN_POINT ( 'NONE',  ( 12.49428694376680049, 8.568214790255201052, -15.13472557389765072 ) ) ;
#27909 = ORIENTED_EDGE ( 'NONE', *, *, #8951, .T. ) ;
#27910 = FACE_OUTER_BOUND ( 'NONE', #27988, .T. ) ;
#27911 = CARTESIAN_POINT ( 'NONE',  ( 166.1922820468853672, -1.999999999999972244, -28.06379628232387446 ) ) ;
#27912 = CARTESIAN_POINT ( 'NONE',  ( 17.08157517049449581, 7.460725202527481947, -14.57009041681831896 ) ) ;
#27913 = EDGE_LOOP ( 'NONE', ( #868, #5535, #16067, #22986 ) ) ;
#27914 = ORIENTED_EDGE ( 'NONE', *, *, #11210, .T. ) ;
#27915 = CARTESIAN_POINT ( 'NONE',  ( 35.54859390953724585, -23.18451583373416014, -17.64281456791166391 ) ) ;
#27916 = CARTESIAN_POINT ( 'NONE',  ( 21.93691487550926311, -3.207747311472892271, -17.94368141530714311 ) ) ;
#27917 = CARTESIAN_POINT ( 'NONE',  ( 17.81745789538532776, 7.988559130291253751, -20.18242036267038841 ) ) ;
#27918 = CARTESIAN_POINT ( 'NONE',  ( 25.20714760837546464, -2.665945389627573991, -12.53535894516201665 ) ) ;
#27919 = VECTOR ( 'NONE', #16005, 1000.000000000000000 ) ;
#27920 = VERTEX_POINT ( 'NONE', #24178 ) ;
#27921 = FACE_OUTER_BOUND ( 'NONE', #1968, .T. ) ;
#27923 = ORIENTED_EDGE ( 'NONE', *, *, #15202, .T. ) ;
#27922 = CARTESIAN_POINT ( 'NONE',  ( 147.0152310637604955, -10.00000000000000355, -0.06116980274991495881 ) ) ;
#27924 = ORIENTED_EDGE ( 'NONE', *, *, #1203, .F. ) ;
#27925 = LINE ( 'NONE', #18268, #22142 ) ;
#27926 = LINE ( 'NONE', #27625, #11678 ) ;
#27927 = CARTESIAN_POINT ( 'NONE',  ( 32.35289370704636980, -10.23129387835982129, -15.31177623828282108 ) ) ;
#27928 = CARTESIAN_POINT ( 'NONE',  ( 11.68234546060339163, 7.643720436761259229, -15.74430661255668262 ) ) ;
#27929 = VERTEX_POINT ( 'NONE', #3285 ) ;
#27930 = EDGE_CURVE ( 'NONE', #23167, #21077, #12559, .T. ) ;
#27931 = VECTOR ( 'NONE', #5211, 1000.000000000000000 ) ;
#27932 = ADVANCED_FACE ( 'NONE', ( #19582 ), #4838, .T. ) ;
#27933 = LINE ( 'NONE', #9708, #17076 ) ;
#27934 = DIRECTION ( 'NONE',  ( 1.110223024625156540E-16, 2.995891024602366092E-32, 1.000000000000000000 ) ) ;
#27935 = EDGE_CURVE ( 'NONE', #24083, #7486, #14994, .T. ) ;
#27936 = CARTESIAN_POINT ( 'NONE',  ( 10.47169460192958645, 16.45368433897878191, -17.33494088278173351 ) ) ;
#27937 = DIRECTION ( 'NONE',  ( -2.908569913943826047E-16, 1.000000000000000000, 6.826925868028084813E-18 ) ) ;
#27938 = EDGE_CURVE ( 'NONE', #29492, #3816, #1139, .T. ) ;
#27939 = DIRECTION ( 'NONE',  ( 0.3090169943749472292, 8.338696094057992503E-17, -0.9510565162951536422 ) ) ;
#27940 = EDGE_LOOP ( 'NONE', ( #12658, #6589, #15802, #25472, #4757 ) ) ;
#27941 = CARTESIAN_POINT ( 'NONE',  ( 142.0152310637605240, -1.999999999999978684, -0.06116980274991495881 ) ) ;
#27942 = CARTESIAN_POINT ( 'NONE',  ( 1.214306433183764966E-14, 4.618802153517016507, -0.3572655899081716435 ) ) ;
#27944 = ORIENTED_EDGE ( 'NONE', *, *, #19721, .F. ) ;
#27943 = VECTOR ( 'NONE', #9237, 1000.000000000000000 ) ;
#27945 = ORIENTED_EDGE ( 'NONE', *, *, #62, .T. ) ;
#27946 = CARTESIAN_POINT ( 'NONE',  ( 100.5683542740252960, -4.999999999999990230, -73.06718635158908626 ) ) ;
#27947 = ORIENTED_EDGE ( 'NONE', *, *, #27487, .F. ) ;
#27948 = CARTESIAN_POINT ( 'NONE',  ( 9.664814466656260095, 16.24138283641780944, -17.88982567228806175 ) ) ;
#27949 = CARTESIAN_POINT ( 'NONE',  ( 19.32227194923075331, 0.3423946635036635433, -13.32047942220886583 ) ) ;
#27950 = CARTESIAN_POINT ( 'NONE',  ( 22.18457322443145330, -2.050108300791262828, -13.94172724511641448 ) ) ;
#27951 = CARTESIAN_POINT ( 'NONE',  ( 21.84445237452005628, 0.7298858868756038509, -19.18266460542251295 ) ) ;
#27952 = LINE ( 'NONE', #7009, #20866 ) ;
#27953 = LINE ( 'NONE', #27802, #912 ) ;
#27954 = CARTESIAN_POINT ( 'NONE',  ( 120.0000000000000000, -19.99999999999999645, -15.00000000000000000 ) ) ;
#27955 = CARTESIAN_POINT ( 'NONE',  ( 22.90372073960079646, -4.505259139820817715, -13.75793632099288111 ) ) ;
#27956 = ORIENTED_EDGE ( 'NONE', *, *, #23952, .T. ) ;
#27957 = CARTESIAN_POINT ( 'NONE',  ( 3.999999999999980904, -2.309401076758567317, -0.3572655899081716435 ) ) ;
#27958 = CARTESIAN_POINT ( 'NONE',  ( 162.0152310637605240, -9.999999999999998224, -34.70218595412750773 ) ) ;
#27959 = CARTESIAN_POINT ( 'NONE',  ( 152.0152310637606092, -10.00000000000000000, -32.93883019725009120 ) ) ;
#27960 = CARTESIAN_POINT ( 'NONE',  ( 169.7287565553229456, -9.999999999999996447, -25.16025403784440329 ) ) ;
#27961 = AXIS2_PLACEMENT_3D ( 'NONE', #21008, #11533, #25301 ) ;
#27962 = CARTESIAN_POINT ( 'NONE',  ( 10.35864918915110877, 16.97212501191939538, -17.93331994345748370 ) ) ;
#27963 = DIRECTION ( 'NONE',  ( -0.9510565162951536422, -2.566386769018988323E-16, 0.3090169943749475623 ) ) ;
#27964 = ORIENTED_EDGE ( 'NONE', *, *, #11286, .T. ) ;
#27965 = CARTESIAN_POINT ( 'NONE',  ( 11.22273001195053155, 9.096583557657577757, -17.24208598844832352 ) ) ;
#27966 = VERTEX_POINT ( 'NONE', #8727 ) ;
#27967 = EDGE_CURVE ( 'NONE', #2772, #20312, #29871, .T. ) ;
#27968 = DIRECTION ( 'NONE',  ( 0.000000000000000000, -0.5000000000000011102, -0.8660254037844379305 ) ) ;
#27969 = CARTESIAN_POINT ( 'NONE',  ( 21.10023079691774228, -0.4353598523292347422, -20.14113737667230097 ) ) ;
#27970 = EDGE_CURVE ( 'NONE', #8103, #25602, #3872, .T. ) ;
#27971 = CARTESIAN_POINT ( 'NONE',  ( 11.29232397858413250, 16.60293006794363535, -16.77785382704750461 ) ) ;
#27972 = CARTESIAN_POINT ( 'NONE',  ( 35.54859390953724585, -22.18451583373416014, -18.19919658220850778 ) ) ;
#27973 = EDGE_CURVE ( 'NONE', #12642, #26976, #13905, .T. ) ;
#27974 = ORIENTED_EDGE ( 'NONE', *, *, #10654, .F. ) ;
#27975 = ORIENTED_EDGE ( 'NONE', *, *, #489, .F. ) ;
#27976 = CARTESIAN_POINT ( 'NONE',  ( 9.910898653440767703, 16.43271037397421708, -16.50709950392603531 ) ) ;
#27977 = CARTESIAN_POINT ( 'NONE',  ( 166.1922820468853672, -9.999999999999998224, -22.25671179336496053 ) ) ;
#27978 = CARTESIAN_POINT ( 'NONE',  ( 9.641350777746193756, 17.66889129127197577, -17.91630266473768884 ) ) ;
#27979 = CARTESIAN_POINT ( 'NONE',  ( 154.5152310637605524, -10.00000000000000000, -19.94844914048349693 ) ) ;
#27980 = CARTESIAN_POINT ( 'NONE',  ( 132.0152310637605524, -10.00000000000000711, -17.38167787843870826 ) ) ;
#27981 = ORIENTED_EDGE ( 'NONE', *, *, #14357, .T. ) ;
#27982 = CARTESIAN_POINT ( 'NONE',  ( 5.355005115540903304, 6.145890662064663168, -4.917753204360280961 ) ) ;
#27983 = ORIENTED_EDGE ( 'NONE', *, *, #28618, .T. ) ;
#27984 = CARTESIAN_POINT ( 'NONE',  ( 10.46247360472336041, 16.49597300757040230, -17.34042816522791952 ) ) ;
#27985 = ORIENTED_EDGE ( 'NONE', *, *, #28212, .F. ) ;
#27986 = CARTESIAN_POINT ( 'NONE',  ( 35.98907965336992731, -19.67091466371804742, -20.42083605867238205 ) ) ;
#27987 = CARTESIAN_POINT ( 'NONE',  ( 27.20760296572909809, -8.488227175050779394, -13.35743234967312354 ) ) ;
#27988 = EDGE_LOOP ( 'NONE', ( #16468, #14265, #29528, #23683 ) ) ;
#27989 = DIRECTION ( 'NONE',  ( -0.8090169943749474513, -2.183098979609982436E-16, 0.5877852522924731371 ) ) ;
#27990 = VECTOR ( 'NONE', #1137, 1000.000000000000000 ) ;
#27991 = CARTESIAN_POINT ( 'NONE',  ( 3.999999999999999112, 1.935983797701081643, -0.2494693066162320116 ) ) ;
#27992 = DIRECTION ( 'NONE',  ( 1.000000000000000000, 0.000000000000000000, 0.000000000000000000 ) ) ;
#27993 = CARTESIAN_POINT ( 'NONE',  ( 31.37220973900873489, -11.08107799475175348, -13.94606079199652982 ) ) ;
#27994 = CARTESIAN_POINT ( 'NONE',  ( 27.46788175125265141, -10.83975311022233079, -17.61709057740623408 ) ) ;
#27995 = ORIENTED_EDGE ( 'NONE', *, *, #21718, .T. ) ;
#27996 = ADVANCED_FACE ( 'NONE', ( #4313 ), #1894, .T. ) ;
#27997 = AXIS2_PLACEMENT_3D ( 'NONE', #19845, #793, #17117 ) ;
#27998 = PLANE ( 'NONE',  #22552 ) ;
#27999 = DIRECTION ( 'NONE',  ( 1.000000000000000000, 0.000000000000000000, 0.000000000000000000 ) ) ;
#28000 = CARTESIAN_POINT ( 'NONE',  ( 175.7287565553229456, -4.999999999999970690, -33.50000000000000000 ) ) ;
#28001 = LINE ( 'NONE', #27854, #16803 ) ;
#28002 = CIRCLE ( 'NONE', #19197, 5.000000000000000000 ) ;
#28003 = EDGE_CURVE ( 'NONE', #29073, #14905, #8879, .T. ) ;
#28004 = CARTESIAN_POINT ( 'NONE',  ( 10.71759363061643100, 16.64586103517192939, -15.95557720612771746 ) ) ;
#28005 = PLANE ( 'NONE',  #28309 ) ;
#28006 = VERTEX_POINT ( 'NONE', #18498 ) ;
#28007 = CARTESIAN_POINT ( 'NONE',  ( -13.00000000000000178, -2.870178842070716726E-15, 18.00000000000000000 ) ) ;
#28008 = VERTEX_POINT ( 'NONE', #27853 ) ;
#28009 = CARTESIAN_POINT ( 'NONE',  ( 9.921764701973689426, 16.38287729030320250, -16.50235149140834778 ) ) ;
#28010 = ORIENTED_EDGE ( 'NONE', *, *, #22321, .F. ) ;
#28011 = CARTESIAN_POINT ( 'NONE',  ( 27.90801785101615096, -12.26699769840798204, -14.39122685649866717 ) ) ;
#28012 = DIRECTION ( 'NONE',  ( -0.9510565162951536422, -2.566386769018988323E-16, 0.3090169943749475623 ) ) ;
#28013 =( LENGTH_UNIT ( ) NAMED_UNIT ( * ) SI_UNIT ( .MILLI., .METRE. ) );
#28014 = CARTESIAN_POINT ( 'NONE',  ( 26.57062215293289498, -11.41726559881178638, -18.09730928560479057 ) ) ;
#28015 = VERTEX_POINT ( 'NONE', #22638 ) ;
#28016 = DIRECTION ( 'NONE',  ( 2.908569913943825554E-16, -1.000000000000000000, 0.000000000000000000 ) ) ;
#28017 = CARTESIAN_POINT ( 'NONE',  ( 11.20364811077027767, 17.00960890128215297, -16.86645280501126365 ) ) ;
#28018 = CARTESIAN_POINT ( 'NONE',  ( 35.54170021948790748, -21.15354613602950096, -18.58520066250327929 ) ) ;
#28019 = CARTESIAN_POINT ( 'NONE',  ( 16.01392728624657025, 9.853228751548474662, -15.03783782146776105 ) ) ;
#28020 = ORIENTED_EDGE ( 'NONE', *, *, #6987, .T. ) ;
#28021 = ORIENTED_EDGE ( 'NONE', *, *, #5294, .T. ) ;
#28022 = EDGE_LOOP ( 'NONE', ( #9346, #21154, #16807, #20477 ) ) ;
#28023 = FACE_OUTER_BOUND ( 'NONE', #15840, .T. ) ;
#28024 = CARTESIAN_POINT ( 'NONE',  ( 26.06151603483908019, -7.281686956891486595, -19.93845510724469960 ) ) ;
#28025 = EDGE_LOOP ( 'NONE', ( #27539, #142, #24397, #2105 ) ) ;
#28026 = CARTESIAN_POINT ( 'NONE',  ( 131.1922820468854241, -10.00000000000000888, -13.59645775552055547 ) ) ;
#28027 = ORIENTED_EDGE ( 'NONE', *, *, #8988, .F. ) ;
#28028 = CARTESIAN_POINT ( 'NONE',  ( 17.90640022563237110, 0.6078909361919438981, -17.24624654394265377 ) ) ;
#28029 = CARTESIAN_POINT ( 'NONE',  ( 17.47084574460127371, 4.633898707001591788, -15.02533140066315198 ) ) ;
#28030 = AXIS2_PLACEMENT_3D ( 'NONE', #18538, #28196, #15940 ) ;
#28031 = EDGE_LOOP ( 'NONE', ( #13587, #3169, #6772, #20560 ) ) ;
#28032 = ADVANCED_FACE ( 'NONE', ( #6914 ), #20483, .T. ) ;
#28033 = DIRECTION ( 'NONE',  ( 0.9510565162951535312, 2.566386769018988816E-16, -0.3090169943749475623 ) ) ;
#28034 = EDGE_CURVE ( 'NONE', #24158, #4384, #16207, .T. ) ;
#28035 = VECTOR ( 'NONE', #7660, 1000.000000000000000 ) ;
#28036 = CARTESIAN_POINT ( 'NONE',  ( 0.000000000000000000, 0.000000000000000000, -2.450000000000000622 ) ) ;
#28037 = DIRECTION ( 'NONE',  ( -2.698458740408365879E-16, 1.000000000000000000, 0.000000000000000000 ) ) ;
#28038 = CARTESIAN_POINT ( 'NONE',  ( -8.000000000000000000, 4.618802153517001408, -0.7145311798163294092 ) ) ;
#28039 = PLANE ( 'NONE',  #25549 ) ;
#28040 = CARTESIAN_POINT ( 'NONE',  ( 9.907423389235603395, 16.44864837861227969, -16.50891839478055090 ) ) ;
#28041 = CARTESIAN_POINT ( 'NONE',  ( 24.43881766525553090, -7.056818123010307531, -19.17719463634885102 ) ) ;
#28042 = CARTESIAN_POINT ( 'NONE',  ( 19.79269262995316936, -1.159804626089355084, -18.29502107036499581 ) ) ;
#28044 = ORIENTED_EDGE ( 'NONE', *, *, #11471, .T. ) ;
#28043 = CARTESIAN_POINT ( 'NONE',  ( 36.54859390953724585, -23.18451583373416014, -17.99055332684694974 ) ) ;
#28045 = FILL_AREA_STYLE_COLOUR ( '', #28595 ) ;
#28046 = CARTESIAN_POINT ( 'NONE',  ( 12.71834232392635045, 8.667191563245470576, -14.95615232649864090 ) ) ;
#28047 = VECTOR ( 'NONE', #15455, 1000.000000000000000 ) ;
#28048 = DIRECTION ( 'NONE',  ( -0.5877852522924731371, -1.586114251531760728E-16, -0.8090169943749474513 ) ) ;
#28049 = CARTESIAN_POINT ( 'NONE',  ( 176.1922820468852535, -9.999999999999994671, -4.936203717676158398 ) ) ;
#28050 = CARTESIAN_POINT ( 'NONE',  ( 146.1922820468854241, -10.00000000000000355, -13.59645775552055902 ) ) ;
#28051 = ORIENTED_EDGE ( 'NONE', *, *, #21958, .T. ) ;
#28052 = DIRECTION ( 'NONE',  ( -1.000000000000000000, -4.440892098500622217E-16, -0.000000000000000000 ) ) ;
#28053 = CARTESIAN_POINT ( 'NONE',  ( 10.71759363061643100, 16.64586103517192939, -15.95557720612771746 ) ) ;
#28054 = ORIENTED_EDGE ( 'NONE', *, *, #17914, .F. ) ;
#28055 = LINE ( 'NONE', #25734, #22740 ) ;
#28056 = LINE ( 'NONE', #7110, #11259 ) ;
#28057 = ORIENTED_EDGE ( 'NONE', *, *, #25415, .T. ) ;
#28058 = APPLICATION_CONTEXT ( 'automotive_design' ) ;
#28059 = CARTESIAN_POINT ( 'NONE',  ( 15.46244301724551740, 3.702889819443702990, -17.82701508041758842 ) ) ;
#28060 = VERTEX_POINT ( 'NONE', #20932 ) ;
#28061 = CARTESIAN_POINT ( 'NONE',  ( 30.07451494818246474, -7.670792865742884992, -18.22619146169064663 ) ) ;
#28062 = ORIENTED_EDGE ( 'NONE', *, *, #16484, .T. ) ;
#28063 = CARTESIAN_POINT ( 'NONE',  ( 33.45813146310553066, -13.79317541067231723, -20.76837346131055639 ) ) ;
#28064 = CARTESIAN_POINT ( 'NONE',  ( 20.68391251823057075, 0.6588762160484964436, -13.99488169736409304 ) ) ;
#28065 = CARTESIAN_POINT ( 'NONE',  ( 19.52759782329482263, 6.073010510103808990, -18.47256557099433394 ) ) ;
#28066 = CARTESIAN_POINT ( 'NONE',  ( 24.92117679868390923, -7.366661744264540346, -12.55155079749028779 ) ) ;
#28067 = EDGE_CURVE ( 'NONE', #23858, #14791, #2192, .T. ) ;
#28068 = EDGE_CURVE ( 'NONE', #26594, #13044, #25523, .T. ) ;
#28069 = VECTOR ( 'NONE', #25344, 999.9999999999998863 ) ;
#28070 = ORIENTED_EDGE ( 'NONE', *, *, #2270, .T. ) ;
#28071 = EDGE_CURVE ( 'NONE', #25350, #26426, #20630, .T. ) ;
#28072 = CARTESIAN_POINT ( 'NONE',  ( 142.0152310637605524, -10.00000000000000355, -8.721423840594312082 ) ) ;
#28074 = VERTEX_POINT ( 'NONE', #2345 ) ;
#28073 = FACE_OUTER_BOUND ( 'NONE', #22521, .T. ) ;
#28075 = LINE ( 'NONE', #9099, #7536 ) ;
#28076 = DIRECTION ( 'NONE',  ( 0.9510565162951535312, 2.566386769018988816E-16, -0.3090169943749475623 ) ) ;
#28077 = CARTESIAN_POINT ( 'NONE',  ( 36.10807049912983757, -19.20547750251314767, -19.41448258861096932 ) ) ;
#28078 = CARTESIAN_POINT ( 'NONE',  ( 12.86487521014348623, 7.673917307032582791, -14.83936302970355037 ) ) ;
#28079 = EDGE_LOOP ( 'NONE', ( #14333, #22308 ) ) ;
#28080 = DIRECTION ( 'NONE',  ( 0.5877852522924731371, 1.586114251531760728E-16, 0.8090169943749474513 ) ) ;
#28081 = FACE_OUTER_BOUND ( 'NONE', #21487, .T. ) ;
#28082 = CARTESIAN_POINT ( 'NONE',  ( 10.47230989469697882, 16.45086252791593751, -17.33468480047602256 ) ) ;
#28083 = DIRECTION ( 'NONE',  ( 1.000000000000000000, 2.891205793294675861E-16, 0.000000000000000000 ) ) ;
#28084 = DIRECTION ( 'NONE',  ( -1.110223024625156540E-16, 0.000000000000000000, -1.000000000000000000 ) ) ;
#28085 = ORIENTED_EDGE ( 'NONE', *, *, #28526, .T. ) ;
#28086 = DIRECTION ( 'NONE',  ( 0.5877852522924731371, 0.000000000000000000, 0.8090169943749474513 ) ) ;
#28087 = CARTESIAN_POINT ( 'NONE',  ( 0.000000000000000000, 0.000000000000000000, 15.00000000000000000 ) ) ;
#28088 = LINE ( 'NONE', #9417, #13492 ) ;
#28089 = ORIENTED_EDGE ( 'NONE', *, *, #12552, .F. ) ;
#28090 = CARTESIAN_POINT ( 'NONE',  ( 9.667469407758799704, 16.22920693809672343, -17.88529630510330293 ) ) ;
#28091 = ADVANCED_FACE ( 'NONE', ( #11620 ), #15747, .T. ) ;
#28092 = ORIENTED_EDGE ( 'NONE', *, *, #21718, .F. ) ;
#28093 = CARTESIAN_POINT ( 'NONE',  ( 26.57181397551241275, -7.970695015363167713, -12.68872038106934852 ) ) ;
#28094 = CARTESIAN_POINT ( 'NONE',  ( 20.73027244251523626, 3.305903845835247434, -19.25852547563239625 ) ) ;
#28095 = LINE ( 'NONE', #27801, #23812 ) ;
#28096 = FACE_OUTER_BOUND ( 'NONE', #15461, .T. ) ;
#28097 = FACE_OUTER_BOUND ( 'NONE', #12457, .T. ) ;
#28098 = VECTOR ( 'NONE', #4995, 1000.000000000000000 ) ;
#28099 = CARTESIAN_POINT ( 'NONE',  ( 26.47511176763426377, -7.718147522161595830, -18.64721581247919602 ) ) ;
#28100 = EDGE_CURVE ( 'NONE', #17512, #21824, #18655, .T. ) ;
#28101 = AXIS2_PLACEMENT_3D ( 'NONE', #20095, #22232, #15663 ) ;
#28102 = EDGE_CURVE ( 'NONE', #28590, #28404, #1738, .T. ) ;
#28103 = ADVANCED_FACE ( 'NONE', ( #15898 ), #25229, .T. ) ;
#28105 = ORIENTED_EDGE ( 'NONE', *, *, #19745, .T. ) ;
#28104 = ADVANCED_BREP_SHAPE_REPRESENTATION ( '', ( #21281, #13190 ), #24415 ) ;
#28106 = EDGE_CURVE ( 'NONE', #9002, #13085, #2044, .T. ) ;
#28107 = DIRECTION ( 'NONE',  ( -0.9510565162951536422, 0.000000000000000000, -0.3090169943749472292 ) ) ;
#28108 = LINE ( 'NONE', #14164, #23342 ) ;
#28109 = VECTOR ( 'NONE', #12281, 1000.000000000000000 ) ;
#28110 = DIRECTION ( 'NONE',  ( 0.000000000000000000, 0.000000000000000000, 1.000000000000000000 ) ) ;
#28112 = DIRECTION ( 'NONE',  ( 0.000000000000000000, 0.000000000000000000, 1.000000000000000000 ) ) ;
#28111 = CIRCLE ( 'NONE', #26149, 2.500000000000000888 ) ;
#28113 = CARTESIAN_POINT ( 'NONE',  ( 10.35864927600819740, 16.97212461358170188, -17.91506874352199574 ) ) ;
#28114 = CARTESIAN_POINT ( 'NONE',  ( 35.54859390953724585, -22.18451583373416014, -17.64281456791166036 ) ) ;
#28115 = CARTESIAN_POINT ( 'NONE',  ( 33.47012763672258728, -12.84706786418751534, -19.72967806864707541 ) ) ;
#28116 = AXIS2_PLACEMENT_3D ( 'NONE', #7249, #13793, #7403 ) ;
#28117 = ORIENTED_EDGE ( 'NONE', *, *, #16348, .T. ) ;
#28118 = CARTESIAN_POINT ( 'NONE',  ( 13.59703899429919005, 7.722038565090276308, -15.53457947969411634 ) ) ;
#28119 = VERTEX_POINT ( 'NONE', #6757 ) ;
#28120 = CARTESIAN_POINT ( 'NONE',  ( 167.0152310637604955, -4.999999999999972466, -26.04193191628311155 ) ) ;
#28121 = CARTESIAN_POINT ( 'NONE',  ( 18.98200677837107264, -2.562081333921657933, -16.63161468174866187 ) ) ;
#28122 = CARTESIAN_POINT ( 'NONE',  ( 11.13911793526871463, 17.30555251181618814, -17.04533519337964975 ) ) ;
#28123 = DIRECTION ( 'NONE',  ( 0.9510565162951536422, 2.566386769018988816E-16, 0.3090169943749472292 ) ) ;
#28124 = ORIENTED_EDGE ( 'NONE', *, *, #7498, .T. ) ;
#28125 = VERTEX_POINT ( 'NONE', #25375 ) ;
#28126 = CARTESIAN_POINT ( 'NONE',  ( 9.641890818133653340, 17.66641459721583374, -17.82828029666912073 ) ) ;
#28127 = PLANE ( 'NONE',  #6243 ) ;
#28128 = VECTOR ( 'NONE', #4969, 1000.000000000000000 ) ;
#28129 = CARTESIAN_POINT ( 'NONE',  ( 11.31072706937237982, 10.01291882189198112, -15.92796669285280764 ) ) ;
#28130 = CARTESIAN_POINT ( 'NONE',  ( 152.2287565553229740, -4.999999999999976907, -12.16987298107781434 ) ) ;
#28131 = DIRECTION ( 'NONE',  ( -1.110223024625156540E-16, 0.000000000000000000, -1.000000000000000000 ) ) ;
#28132 = ORIENTED_EDGE ( 'NONE', *, *, #14575, .T. ) ;
#28133 = CARTESIAN_POINT ( 'NONE',  ( 4.000000000000019540, 6.928203230275512325, 0.000000000000000000 ) ) ;
#28134 = ORIENTED_EDGE ( 'NONE', *, *, #16759, .T. ) ;
#28135 = CARTESIAN_POINT ( 'NONE',  ( 10.47262648896379922, 16.44941058625191133, -17.33455387760982447 ) ) ;
#28136 = ORIENTED_EDGE ( 'NONE', *, *, #4949, .T. ) ;
#28138 = CARTESIAN_POINT ( 'NONE',  ( 32.66938126488236804, -9.629547215342803668, -18.20796273874843507 ) ) ;
#28137 = CIRCLE ( 'NONE', #27652, 2.500000000000002665 ) ;
#28139 = CARTESIAN_POINT ( 'NONE',  ( 13.52175692814481067, 9.804829593628518580, -15.59458061523717909 ) ) ;
#28140 = CARTESIAN_POINT ( 'NONE',  ( 23.56138260001205964, -6.829566487537672259, -18.05074380722902916 ) ) ;
#28141 = ORIENTED_EDGE ( 'NONE', *, *, #18133, .F. ) ;
#28142 = AXIS2_PLACEMENT_3D ( 'NONE', #27707, #11034, #10740 ) ;
#28143 = CARTESIAN_POINT ( 'NONE',  ( 136.1922820468854241, -10.00000000000000533, -22.25671179336495697 ) ) ;
#28144 = CARTESIAN_POINT ( 'NONE',  ( 5.637851296924623057E-15, 9.237604307034036566, -4.285468820183664818 ) ) ;
#28145 =( NAMED_UNIT ( * ) PLANE_ANGLE_UNIT ( ) SI_UNIT ( $, .RADIAN. ) );
#28146 = EDGE_LOOP ( 'NONE', ( #26022, #12089, #13808, #22889 ) ) ;
#28147 = CARTESIAN_POINT ( 'NONE',  ( 19.85629768685782537, 6.556105584440964584, -17.58075288388961965 ) ) ;
#28148 = CARTESIAN_POINT ( 'NONE',  ( 30.87383483136289541, -10.13329766739009052, -15.36655316835725138 ) ) ;
#28149 = EDGE_CURVE ( 'NONE', #26420, #15422, #4469, .T. ) ;
#28150 = EDGE_CURVE ( 'NONE', #22770, #23142, #7061, .T. ) ;
#28152 = ORIENTED_EDGE ( 'NONE', *, *, #23879, .T. ) ;
#28151 = EDGE_CURVE ( 'NONE', #14407, #17627, #21088, .T. ) ;
#28153 = FACE_OUTER_BOUND ( 'NONE', #3519, .T. ) ;
#28154 = CIRCLE ( 'NONE', #30112, 4.000000000000000000 ) ;
#28155 = PLANE ( 'NONE',  #19877 ) ;
#28156 = CARTESIAN_POINT ( 'NONE',  ( 21.57250875526980849, -5.000000000000011546, -66.39335505166295093 ) ) ;
#28157 = AXIS2_PLACEMENT_3D ( 'NONE', #1382, #29353, #8378 ) ;
#28158 = CARTESIAN_POINT ( 'NONE',  ( 0.000000000000000000, 0.000000000000000000, 0.000000000000000000 ) ) ;
#28159 = VECTOR ( 'NONE', #21844, 1000.000000000000000 ) ;
#28160 = UNCERTAINTY_MEASURE_WITH_UNIT (LENGTH_MEASURE( 1.000000000000000082E-05 ), #19239, 'distance_accuracy_value', 'NONE');
#28161 = CARTESIAN_POINT ( 'NONE',  ( 10.34291491886349235, 18.36418536769788901, -17.61263766090776528 ) ) ;
#28162 = CARTESIAN_POINT ( 'NONE',  ( 129.5152310637605808, -1.999999999999982236, -11.28819510263909187 ) ) ;
#28163 = EDGE_LOOP ( 'NONE', ( #25225, #22609, #8489, #10853 ) ) ;
#28164 = DIRECTION ( 'NONE',  ( -0.9510565162951536422, -2.566386769018988816E-16, -0.3090169943749472292 ) ) ;
#28165 = ORIENTED_EDGE ( 'NONE', *, *, #20027, .T. ) ;
#28166 = CARTESIAN_POINT ( 'NONE',  ( 11.46471852075427478, 9.306694396509932687, -15.86428581073749378 ) ) ;
#28167 = CARTESIAN_POINT ( 'NONE',  ( 22.65897993816424716, 3.718266075228530365, -15.21131701836175232 ) ) ;
#28168 = CARTESIAN_POINT ( 'NONE',  ( 142.0152310637606092, -1.999999999999978018, -15.61832212156129707 ) ) ;
#28169 = PLANE ( 'NONE',  #6199 ) ;
#28170 = CARTESIAN_POINT ( 'NONE',  ( 29.76939623719675510, -8.219725197086590995, -17.35520659559267287 ) ) ;
#28171 = ORIENTED_EDGE ( 'NONE', *, *, #26748, .F. ) ;
#28172 = FACE_OUTER_BOUND ( 'NONE', #3309, .T. ) ;
#28173 = CARTESIAN_POINT ( 'NONE',  ( 11.24654891281740987, 16.81286035451327265, -16.80493547870787197 ) ) ;
#28174 = ORIENTED_EDGE ( 'NONE', *, *, #10346, .T. ) ;
#28175 = CARTESIAN_POINT ( 'NONE',  ( 35.44226431226860541, -20.70683327756191616, -19.15799893943290755 ) ) ;
#28176 = FACE_OUTER_BOUND ( 'NONE', #19700, .T. ) ;
#28177 = PRESENTATION_LAYER_ASSIGNMENT (  '', '', ( #24242 ) ) ;
#28178 = DIRECTION ( 'NONE',  ( -0.8090169943749474513, -2.183098979609982436E-16, -0.5877852522924731371 ) ) ;
#28179 = CARTESIAN_POINT ( 'NONE',  ( 28.48873154519036888, -4.568419848414010609, -17.42663535687301035 ) ) ;
#28180 = ORIENTED_EDGE ( 'NONE', *, *, #26866, .F. ) ;
#28181 = CARTESIAN_POINT ( 'NONE',  ( 143.6922820468854525, -1.999999999999978018, -17.92658477444275889 ) ) ;
#28182 = VERTEX_POINT ( 'NONE', #16664 ) ;
#28183 = SURFACE_STYLE_USAGE ( .BOTH. , #12105 ) ;
#28184 = CARTESIAN_POINT ( 'NONE',  ( 18.25949499138229726, 0.6315596619015936275, -15.69045325149238934 ) ) ;
#28185 = VECTOR ( 'NONE', #13782, 1000.000000000000000 ) ;
#28186 = CARTESIAN_POINT ( 'NONE',  ( 15.27107031639597423, 6.121678041989828678, -18.36639460046777828 ) ) ;
#28187 = ADVANCED_FACE ( 'NONE', ( #9931 ), #26137, .T. ) ;
#28188 = ORIENTED_EDGE ( 'NONE', *, *, #27653, .F. ) ;
#28190 = ORIENTED_EDGE ( 'NONE', *, *, #1757, .F. ) ;
#28189 = EDGE_CURVE ( 'NONE', #22328, #2206, #11771, .T. ) ;
#28191 = DIRECTION ( 'NONE',  ( -2.698458740408365879E-16, 1.000000000000000000, 0.000000000000000000 ) ) ;
#28192 = AXIS2_PLACEMENT_3D ( 'NONE', #25374, #4760, #13758 ) ;
#28193 = CARTESIAN_POINT ( 'NONE',  ( 172.2287565553228887, -9.999999999999996447, -12.16987298107780369 ) ) ;
#28194 = PLANE ( 'NONE',  #20738 ) ;
#28195 = CARTESIAN_POINT ( 'NONE',  ( 0.000000000000000000, 1.162403506782538081E-16, -4.187999999999997947 ) ) ;
#28196 = DIRECTION ( 'NONE',  ( -0.5000000000000027756, 0.8660254037844370423, 0.000000000000000000 ) ) ;
#28197 = VECTOR ( 'NONE', #17630, 1000.000000000000000 ) ;
#28198 = CARTESIAN_POINT ( 'NONE',  ( 9.675370519060759733, 17.51287242109451014, -17.23928541814325399 ) ) ;
#28199 = CARTESIAN_POINT ( 'NONE',  ( 20.13453040791782911, -1.388291987844697317, -13.01173725324373009 ) ) ;
#28200 = CARTESIAN_POINT ( 'NONE',  ( 19.47299019774181161, -1.479546722229555744, -17.51644493673600067 ) ) ;
#28202 = VERTEX_POINT ( 'NONE', #7656 ) ;
#28201 = CARTESIAN_POINT ( 'NONE',  ( 36.54276536429808431, -23.15833126744076509, -18.75760452913613463 ) ) ;
#28203 = LINE ( 'NONE', #9520, #7593 ) ;
#28204 = VECTOR ( 'NONE', #24580, 1000.000000000000000 ) ;
#28205 = LINE ( 'NONE', #11666, #2045 ) ;
#28206 = LINE ( 'NONE', #14253, #9313 ) ;
#28207 = CARTESIAN_POINT ( 'NONE',  ( 134.5152310637605524, -4.999999999999981348, -30.37205893520530964 ) ) ;
#28208 = CARTESIAN_POINT ( 'NONE',  ( 15.87806330829146617, 7.947701475055697351, -19.83831759000646855 ) ) ;
#28209 = VERTEX_POINT ( 'NONE', #19244 ) ;
#28210 = CARTESIAN_POINT ( 'NONE',  ( 173.6922820468852535, -1.999999999999970024, 2.247092850131519715 ) ) ;
#28211 = CARTESIAN_POINT ( 'NONE',  ( 10.72284644870490489, 16.62177094183959980, -15.95334970537801134 ) ) ;
#28212 = EDGE_CURVE ( 'NONE', #102, #9595, #28599, .T. ) ;
#28213 = AXIS2_PLACEMENT_3D ( 'NONE', #7212, #16206, #27999 ) ;
#28214 = ORIENTED_EDGE ( 'NONE', *, *, #8323, .F. ) ;
#28215 = CARTESIAN_POINT ( 'NONE',  ( 36.04859390953723874, -22.18451583373416014, -15.00000000000000000 ) ) ;
#28216 = DIRECTION ( 'NONE',  ( 0.9510565162951536422, 0.000000000000000000, -0.3090169943749475623 ) ) ;
#28217 = ORIENTED_EDGE ( 'NONE', *, *, #11899, .T. ) ;
#28218 = PRODUCT_DEFINITION ( 'UNKNOWN', '', #2468, #23539 ) ;
#28219 = CARTESIAN_POINT ( 'NONE',  ( 15.87806330829146617, 7.947701475055697351, -19.83831759000646855 ) ) ;
#28220 = CARTESIAN_POINT ( 'NONE',  ( 30.36731020202829612, -7.149780978071095028, -17.08985122409953306 ) ) ;
#28221 = EDGE_LOOP ( 'NONE', ( #1381, #2485, #24540, #14487 ) ) ;
#28222 = CARTESIAN_POINT ( 'NONE',  ( 35.54502023521215648, -22.16846120802060938, -18.59538644662325524 ) ) ;
#28223 = CARTESIAN_POINT ( 'NONE',  ( 23.04877348721027630, -0.9239720737610787049, -14.85003467231304342 ) ) ;
#28224 = CARTESIAN_POINT ( 'NONE',  ( 18.37740474667574730, 3.980509343919368614, -15.11632106699347844 ) ) ;
#28225 = AXIS2_PLACEMENT_3D ( 'NONE', #3098, #21685, #5213 ) ;
#28226 = CARTESIAN_POINT ( 'NONE',  ( 29.75294099516071711, -10.02427176990993196, -17.65830536592410738 ) ) ;
#28227 = CIRCLE ( 'NONE', #9164, 5.000000000000000888 ) ;
#28228 = ORIENTED_EDGE ( 'NONE', *, *, #175, .T. ) ;
#28229 = FACE_OUTER_BOUND ( 'NONE', #14738, .T. ) ;
#28230 = DIRECTION ( 'NONE',  ( 1.000000000000000000, 0.000000000000000000, 0.000000000000000000 ) ) ;
#28231 = CARTESIAN_POINT ( 'NONE',  ( 157.0152310637604671, -4.999999999999975131, -1.743219247438259813E-14 ) ) ;
#28232 = PLANE ( 'NONE',  #29800 ) ;
#28233 = CARTESIAN_POINT ( 'NONE',  ( 34.52649160559821695, -12.12091213808323964, -18.92441241263726326 ) ) ;
#28234 = CARTESIAN_POINT ( 'NONE',  ( 9.641350835837977584, 17.66889102485563612, -17.91507476468484938 ) ) ;
#28235 = ORIENTED_EDGE ( 'NONE', *, *, #3825, .T. ) ;
#28236 = CARTESIAN_POINT ( 'NONE',  ( 152.0152310637605240, -1.999999999999975797, -6.958068083716895558 ) ) ;
#28237 = PLANE ( 'NONE',  #13888 ) ;
#28238 = CARTESIAN_POINT ( 'NONE',  ( 12.03206445085756116, 9.298183410334813104, -16.68962916345529024 ) ) ;
#28239 = DIRECTION ( 'NONE',  ( 0.5877852522924731371, 1.586114251531760728E-16, -0.8090169943749474513 ) ) ;
#28240 = CARTESIAN_POINT ( 'NONE',  ( 4.000000000000000000, 0.3904826640788077730, -2.450000000000000622 ) ) ;
#28241 = EDGE_CURVE ( 'NONE', #19084, #23150, #21687, .T. ) ;
#28242 = EDGE_CURVE ( 'NONE', #4596, #19824, #26288, .T. ) ;
#28243 = ORIENTED_EDGE ( 'NONE', *, *, #3987, .F. ) ;
#28244 = VECTOR ( 'NONE', #26480, 1000.000000000000000 ) ;
#28245 = FACE_OUTER_BOUND ( 'NONE', #20030, .T. ) ;
#28246 = EDGE_CURVE ( 'NONE', #20619, #319, #5374, .T. ) ;
#28247 = CARTESIAN_POINT ( 'NONE',  ( 154.5152310637604955, -10.00000000000000000, -13.05155085951651195 ) ) ;
#28248 = ORIENTED_EDGE ( 'NONE', *, *, #24466, .T. ) ;
#28249 = EDGE_CURVE ( 'NONE', #5542, #16563, #23536, .T. ) ;
#28250 = CARTESIAN_POINT ( 'NONE',  ( 133.6922820468854241, -1.999999999999980904, -15.07341522555727309 ) ) ;
#28251 = ORIENTED_EDGE ( 'NONE', *, *, #8071, .T. ) ;
#28252 = CARTESIAN_POINT ( 'NONE',  ( 9.675977061968080051, 16.19018975141917593, -17.88172274351348889 ) ) ;
#28253 = CARTESIAN_POINT ( 'NONE',  ( 23.44948677240984480, -6.246615351793893822, -14.99377964970044808 ) ) ;
#28254 = CARTESIAN_POINT ( 'NONE',  ( 26.78588127033857091, -2.187643107580064861, -16.18476928258297676 ) ) ;
#28255 = CARTESIAN_POINT ( 'NONE',  ( 130.7287565553229172, -4.999999999999983125, -36.50000000000000711 ) ) ;
#28256 = FACE_OUTER_BOUND ( 'NONE', #25323, .T. ) ;
#28257 = PLANE ( 'NONE',  #15185 ) ;
#28258 = CARTESIAN_POINT ( 'NONE',  ( 27.91615220763155847, -6.225400021157185826, -17.67258836524805332 ) ) ;
#28259 = LINE ( 'NONE', #21187, #4225 ) ;
#28260 = VERTEX_POINT ( 'NONE', #2502 ) ;
#28261 = CARTESIAN_POINT ( 'NONE',  ( 132.2287565553230024, -10.00000000000000888, -29.49038105676660138 ) ) ;
#28262 = VECTOR ( 'NONE', #15604, 1000.000000000000000 ) ;
#28263 = DIRECTION ( 'NONE',  ( -0.5877852522924731371, -1.586114251531760728E-16, -0.8090169943749474513 ) ) ;
#28264 = PLANE ( 'NONE',  #5856 ) ;
#28265 = LINE ( 'NONE', #16772, #5064 ) ;
#28266 = VECTOR ( 'NONE', #25483, 1000.000000000000000 ) ;
#28267 = CARTESIAN_POINT ( 'NONE',  ( 10.47224519147693478, 16.45115926513079074, -17.33471155705291977 ) ) ;
#28268 = LINE ( 'NONE', #10042, #7726 ) ;
#28269 = CLOSED_SHELL ( 'NONE', ( #10445, #6089, #26784, #18378, #9507, #2144 ) ) ;
#28270 = CARTESIAN_POINT ( 'NONE',  ( 32.74314609665832165, -11.10724048739539782, -18.62249297335446840 ) ) ;
#28271 = ORIENTED_EDGE ( 'NONE', *, *, #7811, .T. ) ;
#28272 = CARTESIAN_POINT ( 'NONE',  ( 13.38012098442259834, 7.626178612778168109, -15.70746696265163145 ) ) ;
#28273 = CYLINDRICAL_SURFACE ( 'NONE', #6142, 4.000000000000000000 ) ;
#28274 = CARTESIAN_POINT ( 'NONE',  ( 17.21692058948253035, 4.245457944912791604, -14.13226496128363863 ) ) ;
#28275 = CARTESIAN_POINT ( 'NONE',  ( 11.27864710625743427, 16.66565394782951515, -16.78350969486689692 ) ) ;
#28276 = CARTESIAN_POINT ( 'NONE',  ( 125.7287565553229172, -9.999999999999994671, -33.50000000000000000 ) ) ;
#28277 = ORIENTED_EDGE ( 'NONE', *, *, #18728, .T. ) ;
#28278 = EDGE_CURVE ( 'NONE', #30251, #23755, #349, .T. ) ;
#28279 = EDGE_LOOP ( 'NONE', ( #18571, #11237, #10496, #1834 ) ) ;
#28280 = CARTESIAN_POINT ( 'NONE',  ( 9.641566850259106758, 17.66790035518494051, -17.86107206016944460 ) ) ;
#28281 = DIRECTION ( 'NONE',  ( -0.000000000000000000, -0.000000000000000000, -1.000000000000000000 ) ) ;
#28282 = EDGE_CURVE ( 'NONE', #9388, #24164, #2639, .T. ) ;
#28283 = CARTESIAN_POINT ( 'NONE',  ( 9.642214727206800617, 17.66492910891761525, -17.80644250212319690 ) ) ;
#28284 = DIRECTION ( 'NONE',  ( -2.698458740408365879E-16, 1.000000000000000000, 0.000000000000000000 ) ) ;
#28285 = EDGE_CURVE ( 'NONE', #16899, #7751, #18799, .T. ) ;
#28286 = ORIENTED_EDGE ( 'NONE', *, *, #25976, .F. ) ;
#28287 = LINE ( 'NONE', #8073, #2792 ) ;
#28288 = ORIENTED_EDGE ( 'NONE', *, *, #10523, .T. ) ;
#28289 = CARTESIAN_POINT ( 'NONE',  ( 10.47008273352651564, 16.46107657294071203, -17.33567129194344858 ) ) ;
#28290 = EDGE_LOOP ( 'NONE', ( #5638, #2311, #23990, #14727 ) ) ;
#28291 = AXIS2_PLACEMENT_3D ( 'NONE', #25493, #4581, #20292 ) ;
#28292 = CARTESIAN_POINT ( 'NONE',  ( 36.09161981528372110, -20.13157329416283048, -20.44814669990763889 ) ) ;
#28293 = CARTESIAN_POINT ( 'NONE',  ( 27.76312469413510442, -10.32446017237915648, -18.80420148706337358 ) ) ;
#28294 = CARTESIAN_POINT ( 'NONE',  ( 26.72358035960067824, -3.685970424986596772, -17.59444040205794835 ) ) ;
#28295 = DIRECTION ( 'NONE',  ( -0.8090169943749474513, -2.183098979609982436E-16, -0.5877852522924731371 ) ) ;
#28296 = CIRCLE ( 'NONE', #10195, 40.00000000000000711 ) ;
#28297 = CARTESIAN_POINT ( 'NONE',  ( 35.06179249480944549, -15.50510465796065596, -20.14053939611612520 ) ) ;
#28298 = DIRECTION ( 'NONE',  ( 0.000000000000000000, 0.000000000000000000, 1.000000000000000000 ) ) ;
#28299 = CARTESIAN_POINT ( 'NONE',  ( 19.04375517570889187, 9.961537237715642590, -16.65452713690489617 ) ) ;
#28300 = CARTESIAN_POINT ( 'NONE',  ( 29.74223563811278481, -10.39579538818624549, -13.90533736129563813 ) ) ;
#28301 = ORIENTED_EDGE ( 'NONE', *, *, #12111, .F. ) ;
#28302 = FACE_BOUND ( 'NONE', #25512, .T. ) ;
#28303 = EDGE_CURVE ( 'NONE', #25132, #1603, #10080, .T. ) ;
#28304 = CARTESIAN_POINT ( 'NONE',  ( 3.918937403516957740, -5.000000000000016875, 12.06124913002446597 ) ) ;
#28305 = CARTESIAN_POINT ( 'NONE',  ( 171.1922820468853388, -1.999999999999970468, -22.25671179336496053 ) ) ;
#28306 = VECTOR ( 'NONE', #14311, 1000.000000000000000 ) ;
#28307 = DIRECTION ( 'NONE',  ( 1.110223024625156540E-16, 2.995891024602366092E-32, 1.000000000000000000 ) ) ;
#28308 = CARTESIAN_POINT ( 'NONE',  ( 152.0152310637606092, -1.999999999999974465, -32.93883019725009120 ) ) ;
#28309 = AXIS2_PLACEMENT_3D ( 'NONE', #23854, #11921, #504 ) ;
#28310 = VECTOR ( 'NONE', #23156, 1000.000000000000000 ) ;
#28311 = CARTESIAN_POINT ( 'NONE',  ( 10.69507909363156628, 16.74911557172037391, -15.96836912279556309 ) ) ;
#28312 = FACE_OUTER_BOUND ( 'NONE', #12715, .T. ) ;
#28313 = LINE ( 'NONE', #21400, #12505 ) ;
#28314 = EDGE_LOOP ( 'NONE', ( #13687, #13929, #18514, #27120 ) ) ;
#28315 = CARTESIAN_POINT ( 'NONE',  ( 9.917332382238186028, 16.40320447359955125, -16.50418441153501448 ) ) ;
#28316 = ORIENTED_EDGE ( 'NONE', *, *, #2382, .F. ) ;
#28317 = EDGE_CURVE ( 'NONE', #20741, #22085, #16806, .T. ) ;
#28318 = EDGE_CURVE ( 'NONE', #14857, #19188, #21394, .T. ) ;
#28319 = CARTESIAN_POINT ( 'NONE',  ( 9.667809135389937580, 16.22764890387498227, -17.88510185254740747 ) ) ;
#28320 = CARTESIAN_POINT ( 'NONE',  ( 23.36829581039676640, 3.373260575288004937, -18.04565522708177738 ) ) ;
#28321 = CARTESIAN_POINT ( 'NONE',  ( 163.6922820468853956, -1.999999999999971800, -35.24709285013155835 ) ) ;
#28322 = LINE ( 'NONE', #18668, #11066 ) ;
#28323 = EDGE_CURVE ( 'NONE', #10099, #28570, #23850, .T. ) ;
#28324 = CARTESIAN_POINT ( 'NONE',  ( 27.44219139316946965, -6.774709612358828181, -18.29578255718776703 ) ) ;
#28325 = ORIENTED_EDGE ( 'NONE', *, *, #18172, .F. ) ;
#28326 = DIRECTION ( 'NONE',  ( 0.3090169943749475623, 8.338696094058001131E-17, 0.9510565162951536422 ) ) ;
#28327 = EDGE_CURVE ( 'NONE', #12785, #25944, #9636, .T. ) ;
#28328 = CARTESIAN_POINT ( 'NONE',  ( 11.21766632152761822, 16.94531959984159641, -16.84123939818963223 ) ) ;
#28329 = AXIS2_PLACEMENT_3D ( 'NONE', #1682, #13406, #22732 ) ;
#28330 = VERTEX_POINT ( 'NONE', #2950 ) ;
#28331 = VECTOR ( 'NONE', #26493, 1000.000000000000000 ) ;
#28333 = VECTOR ( 'NONE', #1906, 1000.000000000000000 ) ;
#28332 = CARTESIAN_POINT ( 'NONE',  ( 33.36629945566365052, -11.89386221509426633, -18.35752312617820081 ) ) ;
#28334 = CARTESIAN_POINT ( 'NONE',  ( 15.73644607668725826, 9.740111719757674535, -14.94734896276200153 ) ) ;
#28335 = DIRECTION ( 'NONE',  ( 1.000000000000000000, 2.698458740408367851E-16, 0.000000000000000000 ) ) ;
#28336 = CARTESIAN_POINT ( 'NONE',  ( 9.084523633786250940, 16.30981489620654301, -17.07623073379102507 ) ) ;
#28337 = CARTESIAN_POINT ( 'NONE',  ( 25.50153931649120764, -9.195696458170099064, -12.32940773450113170 ) ) ;
#28338 = VERTEX_POINT ( 'NONE', #5062 ) ;
#28339 = DIRECTION ( 'NONE',  ( 0.000000000000000000, 0.000000000000000000, 1.000000000000000000 ) ) ;
#28340 = AXIS2_PLACEMENT_3D ( 'NONE', #81, #20113, #19963 ) ;
#28341 = CARTESIAN_POINT ( 'NONE',  ( 20.38603433104324480, 7.363110203939331022, -17.91596102798271062 ) ) ;
#28342 = CARTESIAN_POINT ( 'NONE',  ( 17.06308625499319831, 6.674173717519480853, -15.25088821959635865 ) ) ;
#28343 = EDGE_LOOP ( 'NONE', ( #10109, #25782, #16971, #14771, #27494 ) ) ;
#28344 = DIRECTION ( 'NONE',  ( -0.9510565162951536422, -2.566386769018988323E-16, 0.3090169943749475623 ) ) ;
#28345 = VERTEX_POINT ( 'NONE', #12228 ) ;
#28346 = CARTESIAN_POINT ( 'NONE',  ( 0.000000000000000000, 1.178949249685215417, 2.041999999999998483 ) ) ;
#28347 = DIRECTION ( 'NONE',  ( 0.5877852522924731371, 1.586114251531760728E-16, -0.8090169943749474513 ) ) ;
#28348 = VECTOR ( 'NONE', #20860, 1000.000000000000000 ) ;
#28349 = CARTESIAN_POINT ( 'NONE',  ( 133.7287565553229456, -9.999999999999980460, 0.5000000000000029976 ) ) ;
#28350 = CARTESIAN_POINT ( 'NONE',  ( 63.44486372867152824, -29.99999999999998934, -15.00000000000000000 ) ) ;
#28351 = VECTOR ( 'NONE', #23359, 1000.000000000000000 ) ;
#28352 = DIRECTION ( 'NONE',  ( 1.110223024625156540E-16, 2.995891024602366092E-32, 1.000000000000000000 ) ) ;
#28353 = CARTESIAN_POINT ( 'NONE',  ( 9.641404825192898542, 17.66864342279195199, -17.88841768828662282 ) ) ;
#28354 = CARTESIAN_POINT ( 'NONE',  ( 28.66609726738115071, -6.663921799113727396, -16.65640135049372006 ) ) ;
#28355 = CARTESIAN_POINT ( 'NONE',  ( 20.31878617967674217, -0.6648838724932636390, -18.90140657046049455 ) ) ;
#28357 = ORIENTED_EDGE ( 'NONE', *, *, #26225, .T. ) ;
#28356 = CARTESIAN_POINT ( 'NONE',  ( 32.98128152813007574, -11.80310687477359188, -20.53574887303233609 ) ) ;
#28358 = FACE_OUTER_BOUND ( 'NONE', #24115, .T. ) ;
#28359 = DIRECTION ( 'NONE',  ( 0.9510565162951536422, 2.566386769018988816E-16, 0.3090169943749472292 ) ) ;
#28360 = ADVANCED_FACE ( 'NONE', ( #12077 ), #14352, .T. ) ;
#28361 = CARTESIAN_POINT ( 'NONE',  ( 151.1922820468853956, -1.999999999999975797, -10.74328820663507678 ) ) ;
#28362 = LINE ( 'NONE', #2549, #21716 ) ;
#28363 = CARTESIAN_POINT ( 'NONE',  ( 15.22033579473957410, 7.355362781181614018, -19.64495939069069763 ) ) ;
#28364 = FACE_OUTER_BOUND ( 'NONE', #20953, .T. ) ;
#28365 = EDGE_CURVE ( 'NONE', #18308, #19412, #17258, .T. ) ;
#28366 = CARTESIAN_POINT ( 'NONE',  ( 10.33811712360892443, 18.38618866831204102, -17.91390369733608523 ) ) ;
#28367 = CARTESIAN_POINT ( 'NONE',  ( 20.00000000000000355, 60.00000000000000711, -24.99999999999999645 ) ) ;
#28368 = CARTESIAN_POINT ( 'NONE',  ( 133.6922820468854241, -10.00000000000000711, 2.247092850131519715 ) ) ;
#28369 = CARTESIAN_POINT ( 'NONE',  ( 14.33367420948735393, 6.252843122977492563, -16.41390433006782956 ) ) ;
#28370 = CARTESIAN_POINT ( 'NONE',  ( 14.32916401545863039, 6.225515681311286187, -14.04012878508491369 ) ) ;
#28371 = VERTEX_POINT ( 'NONE', #14955 ) ;
#28373 = AXIS2_PLACEMENT_3D ( 'NONE', #12003, #4548, #13837 ) ;
#28372 = CARTESIAN_POINT ( 'NONE',  ( 35.54787733059053778, -22.18129662410796854, -18.46719521006932396 ) ) ;
#28374 = CARTESIAN_POINT ( 'NONE',  ( 24.19805618307960060, -0.7920880973371497991, -16.79971198345035432 ) ) ;
#28375 = AXIS2_PLACEMENT_3D ( 'NONE', #22395, #13522, #1798 ) ;
#28376 = EDGE_LOOP ( 'NONE', ( #3251, #4285, #22905, #27975 ) ) ;
#28377 = CARTESIAN_POINT ( 'NONE',  ( 21.44849557978440657, 3.047722651366359781, -15.04725200041975341 ) ) ;
#28378 = CARTESIAN_POINT ( 'NONE',  ( 27.75006011364712322, -11.91879133414019698, -17.49150313904273801 ) ) ;
#28379 = VERTEX_POINT ( 'NONE', #21997 ) ;
#28380 = LINE ( 'NONE', #21913, #18183 ) ;
#28381 = EDGE_CURVE ( 'NONE', #13222, #2910, #24290, .T. ) ;
#28383 = ORIENTED_EDGE ( 'NONE', *, *, #4022, .F. ) ;
#28382 = DIRECTION ( 'NONE',  ( 0.3090169943749472292, 8.338696094057992503E-17, -0.9510565162951536422 ) ) ;
#28384 = DIRECTION ( 'NONE',  ( 0.3090169943749472292, 8.338696094057992503E-17, -0.9510565162951536422 ) ) ;
#28385 = LINE ( 'NONE', #26065, #29303 ) ;
#28386 = CARTESIAN_POINT ( 'NONE',  ( 34.66364242521329686, -12.71642730124038501, -18.97786663347613256 ) ) ;
#28387 = AXIS2_PLACEMENT_3D ( 'NONE', #11964, #16858, #9521 ) ;
#28388 = CARTESIAN_POINT ( 'NONE',  ( 9.641350810849047548, 17.66889113945805789, -17.92015940598198753 ) ) ;
#28389 = ORIENTED_EDGE ( 'NONE', *, *, #23802, .F. ) ;
#28390 = DIRECTION ( 'NONE',  ( 1.000000000000000000, 2.698458740408365879E-16, 0.000000000000000000 ) ) ;
#28391 = DIRECTION ( 'NONE',  ( 1.000000000000000000, 0.000000000000000000, 0.000000000000000000 ) ) ;
#28392 = CARTESIAN_POINT ( 'NONE',  ( 12.14965596459611774, 8.983642127099937369, -16.62385966901067391 ) ) ;
#28393 = EDGE_CURVE ( 'NONE', #5343, #21323, #22456, .T. ) ;
#28394 = LINE ( 'NONE', #7447, #2949 ) ;
#28395 = CARTESIAN_POINT ( 'NONE',  ( 3.999999999999999112, 1.935983797701081643, -2.200530693383769609 ) ) ;
#28396 = ORIENTED_EDGE ( 'NONE', *, *, #11687, .F. ) ;
#28397 = DIRECTION ( 'NONE',  ( 0.9510565162951536422, 0.000000000000000000, -0.3090169943749475623 ) ) ;
#28398 = FACE_OUTER_BOUND ( 'NONE', #8852, .T. ) ;
#28399 = ORIENTED_EDGE ( 'NONE', *, *, #28034, .T. ) ;
#28400 = CARTESIAN_POINT ( 'NONE',  ( 162.0152310637605524, -4.999999999999973355, -32.93883019725009120 ) ) ;
#28401 = ORIENTED_EDGE ( 'NONE', *, *, #22840, .F. ) ;
#28402 = CARTESIAN_POINT ( 'NONE',  ( 13.37103985619203783, 7.622196798368539028, -15.71470239503888422 ) ) ;
#28403 = CARTESIAN_POINT ( 'NONE',  ( 25.76376746566330311, -3.589579415956118069, -17.31313795625071350 ) ) ;
#28404 = VERTEX_POINT ( 'NONE', #29373 ) ;
#28405 = CARTESIAN_POINT ( 'NONE',  ( 21.34960977245966873, -3.524359730468174412, -18.69795900347392248 ) ) ;
#28406 = DIRECTION ( 'NONE',  ( 0.9510565162951536422, 2.566386769018988816E-16, 0.3090169943749472292 ) ) ;
#28407 = CARTESIAN_POINT ( 'NONE',  ( 132.0152310637605524, -4.999999999999982236, -1.465663491281971624E-14 ) ) ;
#28408 = DIRECTION ( 'NONE',  ( 0.9510565162951536422, 2.566386769018988816E-16, 0.3090169943749472292 ) ) ;
#28409 = DIRECTION ( 'NONE',  ( -0.5877852522924731371, -1.586114251531760235E-16, 0.8090169943749474513 ) ) ;
#28410 = EDGE_CURVE ( 'NONE', #24264, #29043, #11299, .T. ) ;
#28411 = DIRECTION ( 'NONE',  ( -0.8090169943749474513, -2.183098979609982436E-16, 0.5877852522924731371 ) ) ;
#28412 = DIRECTION ( 'NONE',  ( 1.000000000000000000, 2.891205793294675861E-16, 0.000000000000000000 ) ) ;
#28413 = EDGE_CURVE ( 'NONE', #13701, #12555, #29055, .T. ) ;
#28414 = FACE_OUTER_BOUND ( 'NONE', #11936, .T. ) ;
#28415 = DIRECTION ( 'NONE',  ( 0.5877852522924731371, 1.586114251531760728E-16, 0.8090169943749474513 ) ) ;
#28416 = CARTESIAN_POINT ( 'NONE',  ( 12.02685106364323531, 9.321538569219327997, -16.69182734290254899 ) ) ;
#28417 = CARTESIAN_POINT ( 'NONE',  ( 176.1922820468853104, -9.999999999999994671, -22.25671179336496053 ) ) ;
#28418 = CARTESIAN_POINT ( 'NONE',  ( 33.33926371295168423, -12.28475995124076903, -19.67523791759492013 ) ) ;
#28419 = ORIENTED_EDGE ( 'NONE', *, *, #15787, .T. ) ;
#28420 = CARTESIAN_POINT ( 'NONE',  ( 8.944584683310379702, 16.95159276115599667, -17.92279151347708677 ) ) ;
#28421 = EDGE_LOOP ( 'NONE', ( #21782, #19335, #2509, #20461 ) ) ;
#28422 = CARTESIAN_POINT ( 'NONE',  ( 63.44486372867149981, -20.00000000000003197, -186.4312945166758482 ) ) ;
#28423 = AXIS2_PLACEMENT_3D ( 'NONE', #25220, #2035, #4153 ) ;
#28424 = CARTESIAN_POINT ( 'NONE',  ( 21.48529164538665981, 5.106035544247377267, -18.65531623833433628 ) ) ;
#28425 = CARTESIAN_POINT ( 'NONE',  ( 12.75119036009696316, 9.912382880115339745, -16.17456125963731850 ) ) ;
#28426 = CARTESIAN_POINT ( 'NONE',  ( 19.18522118495666007, -5.000000000000012434, -59.04603939800706058 ) ) ;
#28427 = ORIENTED_EDGE ( 'NONE', *, *, #7768, .T. ) ;
#28428 = CARTESIAN_POINT ( 'NONE',  ( 11.46775782571576130, 9.292755756535285627, -15.86302895122203616 ) ) ;
#28429 = CARTESIAN_POINT ( 'NONE',  ( 420.0000000000002274, 25.64101615137744616, 12.00000000000000178 ) ) ;
#28430 = CARTESIAN_POINT ( 'NONE',  ( 10.43540724046455992, 14.02724713458965233, -16.28994223329847202 ) ) ;
#28431 = CARTESIAN_POINT ( 'NONE',  ( 176.1922820468853388, -9.999999999999994671, -30.91696583120936026 ) ) ;
#28432 = ORIENTED_EDGE ( 'NONE', *, *, #2863, .F. ) ;
#28433 = CARTESIAN_POINT ( 'NONE',  ( 130.7287565553229456, -4.999999999999982236, -30.76635726929466585 ) ) ;
#28434 = EDGE_LOOP ( 'NONE', ( #27945, #17936, #17419, #7897 ) ) ;
#28435 = CARTESIAN_POINT ( 'NONE',  ( 10.36430886937160167, 16.94616899698690204, -17.73806594831300032 ) ) ;
#28436 = ORIENTED_EDGE ( 'NONE', *, *, #9795, .F. ) ;
#28437 = CARTESIAN_POINT ( 'NONE',  ( 36.54859390953724585, -22.18451583373416014, -17.78191007148576475 ) ) ;
#28438 = CARTESIAN_POINT ( 'NONE',  ( 13.75440121443578079, 9.907639265912045801, -15.40915901261088905 ) ) ;
#28439 = CARTESIAN_POINT ( 'NONE',  ( 25.97851742199650005, -11.98992670343847244, -16.97112261376066655 ) ) ;
#28440 = VECTOR ( 'NONE', #29200, 1000.000000000000000 ) ;
#28441 = ORIENTED_EDGE ( 'NONE', *, *, #5714, .T. ) ;
#28442 = DIRECTION ( 'NONE',  ( 0.9510565162951535312, 2.566386769018988816E-16, -0.3090169943749475623 ) ) ;
#28443 = VERTEX_POINT ( 'NONE', #17558 ) ;
#28444 = LINE ( 'NONE', #25664, #10817 ) ;
#28445 = CARTESIAN_POINT ( 'NONE',  ( 18.58892183794801056, 4.077935791202882854, -15.09018232067737841 ) ) ;
#28446 = CARTESIAN_POINT ( 'NONE',  ( 25.52642221012979462, -9.988304178644780151, -15.98026830291908773 ) ) ;
#28447 = VERTEX_POINT ( 'NONE', #17700 ) ;
#28448 = VECTOR ( 'NONE', #23796, 1000.000000000000000 ) ;
#28449 = ORIENTED_EDGE ( 'NONE', *, *, #26052, .T. ) ;
#28450 = FACE_BOUND ( 'NONE', #9150, .T. ) ;
#28451 = EDGE_CURVE ( 'NONE', #15396, #7245, #1247, .T. ) ;
#28452 = ADVANCED_FACE ( 'NONE', ( #8093 ), #27061, .T. ) ;
#28453 = ADVANCED_FACE ( 'NONE', ( #12678 ), #18482, .T. ) ;
#28454 = DIRECTION ( 'NONE',  ( 0.9510565162951535312, 2.566386769018988816E-16, -0.3090169943749475623 ) ) ;
#28455 = CARTESIAN_POINT ( 'NONE',  ( 138.6922820468854525, -1.999999999999979572, -17.92658477444275533 ) ) ;
#28456 = DIRECTION ( 'NONE',  ( -0.9510565162951536422, -2.566386769018988816E-16, -0.3090169943749472292 ) ) ;
#28457 = VECTOR ( 'NONE', #28873, 1000.000000000000000 ) ;
#28458 = LINE ( 'NONE', #28765, #24138 ) ;
#28459 = CARTESIAN_POINT ( 'NONE',  ( 12.27631119714397201, 9.497383584800669354, -15.31093738554958428 ) ) ;
#28460 = LINE ( 'NONE', #9480, #24102 ) ;
#28461 = ORIENTED_EDGE ( 'NONE', *, *, #19814, .T. ) ;
#28462 = CARTESIAN_POINT ( 'NONE',  ( -13.00000000000001243, 55.00000000000000711, -18.00000000000000000 ) ) ;
#28463 = ORIENTED_EDGE ( 'NONE', *, *, #26563, .T. ) ;
#28464 = CARTESIAN_POINT ( 'NONE',  ( 11.46775782571576130, 9.292755756535285627, -15.86302895122203616 ) ) ;
#28465 = VERTEX_POINT ( 'NONE', #3534 ) ;
#28466 = AXIS2_PLACEMENT_3D ( 'NONE', #12297, #21612, #21464 ) ;
#28467 = CARTESIAN_POINT ( 'NONE',  ( 19.45720675144774603, -0.6714082060231494342, -20.03460252700725519 ) ) ;
#28468 = CARTESIAN_POINT ( 'NONE',  ( 149.5152310637605808, -1.999999999999975353, -30.37205893520531319 ) ) ;
#28469 = CARTESIAN_POINT ( 'NONE',  ( 79.48924668973215546, -4.999999999999995559, 57.75231823919976648 ) ) ;
#28470 = FACE_OUTER_BOUND ( 'NONE', #19107, .T. ) ;
#28471 = ORIENTED_EDGE ( 'NONE', *, *, #8623, .T. ) ;
#28472 = DIRECTION ( 'NONE',  ( -2.207829878515935943E-16, 1.000000000000000000, 0.000000000000000000 ) ) ;
#28473 = CARTESIAN_POINT ( 'NONE',  ( 11.28421916535349112, 16.64009977454265865, -16.78120545242191142 ) ) ;
#28474 = ORIENTED_EDGE ( 'NONE', *, *, #7665, .T. ) ;
#28475 = CARTESIAN_POINT ( 'NONE',  ( 33.59450136257035524, -12.41883169790769692, -18.71738141962731561 ) ) ;
#28476 = CARTESIAN_POINT ( 'NONE',  ( 18.47369133221681281, 7.987600538477567014, -15.27093437040897861 ) ) ;
#28477 = ORIENTED_EDGE ( 'NONE', *, *, #18902, .F. ) ;
#28478 = VERTEX_POINT ( 'NONE', #6117 ) ;
#28479 = DIRECTION ( 'NONE',  ( 0.5877852522924731371, 1.586114251531760728E-16, 0.8090169943749474513 ) ) ;
#28480 = CARTESIAN_POINT ( 'NONE',  ( 9.116630548627156827, 16.16256849206635238, -17.05302909012592494 ) ) ;
#28481 = CARTESIAN_POINT ( 'NONE',  ( 28.41550859958678643, -4.728095322062062067, -17.81194336819277524 ) ) ;
#28482 = ORIENTED_EDGE ( 'NONE', *, *, #3371, .F. ) ;
#28483 = CARTESIAN_POINT ( 'NONE',  ( 168.6922820468853104, -1.999999999999971800, -9.266330736598359152 ) ) ;
#28484 = CARTESIAN_POINT ( 'NONE',  ( 18.39996379557756256, 0.6904185378075045065, -15.43317298867526866 ) ) ;
#28485 = CARTESIAN_POINT ( 'NONE',  ( 15.41580380672748163, 5.935325531760808460, -16.22756139702874023 ) ) ;
#28486 = ORIENTED_EDGE ( 'NONE', *, *, #16936, .F. ) ;
#28487 = LINE ( 'NONE', #2259, #3557 ) ;
#28488 = ORIENTED_EDGE ( 'NONE', *, *, #9998, .F. ) ;
#28489 = ORIENTED_EDGE ( 'NONE', *, *, #20237, .T. ) ;
#28490 = LINE ( 'NONE', #28634, #27828 ) ;
#28491 = EDGE_CURVE ( 'NONE', #10208, #19917, #28763, .T. ) ;
#28492 = AXIS2_PLACEMENT_3D ( 'NONE', #10909, #17772, #10455 ) ;
#28493 = EDGE_CURVE ( 'NONE', #3119, #379, #17401, .T. ) ;
#28494 = ADVANCED_FACE ( 'NONE', ( #26441 ), #15260, .T. ) ;
#28495 = DIRECTION ( 'NONE',  ( -1.110223024625156540E-16, 0.000000000000000000, -1.000000000000000000 ) ) ;
#28496 = ADVANCED_FACE ( 'NONE', ( #3245 ), #24838, .T. ) ;
#28497 = DIRECTION ( 'NONE',  ( -0.5877852522924731371, -1.586114251531760728E-16, -0.8090169943749474513 ) ) ;
#28498 = CARTESIAN_POINT ( 'NONE',  ( 173.6922820468853104, -9.999999999999994671, -15.07341522555727664 ) ) ;
#28499 = DIRECTION ( 'NONE',  ( 0.5877852522924731371, 1.586114251531760728E-16, 0.8090169943749474513 ) ) ;
#28500 = CARTESIAN_POINT ( 'NONE',  ( 9.649959050778257108, 17.62941265384766254, -17.56860460898032628 ) ) ;
#28501 = CARTESIAN_POINT ( 'NONE',  ( 26.72351632055398696, -11.69804524575189397, -15.34103589027250791 ) ) ;
#28502 = CARTESIAN_POINT ( 'NONE',  ( 22.90957683611224738, 2.308586283387667581, -16.61139769879808625 ) ) ;
#28504 = ORIENTED_EDGE ( 'NONE', *, *, #28493, .T. ) ;
#28503 = CARTESIAN_POINT ( 'NONE',  ( 35.05385823632300912, -20.96193052275466329, -21.15110683048779805 ) ) ;
#28505 = CARTESIAN_POINT ( 'NONE',  ( 180.7287565553229740, -84.33034373659253902, 0.5000000000000029976 ) ) ;
#28506 = CARTESIAN_POINT ( 'NONE',  ( 15.61762486822808604, 9.948436389806387226, -12.64537296286936829 ) ) ;
#28507 = LINE ( 'NONE', #12423, #14189 ) ;
#28508 = LINE ( 'NONE', #11966, #14126 ) ;
#28509 = CARTESIAN_POINT ( 'NONE',  ( 16.57956996521092918, 4.788269978297743812, -19.71382457362092566 ) ) ;
#28510 = ORIENTED_EDGE ( 'NONE', *, *, #24561, .F. ) ;
#28511 = CARTESIAN_POINT ( 'NONE',  ( 133.6922820468854241, -1.999999999999981348, -26.58683881228715506 ) ) ;
#28512 = CARTESIAN_POINT ( 'NONE',  ( 10.33841720888800531, 18.38481243897025053, -17.83974501271621449 ) ) ;
#28513 = CARTESIAN_POINT ( 'NONE',  ( 169.7287565553228887, -9.999999999999998224, -7.839745962155603820 ) ) ;
#28514 = PLANE ( 'NONE',  #27889 ) ;
#28515 = CARTESIAN_POINT ( 'NONE',  ( 19.52227536296714305, 7.868296793410291201, -18.00468392081665669 ) ) ;
#28516 = VECTOR ( 'NONE', #903, 999.9999999999998863 ) ;
#28517 = CARTESIAN_POINT ( 'NONE',  ( 28.46611200899306127, -11.40119892829609327, -11.67154496650716666 ) ) ;
#28518 = EDGE_LOOP ( 'NONE', ( #3842, #20515, #920, #23237 ) ) ;
#28519 = CARTESIAN_POINT ( 'NONE',  ( 35.03938282813840743, -19.89690018161999419, -20.20402626681843117 ) ) ;
#28520 = CARTESIAN_POINT ( 'NONE',  ( 21.68595642006795288, -3.720678421232956445, -15.48850127590278980 ) ) ;
#28521 = CARTESIAN_POINT ( 'NONE',  ( 19.13053735399196142, -0.4946192386601480084, -18.78456443592403602 ) ) ;
#28522 = VERTEX_POINT ( 'NONE', #7807 ) ;
#28523 = CARTESIAN_POINT ( 'NONE',  ( 26.51887141003594195, -6.641914482010843557, -12.47546034222045819 ) ) ;
#28524 = EDGE_CURVE ( 'NONE', #11088, #28371, #17113, .T. ) ;
#28525 = ORIENTED_EDGE ( 'NONE', *, *, #17481, .F. ) ;
#28526 = EDGE_CURVE ( 'NONE', #5542, #6718, #24589, .T. ) ;
#28527 = DIRECTION ( 'NONE',  ( -0.8090169943749474513, -2.183098979609982436E-16, -0.5877852522924731371 ) ) ;
#28528 = ADVANCED_FACE ( 'NONE', ( #10234 ), #10692, .T. ) ;
#28529 = CARTESIAN_POINT ( 'NONE',  ( 131.1922820468854241, -10.00000000000000888, -4.936203717676158398 ) ) ;
#28530 = FACE_OUTER_BOUND ( 'NONE', #12968, .T. ) ;
#28531 = AXIS2_PLACEMENT_3D ( 'NONE', #25752, #4681, #23306 ) ;
#28532 = CARTESIAN_POINT ( 'NONE',  ( 119.9999999999999858, -30.00000000000000000, -17.99999999999998934 ) ) ;
#28533 = CARTESIAN_POINT ( 'NONE',  ( 35.28777801271252912, -15.52033788203570985, -19.16652784865743442 ) ) ;
#28534 = CARTESIAN_POINT ( 'NONE',  ( 12.75811015101040446, 7.626735917299793499, -14.92445666636202617 ) ) ;
#28535 = DIRECTION ( 'NONE',  ( -2.698458740408365879E-16, 1.000000000000000000, 0.000000000000000000 ) ) ;
#28536 = CARTESIAN_POINT ( 'NONE',  ( 98.70167508945917234, -4.999999999999990230, 71.71096453785942515 ) ) ;
#28537 = CARTESIAN_POINT ( 'NONE',  ( 12.26413032053702779, 8.815164712426300397, -16.54932944099246228 ) ) ;
#28538 = CARTESIAN_POINT ( 'NONE',  ( -11.85189716074913058, -5.341585316273319783, 9.999999999999998224 ) ) ;
#28539 = PLANE ( 'NONE',  #12024 ) ;
#28540 = VERTEX_POINT ( 'NONE', #25048 ) ;
#28541 = DIRECTION ( 'NONE',  ( -2.698458740408365879E-16, 1.000000000000000000, 0.000000000000000000 ) ) ;
#28542 = DIRECTION ( 'NONE',  ( 0.000000000000000000, 0.000000000000000000, 1.000000000000000000 ) ) ;
#28543 = ORIENTED_EDGE ( 'NONE', *, *, #14988, .F. ) ;
#28544 = ORIENTED_EDGE ( 'NONE', *, *, #22070, .F. ) ;
#28545 = CARTESIAN_POINT ( 'NONE',  ( 11.22494245711612848, 9.086454032755447940, -17.24116976563960435 ) ) ;
#28546 = EDGE_CURVE ( 'NONE', #29924, #17091, #12155, .T. ) ;
#28547 = CARTESIAN_POINT ( 'NONE',  ( 23.18962843369624949, -6.128656054388458507, -17.19981796389819095 ) ) ;
#28548 = CARTESIAN_POINT ( 'NONE',  ( 23.72517123929712213, -5.798560033841243744, -19.46542475990168342 ) ) ;
#28549 = CARTESIAN_POINT ( 'NONE',  ( 162.2287565553229456, -9.999999999999998224, -20.83012701892220520 ) ) ;
#28550 = LINE ( 'NONE', #17064, #14047 ) ;
#28551 = CIRCLE ( 'NONE', #29530, 4.250000000000000000 ) ;
#28552 = LINE ( 'NONE', #11722, #598 ) ;
#28553 = VERTEX_POINT ( 'NONE', #13729 ) ;
#28554 = LINE ( 'NONE', #12179, #28951 ) ;
#28555 = FACE_OUTER_BOUND ( 'NONE', #21011, .T. ) ;
#28556 = PLANE ( 'NONE',  #16013 ) ;
#28557 = ADVANCED_FACE ( 'NONE', ( #18006 ), #20595, .T. ) ;
#28558 = PLANE ( 'NONE',  #6864 ) ;
#28559 = LINE ( 'NONE', #24101, #29989 ) ;
#28560 = CARTESIAN_POINT ( 'NONE',  ( 10.47262648896379922, 16.44941058625191133, -17.33455387760982447 ) ) ;
#28561 = CARTESIAN_POINT ( 'NONE',  ( 164.7287565553228887, -1.999999999999972244, -7.839745962155603820 ) ) ;
#28562 = PLANE ( 'NONE',  #10699 ) ;
#28563 = ORIENTED_EDGE ( 'NONE', *, *, #2108, .F. ) ;
#28564 = CARTESIAN_POINT ( 'NONE',  ( 13.37514969516658070, 7.623989538026159529, -15.71142857098959489 ) ) ;
#28565 = FACE_OUTER_BOUND ( 'NONE', #17740, .T. ) ;
#28566 = AXIS2_PLACEMENT_3D ( 'NONE', #790, #2793, #19394 ) ;
#28567 = CARTESIAN_POINT ( 'NONE',  ( 20.99533150354982070, 4.487273811465053441, -19.54336078777620500 ) ) ;
#28568 = CARTESIAN_POINT ( 'NONE',  ( 12.86616790684404421, 9.515247448762703897, -16.11708638872277177 ) ) ;
#28569 = CARTESIAN_POINT ( 'NONE',  ( 148.6922820468854525, -1.999999999999975797, -23.73366926340167637 ) ) ;
#28570 = VERTEX_POINT ( 'NONE', #6883 ) ;
#28571 = ORIENTED_EDGE ( 'NONE', *, *, #25754, .T. ) ;
#28572 = CARTESIAN_POINT ( 'NONE',  ( 9.997747326010761881, 16.03441129093729245, -16.47093000352221637 ) ) ;
#28573 = FACE_OUTER_BOUND ( 'NONE', #24322, .T. ) ;
#28574 = CARTESIAN_POINT ( 'NONE',  ( 9.916824447075894611, 16.40553392900050156, -16.50439446175997205 ) ) ;
#28575 = DIRECTION ( 'NONE',  ( -0.000000000000000000, -0.000000000000000000, 1.000000000000000000 ) ) ;
#28576 = VERTEX_POINT ( 'NONE', #20737 ) ;
#28577 = CARTESIAN_POINT ( 'NONE',  ( 136.1922820468854241, -4.999999999999981348, -30.91696583120935671 ) ) ;
#28578 = ORIENTED_EDGE ( 'NONE', *, *, #13651, .T. ) ;
#28579 = CARTESIAN_POINT ( 'NONE',  ( 13.11546866977305825, 8.567317423965196355, -15.91839467484043880 ) ) ;
#28580 = EDGE_CURVE ( 'NONE', #24253, #16928, #4133, .T. ) ;
#28581 = ORIENTED_EDGE ( 'NONE', *, *, #861, .T. ) ;
#28582 = CARTESIAN_POINT ( 'NONE',  ( 33.60507142094932931, -10.68002793468083134, -20.32431474444524255 ) ) ;
#28583 = CARTESIAN_POINT ( 'NONE',  ( 16.78426473046523526, 10.16049046829612479, -19.50779498702920378 ) ) ;
#28584 = CARTESIAN_POINT ( 'NONE',  ( 29.62588713853392264, -10.65184931322849060, -12.76488833982454629 ) ) ;
#28585 = ADVANCED_FACE ( 'NONE', ( #16016 ), #13426, .T. ) ;
#28586 = ORIENTED_EDGE ( 'NONE', *, *, #4234, .T. ) ;
#28587 = VECTOR ( 'NONE', #22118, 1000.000000000000000 ) ;
#28588 = CARTESIAN_POINT ( 'NONE',  ( 139.7287565553230024, -10.00000000000000533, 0.8205080756887930260 ) ) ;
#28589 = ORIENTED_EDGE ( 'NONE', *, *, #7941, .T. ) ;
#28590 = VERTEX_POINT ( 'NONE', #24900 ) ;
#28591 = CARTESIAN_POINT ( 'NONE',  ( 142.2287565553230309, -10.00000000000000533, -20.83012701892220164 ) ) ;
#28592 = CARTESIAN_POINT ( 'NONE',  ( 18.08386662754633534, 1.890959213400748684, -17.98613275626550134 ) ) ;
#28593 = VECTOR ( 'NONE', #8032, 1000.000000000000000 ) ;
#28594 = CARTESIAN_POINT ( 'NONE',  ( 28.49100808714443289, -10.93160309251996765, -13.65156567797833631 ) ) ;
#28595 = COLOUR_RGB ( '', 0.66274510, 0.83137255, 0.94901961) ;
#28596 = CARTESIAN_POINT ( 'NONE',  ( 156.1922820468854241, -1.999999999999974021, -30.91696583120936026 ) ) ;
#28597 = CARTESIAN_POINT ( 'NONE',  ( 164.5152310637604671, -1.999999999999972244, -13.05155085951651195 ) ) ;
#28598 = DIRECTION ( 'NONE',  ( -2.698458740408365879E-16, 1.000000000000000000, 0.000000000000000000 ) ) ;
#28599 = LINE ( 'NONE', #21235, #9693 ) ;
#28600 = DIRECTION ( 'NONE',  ( 0.5877852522924731371, 0.000000000000000000, 0.8090169943749474513 ) ) ;
#28601 = VECTOR ( 'NONE', #17022, 1000.000000000000000 ) ;
#28602 = CARTESIAN_POINT ( 'NONE',  ( 12.27690927615027583, 9.494639109526119114, -15.31069018153633721 ) ) ;
#28603 = DIRECTION ( 'NONE',  ( 0.000000000000000000, 0.000000000000000000, 1.000000000000000000 ) ) ;
#28604 = CARTESIAN_POINT ( 'NONE',  ( 84.03026872336096176, -4.999999999999994671, 61.05156386724048190 ) ) ;
#28605 = ORIENTED_EDGE ( 'NONE', *, *, #4697, .F. ) ;
#28606 = VECTOR ( 'NONE', #7858, 1000.000000000000000 ) ;
#28607 = CARTESIAN_POINT ( 'NONE',  ( 12.47535353872619446, 8.560407331872438519, -15.14977315560688176 ) ) ;
#28608 = ORIENTED_EDGE ( 'NONE', *, *, #6640, .T. ) ;
#28609 = CARTESIAN_POINT ( 'NONE',  ( 18.31109272121128484, -1.763409964857557188, -18.37077502410619090 ) ) ;
#28610 = FACE_OUTER_BOUND ( 'NONE', #25819, .T. ) ;
#28611 = SURFACE_STYLE_FILL_AREA ( #25999 ) ;
#28612 = LINE ( 'NONE', #2456, #28306 ) ;
#28613 = EDGE_LOOP ( 'NONE', ( #222, #22853, #1980, #27521 ) ) ;
#28614 = FACE_OUTER_BOUND ( 'NONE', #6118, .T. ) ;
#28615 = CARTESIAN_POINT ( 'NONE',  ( 12.84801357566967717, 9.517348710814296453, -16.13078356789775469 ) ) ;
#28616 = EDGE_CURVE ( 'NONE', #15678, #8129, #6274, .T. ) ;
#28617 = ORIENTED_EDGE ( 'NONE', *, *, #14577, .F. ) ;
#28618 = EDGE_CURVE ( 'NONE', #11106, #11337, #22603, .T. ) ;
#28619 = CARTESIAN_POINT ( 'NONE',  ( 35.54686456755326418, -21.17674681625933530, -18.46270299499373735 ) ) ;
#28620 = CARTESIAN_POINT ( 'NONE',  ( 15.44629794785920218, 3.545610805586186132, -16.71614555938632307 ) ) ;
#28621 = EDGE_CURVE ( 'NONE', #2945, #23086, #6724, .T. ) ;
#28622 = DIRECTION ( 'NONE',  ( 1.110223024625156540E-16, 2.995891024602366092E-32, 1.000000000000000000 ) ) ;
#28623 = EDGE_CURVE ( 'NONE', #23153, #11088, #14584, .T. ) ;
#28624 = CARTESIAN_POINT ( 'NONE',  ( 27.18523481531828168, -13.05407500640787077, -12.66260957699712186 ) ) ;
#28625 = VERTEX_POINT ( 'NONE', #8845 ) ;
#28626 = DIRECTION ( 'NONE',  ( 1.000000000000000000, 0.000000000000000000, 0.000000000000000000 ) ) ;
#28627 = CARTESIAN_POINT ( 'NONE',  ( 24.00718893345771932, -1.002666751694005765, -18.91818096615087796 ) ) ;
#28628 = CARTESIAN_POINT ( 'NONE',  ( 18.26355027798676645, 7.143056880744947712, -15.77244846760033958 ) ) ;
#28629 = AXIS2_PLACEMENT_3D ( 'NONE', #10897, #13045, #20211 ) ;
#28630 = VERTEX_POINT ( 'NONE', #27518 ) ;
#28631 = DIRECTION ( 'NONE',  ( -0.8090169943749474513, -2.183098979609982436E-16, -0.5877852522924731371 ) ) ;
#28632 = ORIENTED_EDGE ( 'NONE', *, *, #8980, .T. ) ;
#28633 = ORIENTED_EDGE ( 'NONE', *, *, #4499, .F. ) ;
#28634 = CARTESIAN_POINT ( 'NONE',  ( 5.351309945704854520, -5.000000000000015987, 16.46963852221801972 ) ) ;
#28635 = AXIS2_PLACEMENT_3D ( 'NONE', #11931, #4931, #11786 ) ;
#28636 = APPLICATION_CONTEXT ( 'automotive_design' ) ;
#28637 = VECTOR ( 'NONE', #2198, 1000.000000000000000 ) ;
#28638 = LINE ( 'NONE', #7689, #9405 ) ;
#28639 = DIRECTION ( 'NONE',  ( 0.5877852522924731371, 0.000000000000000000, 0.8090169943749474513 ) ) ;
#28640 = VECTOR ( 'NONE', #12558, 1000.000000000000000 ) ;
#28641 = CARTESIAN_POINT ( 'NONE',  ( 134.5152310637605524, -4.999999999999981348, -13.05155085951650840 ) ) ;
#28642 = CARTESIAN_POINT ( 'NONE',  ( 172.7287565553229456, -1.999999999999970468, -39.49999999999997868 ) ) ;
#28643 = CARTESIAN_POINT ( 'NONE',  ( 11.47304865262203499, 9.268493388164605662, -15.86084085272616484 ) ) ;
#28644 = CARTESIAN_POINT ( 'NONE',  ( 26.45169718342334164, -9.008644514675534509, -18.11399877363951205 ) ) ;
#28645 = CARTESIAN_POINT ( 'NONE',  ( 21.00058363250239069, -3.857595149258782996, -18.17417979037076847 ) ) ;
#28646 = EDGE_CURVE ( 'NONE', #2890, #7231, #6575, .T. ) ;
#28648 = ORIENTED_EDGE ( 'NONE', *, *, #27520, .F. ) ;
#28647 = CARTESIAN_POINT ( 'NONE',  ( 32.36240160181304759, -11.00785621467150044, -17.57054915585148436 ) ) ;
#28649 = DIRECTION ( 'NONE',  ( 2.698458740408365879E-16, -1.000000000000000000, 0.000000000000000000 ) ) ;
#28650 = CARTESIAN_POINT ( 'NONE',  ( 154.7287565553230024, -10.00000000000000000, -25.16025403784440329 ) ) ;
#28651 = CARTESIAN_POINT ( 'NONE',  ( 1.214306433183764966E-14, 4.618802153517016507, -2.092734410091829034 ) ) ;
#28652 = DIRECTION ( 'NONE',  ( 0.3090169943749475623, 8.338696094058001131E-17, 0.9510565162951536422 ) ) ;
#28653 = STYLED_ITEM ( 'NONE', ( #18020 ), #11840 ) ;
#28654 = DIRECTION ( 'NONE',  ( 0.000000000000000000, 0.000000000000000000, -1.000000000000000000 ) ) ;
#28655 = DIRECTION ( 'NONE',  ( -0.5877852522924731371, -1.586114251531760235E-16, 0.8090169943749474513 ) ) ;
#28656 = CARTESIAN_POINT ( 'NONE',  ( 19.07848178107829540, -2.338951347401693859, -17.85627120065723616 ) ) ;
#28657 = ORIENTED_EDGE ( 'NONE', *, *, #26363, .F. ) ;
#28658 = DIRECTION ( 'NONE',  ( 0.9510565162951536422, 0.000000000000000000, -0.3090169943749475623 ) ) ;
#28659 = CARTESIAN_POINT ( 'NONE',  ( 10.72091424521701519, 16.63063227333373462, -15.95414859203816782 ) ) ;
#28660 = VECTOR ( 'NONE', #17717, 1000.000000000000000 ) ;
#28661 = DIRECTION ( 'NONE',  ( -1.110223024625156540E-16, 0.000000000000000000, -1.000000000000000000 ) ) ;
#28662 = DIRECTION ( 'NONE',  ( 0.000000000000000000, 0.000000000000000000, 1.000000000000000000 ) ) ;
#28663 = ADVANCED_FACE ( 'NONE', ( #1700 ), #8985, .T. ) ;
#28664 = CARTESIAN_POINT ( 'NONE',  ( 19.07848178107829540, -2.338951347401693859, -17.85627120065723616 ) ) ;
#28665 = EDGE_CURVE ( 'NONE', #10103, #9448, #2012, .T. ) ;
#28666 = ADVANCED_FACE ( 'NONE', ( #11429 ), #18306, .F. ) ;
#28667 = CARTESIAN_POINT ( 'NONE',  ( 14.35528768574272895, 10.45889919667044410, -14.17515447063821910 ) ) ;
#28668 = ORIENTED_EDGE ( 'NONE', *, *, #1895, .F. ) ;
#28669 = CARTESIAN_POINT ( 'NONE',  ( 33.17819505895439391, -11.78846528140086924, -19.49437495119144259 ) ) ;
#28670 = VERTEX_POINT ( 'NONE', #25342 ) ;
#28671 = CARTESIAN_POINT ( 'NONE',  ( 28.52362724998032917, -7.841767518281756111, -12.14325827080317666 ) ) ;
#28672 = CARTESIAN_POINT ( 'NONE',  ( 18.53362878050275597, 1.800236982614616510, -15.18126852959267481 ) ) ;
#28673 = ORIENTED_EDGE ( 'NONE', *, *, #17041, .F. ) ;
#28674 = VERTEX_POINT ( 'NONE', #4432 ) ;
#28675 = VECTOR ( 'NONE', #28131, 1000.000000000000000 ) ;
#28676 = DIRECTION ( 'NONE',  ( 0.9510565162951535312, 2.566386769018988816E-16, -0.3090169943749475623 ) ) ;
#28677 = CARTESIAN_POINT ( 'NONE',  ( 144.5152310637605808, -1.999999999999977129, -21.71180489736091346 ) ) ;
#28678 = CIRCLE ( 'NONE', #15470, 4.000000000000000000 ) ;
#28679 = LINE ( 'NONE', #3759, #28197 ) ;
#28680 = DIRECTION ( 'NONE',  ( 0.3090169943749472292, 8.338696094057992503E-17, -0.9510565162951536422 ) ) ;
#28681 = CARTESIAN_POINT ( 'NONE',  ( -20.00000000000017053, 34.64101615137744972, 0.000000000000000000 ) ) ;
#28682 = CARTESIAN_POINT ( 'NONE',  ( 36.54859390953724585, -22.18451583373416014, -18.19919658220850778 ) ) ;
#28683 = CARTESIAN_POINT ( 'NONE',  ( 9.641350810849047548, 17.66889113945805789, -17.91664992932186351 ) ) ;
#28684 = CARTESIAN_POINT ( 'NONE',  ( 157.2287565553230024, -1.999999999999973133, -29.49038105676660493 ) ) ;
#28685 = DIRECTION ( 'NONE',  ( -0.9510565162951536422, -2.566386769018988816E-16, -0.3090169943749472292 ) ) ;
#28686 = CARTESIAN_POINT ( 'NONE',  ( 12.02406503409520333, 9.334315655862766903, -16.69297946412503819 ) ) ;
#28687 = DIRECTION ( 'NONE',  ( -0.000000000000000000, -0.000000000000000000, -1.000000000000000000 ) ) ;
#28688 = FACE_BOUND ( 'NONE', #17146, .T. ) ;
#28689 = VERTEX_POINT ( 'NONE', #18464 ) ;
#28690 = EDGE_LOOP ( 'NONE', ( #10849, #28617, #11524, #22477 ) ) ;
#28691 = FACE_OUTER_BOUND ( 'NONE', #8736, .T. ) ;
#28692 = CARTESIAN_POINT ( 'NONE',  ( -2.681483223904232549, 3.070647092368427256, -2.450000000000005063 ) ) ;
#28693 = ADVANCED_FACE ( 'NONE', ( #10984 ), #27816, .T. ) ;
#28694 = EDGE_CURVE ( 'NONE', #22122, #9309, #23193, .T. ) ;
#28695 = VECTOR ( 'NONE', #25956, 1000.000000000000000 ) ;
#28696 = CARTESIAN_POINT ( 'NONE',  ( 120.0000000000000000, 20.00000000000000355, -15.00000000000000000 ) ) ;
#28697 = ORIENTED_EDGE ( 'NONE', *, *, #21341, .T. ) ;
#28698 = VERTEX_POINT ( 'NONE', #19206 ) ;
#28699 = ADVANCED_FACE ( 'NONE', ( #4722 ), #28562, .T. ) ;
#28700 = ORIENTED_EDGE ( 'NONE', *, *, #16094, .T. ) ;
#28701 = EDGE_CURVE ( 'NONE', #9311, #10747, #311, .T. ) ;
#28702 = CARTESIAN_POINT ( 'NONE',  ( 11.40026617402801179, 8.559985368287675200, -17.14749594687102174 ) ) ;
#28703 = VECTOR ( 'NONE', #6449, 1000.000000000000000 ) ;
#28704 = CARTESIAN_POINT ( 'NONE',  ( 24.36960067559809318, -5.041758482997499513, -18.26785210147486538 ) ) ;
#28705 = CARTESIAN_POINT ( 'NONE',  ( 21.00058363250239069, -3.857595149258782996, -18.17417979037076847 ) ) ;
#28706 = CARTESIAN_POINT ( 'NONE',  ( 149.7287565553230024, -1.999999999999975797, -16.50000000000000355 ) ) ;
#28707 = CARTESIAN_POINT ( 'NONE',  ( 174.7287565553228603, -9.999999999999996447, -7.839745962155603820 ) ) ;
#28708 = LINE ( 'NONE', #7756, #21567 ) ;
#28709 = CARTESIAN_POINT ( 'NONE',  ( 130.7287565553229456, -4.999999999999983125, 3.500000000000003109 ) ) ;
#28710 = LINE ( 'NONE', #19503, #28457 ) ;
#28711 = CARTESIAN_POINT ( 'NONE',  ( 141.1922820468854525, -10.00000000000000533, -13.59645775552055902 ) ) ;
#28712 = VECTOR ( 'NONE', #1083, 1000.000000000000000 ) ;
#28713 = CARTESIAN_POINT ( 'NONE',  ( 148.6922820468854525, -1.999999999999976241, -26.58683881228715862 ) ) ;
#28714 = LINE ( 'NONE', #12638, #28516 ) ;
#28715 = CARTESIAN_POINT ( 'NONE',  ( 12.02558468657594659, 9.327346335875439820, -16.69235103436730938 ) ) ;
#28716 = DIRECTION ( 'NONE',  ( 0.5877852522924731371, 1.586114251531760728E-16, 0.8090169943749474513 ) ) ;
#28717 = CARTESIAN_POINT ( 'NONE',  ( 33.76744293605320024, -13.18274801178271005, -18.77722780292321758 ) ) ;
#28718 = VECTOR ( 'NONE', #6715, 1000.000000000000000 ) ;
#28719 = ORIENTED_EDGE ( 'NONE', *, *, #20740, .F. ) ;
#28720 = CARTESIAN_POINT ( 'NONE',  ( 17.72817910449685996, 9.547663288818908356, -12.24198789229035533 ) ) ;
#28721 = DIRECTION ( 'NONE',  ( 1.000000000000000000, 2.698458740408365879E-16, -1.110223024625156540E-16 ) ) ;
#28722 = CARTESIAN_POINT ( 'NONE',  ( 22.34083945069921739, -4.755659482961629436, -14.12236044035638116 ) ) ;
#28723 = CARTESIAN_POINT ( 'NONE',  ( 12.84461350077944886, 9.519659821018855439, -16.13320262440205966 ) ) ;
#28724 = LINE ( 'NONE', #28426, #15061 ) ;
#28725 = VECTOR ( 'NONE', #21493, 1000.000000000000000 ) ;
#28726 = VERTEX_POINT ( 'NONE', #18915 ) ;
#28727 = ORIENTED_EDGE ( 'NONE', *, *, #17621, .F. ) ;
#28728 = VECTOR ( 'NONE', #2085, 999.9999999999998863 ) ;
#28729 = VERTEX_POINT ( 'NONE', #7323 ) ;
#28730 = CARTESIAN_POINT ( 'NONE',  ( 11.48249212886396897, 9.228508165798535501, -15.85668214399537845 ) ) ;
#28731 = DIRECTION ( 'NONE',  ( -1.000000000000000000, 0.000000000000000000, 0.000000000000000000 ) ) ;
#28732 = CARTESIAN_POINT ( 'NONE',  ( 9.949118446627077006, 16.25742953053141804, -16.49103975576934644 ) ) ;
#28733 = CARTESIAN_POINT ( 'NONE',  ( 12.98686435253176796, -5.000000000000014211, 39.96945861731516203 ) ) ;
#28734 = ORIENTED_EDGE ( 'NONE', *, *, #10861, .F. ) ;
#28735 = ADVANCED_FACE ( 'NONE', ( #21505 ), #17879, .F. ) ;
#28736 = LINE ( 'NONE', #1087, #3767 ) ;
#28737 = ORIENTED_EDGE ( 'NONE', *, *, #18589, .F. ) ;
#28738 = EDGE_CURVE ( 'NONE', #13474, #24401, #7032, .T. ) ;
#28739 = CARTESIAN_POINT ( 'NONE',  ( 12.22285885739602662, 8.868278133530205665, -16.57678160000113721 ) ) ;
#28740 = VERTEX_POINT ( 'NONE', #16323 ) ;
#28741 = CARTESIAN_POINT ( 'NONE',  ( 36.54859390953724585, -23.18451583373416014, -16.11276402859391510 ) ) ;
#28742 = CARTESIAN_POINT ( 'NONE',  ( 26.92971693216691165, -8.617903733377630715, -13.36642543767191427 ) ) ;
#28743 = CARTESIAN_POINT ( 'NONE',  ( 30.24922550192677306, -10.40856591028444278, -13.02298783260255988 ) ) ;
#28744 = ORIENTED_EDGE ( 'NONE', *, *, #9238, .F. ) ;
#28745 = LINE ( 'NONE', #26424, #18417 ) ;
#28746 = VERTEX_POINT ( 'NONE', #16022 ) ;
#28747 = ORIENTED_EDGE ( 'NONE', *, *, #13280, .F. ) ;
#28748 = ORIENTED_EDGE ( 'NONE', *, *, #26436, .F. ) ;
#28749 = CARTESIAN_POINT ( 'NONE',  ( 36.12281451779777797, -20.27171456826661355, -20.44288436412734100 ) ) ;
#28750 = APPLICATION_PROTOCOL_DEFINITION ( 'draft international standard', 'automotive_design', 1998, #3641 ) ;
#28751 = B_SPLINE_CURVE_WITH_KNOTS ( 'NONE', 3,
 ( #10238, #1253, #26294, #17561, #7813, #26913 ),
 .UNSPECIFIED., .F., .F.,
 ( 4, 2, 4 ),
 ( 2.380731629605729715E-07, 0.002336973833157549897, 0.004673709593152139234 ),
 .UNSPECIFIED. ) ;
#28752 = ORIENTED_EDGE ( 'NONE', *, *, #12858, .F. ) ;
#28753 = CARTESIAN_POINT ( 'NONE',  ( 20.29079399015155616, 4.720006093641750944, -15.95989367155712202 ) ) ;
#28754 = VECTOR ( 'NONE', #17213, 1000.000000000000000 ) ;
#28755 = CARTESIAN_POINT ( 'NONE',  ( 19.25048709941964376, 7.441878894999256921, -18.84525011105569803 ) ) ;
#28756 = ORIENTED_EDGE ( 'NONE', *, *, #8530, .T. ) ;
#28757 = TOROIDAL_SURFACE ( 'NONE', #30226, 7.000000000000000888, 2.000000000000000000 ) ;
#28758 = CARTESIAN_POINT ( 'NONE',  ( 162.0152310637604103, -1.999999999999973577, -0.06116980274991495881 ) ) ;
#28759 = LINE ( 'NONE', #1243, #28440 ) ;
#28760 = EDGE_CURVE ( 'NONE', #26011, #5942, #8994, .T. ) ;
#28761 = FACE_OUTER_BOUND ( 'NONE', #12636, .T. ) ;
#28762 = DIRECTION ( 'NONE',  ( -2.698458740408365879E-16, 1.000000000000000000, 0.000000000000000000 ) ) ;
#28763 = LINE ( 'NONE', #24748, #23856 ) ;
#28764 = PRODUCT_RELATED_PRODUCT_CATEGORY ( 'part', '', ( #15688 ) ) ;
#28765 = CARTESIAN_POINT ( 'NONE',  ( -5.000000000000000000, 0.000000000000000000, 18.00000000000000000 ) ) ;
#28766 = CARTESIAN_POINT ( 'NONE',  ( 12.27664511671607883, 9.495749246718952818, -15.31080714918738295 ) ) ;
#28767 = CARTESIAN_POINT ( 'NONE',  ( 2.500000000000000444, 2.357898499370430834, -3.469446951953614189E-15 ) ) ;
#28768 = VECTOR ( 'NONE', #28307, 1000.000000000000000 ) ;
#28769 = DIRECTION ( 'NONE',  ( 0.000000000000000000, 0.000000000000000000, -1.000000000000000000 ) ) ;
#28770 = ORIENTED_EDGE ( 'NONE', *, *, #16728, .F. ) ;
#28771 = CARTESIAN_POINT ( 'NONE',  ( 12.51417009928267099, 8.576964204390579383, -15.11888119342340353 ) ) ;
#28772 = ORIENTED_EDGE ( 'NONE', *, *, #16833, .F. ) ;
#28773 = CARTESIAN_POINT ( 'NONE',  ( 18.63699955181457923, 5.162464354397502397, -14.86688106074863569 ) ) ;
#28774 = CARTESIAN_POINT ( 'NONE',  ( 157.2287565553230024, -10.00000000000000000, -29.49038105676660493 ) ) ;
#28775 = DIRECTION ( 'NONE',  ( -2.698458740408365879E-16, 1.000000000000000000, 0.000000000000000000 ) ) ;
#28776 = DIRECTION ( 'NONE',  ( 0.000000000000000000, 0.000000000000000000, 1.000000000000000000 ) ) ;
#28777 = VECTOR ( 'NONE', #8202, 1000.000000000000000 ) ;
#28778 = EDGE_LOOP ( 'NONE', ( #24999, #22994, #4603, #25129 ) ) ;
#28779 = DIRECTION ( 'NONE',  ( 0.5877852522924731371, 1.586114251531760728E-16, 0.8090169943749474513 ) ) ;
#28780 = ORIENTED_EDGE ( 'NONE', *, *, #29830, .T. ) ;
#28781 = CARTESIAN_POINT ( 'NONE',  ( 12.83122539074939894, 9.545332027449857648, -16.14146395906381670 ) ) ;
#28782 = ORIENTED_EDGE ( 'NONE', *, *, #28881, .F. ) ;
#28783 = CARTESIAN_POINT ( 'NONE',  ( 36.41702210941816986, -20.59343343131470050, -19.35259392719279603 ) ) ;
#28784 = CARTESIAN_POINT ( 'NONE',  ( 16.34386185847872142, 4.569898679961749366, -19.52586945278800812 ) ) ;
#28785 = FACE_OUTER_BOUND ( 'NONE', #11319, .T. ) ;
#28786 = CARTESIAN_POINT ( 'NONE',  ( 25.74126694659371495, -13.30326880535473322, -17.45270501867052104 ) ) ;
#28787 = VERTEX_POINT ( 'NONE', #4140 ) ;
#28788 = DIRECTION ( 'NONE',  ( 6.938893903907227392E-16, -0.000000000000000000, 1.000000000000000000 ) ) ;
#28789 = CARTESIAN_POINT ( 'NONE',  ( 26.20148740379470453, -2.166401353139026487, -14.75472287570676322 ) ) ;
#28790 = CARTESIAN_POINT ( 'NONE',  ( 19.07173961884560498, -1.856618079973750390, -13.92706601484911033 ) ) ;
#28791 = LINE ( 'NONE', #3129, #28936 ) ;
#28792 = VERTEX_POINT ( 'NONE', #4440 ) ;
#28793 = MECHANICAL_DESIGN_GEOMETRIC_PRESENTATION_REPRESENTATION (  '', ( #2445 ), #10279 ) ;
#28794 = ORIENTED_EDGE ( 'NONE', *, *, #10347, .T. ) ;
#28795 = LINE ( 'NONE', #9506, #5964 ) ;
#28796 = AXIS2_PLACEMENT_3D ( 'NONE', #22499, #15609, #11465 ) ;
#28797 = CONICAL_SURFACE ( 'NONE', #986, 4.000000000000003553, 1.047197551196597853 ) ;
#28798 = DIRECTION ( 'NONE',  ( -0.5877852522924731371, -1.586114251531760728E-16, -0.8090169943749474513 ) ) ;
#28799 = VECTOR ( 'NONE', #27132, 1000.000000000000000 ) ;
#28800 = ADVANCED_FACE ( 'NONE', ( #2162 ), #9142, .T. ) ;
#28801 = EDGE_CURVE ( 'NONE', #29449, #21526, #22608, .T. ) ;
#28802 = CARTESIAN_POINT ( 'NONE',  ( 147.0152310637605240, -1.999999999999977573, 1.702185954127501066 ) ) ;
#28803 = DIRECTION ( 'NONE',  ( -2.698458740408365879E-16, 1.000000000000000000, 0.000000000000000000 ) ) ;
#28804 = ADVANCED_FACE ( 'NONE', ( #23658, #10049 ), #2760, .T. ) ;
#28805 = LINE ( 'NONE', #10273, #23149 ) ;
#28806 = EDGE_CURVE ( 'NONE', #19636, #9848, #9752, .T. ) ;
#28807 = CARTESIAN_POINT ( 'NONE',  ( 11.47079713067724782, 9.278817116560638567, -15.86177209170659275 ) ) ;
#28808 = CARTESIAN_POINT ( 'NONE',  ( 27.00739300205740889, -11.59555048707680847, -14.72185353022491050 ) ) ;
#28809 = CARTESIAN_POINT ( 'NONE',  ( 25.01196530022370368, -10.21768535905550124, -13.66937216179565517 ) ) ;
#28811 = ORIENTED_EDGE ( 'NONE', *, *, #7021, .T. ) ;
#28810 = CARTESIAN_POINT ( 'NONE',  ( 35.54317590287104167, -23.16017559978188345, -18.72806989825276247 ) ) ;
#28812 = DIRECTION ( 'NONE',  ( -1.000000000000000000, 0.000000000000000000, -0.000000000000000000 ) ) ;
#28813 = LINE ( 'NONE', #26489, #5307 ) ;
#28814 = CARTESIAN_POINT ( 'NONE',  ( -1.321505333908961966, 3.855830693249140406, -0.03421028094653050244 ) ) ;
#28815 = DIRECTION ( 'NONE',  ( 0.000000000000000000, -1.000000000000000000, 0.000000000000000000 ) ) ;
#28816 = LINE ( 'NONE', #15007, #6419 ) ;
#28817 = DIRECTION ( 'NONE',  ( 1.000000000000000000, 2.698458740408365879E-16, -1.110223024625156540E-16 ) ) ;
#28818 = CARTESIAN_POINT ( 'NONE',  ( 17.18819971663578272, 0.8441372818425427749, -18.45219435416397502 ) ) ;
#28819 = ORIENTED_EDGE ( 'NONE', *, *, #4537, .F. ) ;
#28820 = CARTESIAN_POINT ( 'NONE',  ( 130.7287565553229456, -9.999999999999982236, 3.500000000000003109 ) ) ;
#28821 = CARTESIAN_POINT ( 'NONE',  ( 11.75823633891744535, 11.87334092381181883, -15.52517956378672359 ) ) ;
#28822 = AXIS2_PLACEMENT_3D ( 'NONE', #28851, #12912, #7889 ) ;
#28823 = DIRECTION ( 'NONE',  ( 0.000000000000000000, 0.000000000000000000, -1.000000000000000000 ) ) ;
#28824 = DIRECTION ( 'NONE',  ( 0.3090169943749472292, 8.338696094057992503E-17, -0.9510565162951536422 ) ) ;
#28825 = CARTESIAN_POINT ( 'NONE',  ( 20.72626264887238534, -1.914771856900582714, -13.62749948506543518 ) ) ;
#28826 = CARTESIAN_POINT ( 'NONE',  ( 16.77192278198516107, 3.819237988068143075, -20.73389043596634806 ) ) ;
#28827 = EDGE_LOOP ( 'NONE', ( #19645, #7105, #29394, #915, #15960 ) ) ;
#28828 = CARTESIAN_POINT ( 'NONE',  ( 33.75544676243647757, -14.12885555826641593, -19.81592319558764004 ) ) ;
#28829 = CARTESIAN_POINT ( 'NONE',  ( 24.76964776845370864, -3.801875552749832909, -18.97459646659829247 ) ) ;
#28830 = CARTESIAN_POINT ( 'NONE',  ( 19.18059203083059217, 2.087369379035357575, -14.72322290489779917 ) ) ;
#28831 = CARTESIAN_POINT ( 'NONE',  ( 26.72358035960067824, -3.685970424986596772, -17.59444040205794835 ) ) ;
#28832 = VECTOR ( 'NONE', #7817, 1000.000000000000000 ) ;
#28833 = ORIENTED_EDGE ( 'NONE', *, *, #23807, .F. ) ;
#28834 = CARTESIAN_POINT ( 'NONE',  ( 152.0152310637605524, -4.999999999999976907, -1.687708096207002932E-14 ) ) ;
#28835 = ORIENTED_EDGE ( 'NONE', *, *, #28102, .F. ) ;
#28836 = EDGE_CURVE ( 'NONE', #10847, #23159, #25640, .T. ) ;
#28837 = VECTOR ( 'NONE', #17809, 999.9999999999998863 ) ;
#28839 = ORIENTED_EDGE ( 'NONE', *, *, #22911, .T. ) ;
#28838 = CARTESIAN_POINT ( 'NONE',  ( 134.5152310637605524, -10.00000000000000533, -4.391296821672111328 ) ) ;
#28840 = CARTESIAN_POINT ( 'NONE',  ( 125.7287565553229172, -9.999999999999982236, -33.50000000000000000 ) ) ;
#28841 = EDGE_CURVE ( 'NONE', #26554, #21526, #26258, .T. ) ;
#28842 = EDGE_CURVE ( 'NONE', #14105, #3757, #13133, .T. ) ;
#28843 = DIRECTION ( 'NONE',  ( -0.5877852522924731371, 0.000000000000000000, 0.8090169943749474513 ) ) ;
#28844 = EDGE_CURVE ( 'NONE', #28674, #25189, #7773, .T. ) ;
#28845 = CARTESIAN_POINT ( 'NONE',  ( 18.68520274485960542, 10.62608585526774441, -17.78552708330943588 ) ) ;
#28846 = CARTESIAN_POINT ( 'NONE',  ( 33.40535544545146251, -10.40465400369240356, -18.27852168438239389 ) ) ;
#28847 = CARTESIAN_POINT ( 'NONE',  ( 9.916637298967875935, 16.40639221407973380, -16.50447193873893781 ) ) ;
#28848 = LINE ( 'NONE', #15192, #21983 ) ;
#28849 = DIRECTION ( 'NONE',  ( 0.5877852522924731371, 1.586114251531760728E-16, -0.8090169943749474513 ) ) ;
#28850 = CARTESIAN_POINT ( 'NONE',  ( 13.12216094266758581, 8.570213704404382682, -15.91306547940487448 ) ) ;
#28851 = CARTESIAN_POINT ( 'NONE',  ( 133.7287565553229456, -1.999999999999988010, 0.5000000000000029976 ) ) ;
#28852 = LINE ( 'NONE', #17199, #15880 ) ;
#28853 = VECTOR ( 'NONE', #28535, 1000.000000000000000 ) ;
#28854 = ORIENTED_EDGE ( 'NONE', *, *, #6821, .F. ) ;
#28855 = AXIS2_PLACEMENT_3D ( 'NONE', #27979, #16482, #13596 ) ;
#28856 = DIRECTION ( 'NONE',  ( -0.8090169943749474513, -2.183098979609982436E-16, 0.5877852522924731371 ) ) ;
#28857 = CARTESIAN_POINT ( 'NONE',  ( 162.0152310637604671, -1.999999999999973133, -6.958068083716895558 ) ) ;
#28858 = ORIENTED_EDGE ( 'NONE', *, *, #11995, .T. ) ;
#28859 = CARTESIAN_POINT ( 'NONE',  ( 159.5152310637604955, -1.999999999999973133, -21.71180489736091346 ) ) ;
#28860 = ORIENTED_EDGE ( 'NONE', *, *, #12933, .F. ) ;
#28861 = ORIENTED_EDGE ( 'NONE', *, *, #8153, .F. ) ;
#28862 = ORIENTED_EDGE ( 'NONE', *, *, #15518, .F. ) ;
#28863 = CARTESIAN_POINT ( 'NONE',  ( 11.22367979475099631, 9.092227732665495665, -17.24169321984975056 ) ) ;
#28864 = COLOUR_RGB ( '', 0.31764706, 0.68627451, 0.89019608) ;
#28865 = CARTESIAN_POINT ( 'NONE',  ( 29.49229018507869071, -8.391778287988243434, -19.20830874944899236 ) ) ;
#28866 = CARTESIAN_POINT ( 'NONE',  ( 22.34648740292275093, -2.602002351270185532, -19.46322174391540116 ) ) ;
#28867 = DIRECTION ( 'NONE',  ( -0.5877852522924731371, -1.586114251531760728E-16, -0.8090169943749474513 ) ) ;
#28868 = CARTESIAN_POINT ( 'NONE',  ( 103.2426971230879786, -4.999999999999989342, 75.01021016590013346 ) ) ;
#28869 = CARTESIAN_POINT ( 'NONE',  ( 139.5152310637606092, -10.00000000000000533, -11.28819510263909542 ) ) ;
#28870 = ORIENTED_EDGE ( 'NONE', *, *, #10695, .T. ) ;
#28871 = DIRECTION ( 'NONE',  ( -0.9510565162951536422, 0.000000000000000000, -0.3090169943749472292 ) ) ;
#28872 = CIRCLE ( 'NONE', #18097, 8.000000000000007105 ) ;
#28873 = DIRECTION ( 'NONE',  ( -2.698458740408365879E-16, 1.000000000000000000, 0.000000000000000000 ) ) ;
#28874 = CARTESIAN_POINT ( 'NONE',  ( 0.000000000000000000, 0.000000000000000000, 18.00000000000000000 ) ) ;
#28875 = VECTOR ( 'NONE', #15771, 1000.000000000000000 ) ;
#28876 = EDGE_CURVE ( 'NONE', #21691, #6733, #21511, .T. ) ;
#28877 = DIRECTION ( 'NONE',  ( 0.5877852522924731371, 1.586114251531760728E-16, -0.8090169943749474513 ) ) ;
#28878 = CARTESIAN_POINT ( 'NONE',  ( 144.5152310637605524, -4.999999999999978684, -2.627941064794695691 ) ) ;
#28879 = ADVANCED_FACE ( 'NONE', ( #25801 ), #11742, .T. ) ;
#28880 = EDGE_CURVE ( 'NONE', #27071, #929, #21060, .T. ) ;
#28881 = EDGE_CURVE ( 'NONE', #7141, #8863, #28724, .T. ) ;
#28882 = CARTESIAN_POINT ( 'NONE',  ( 13.12425544150138279, 8.571136816377206813, -15.91139631635614471 ) ) ;
#28883 = CARTESIAN_POINT ( 'NONE',  ( 33.64261581855389949, -12.62196589562294591, -18.73949555988700055 ) ) ;
#28884 = ORIENTED_EDGE ( 'NONE', *, *, #29866, .F. ) ;
#28885 = CARTESIAN_POINT ( 'NONE',  ( 9.115110896146415342, 16.16953781205366170, -17.05365751988364309 ) ) ;
#28886 = PRODUCT ( 'hex thin nut chamfered gradeab_iso_ISO - 4035 - M10 - N', 'hex thin nut chamfered gradeab_iso_ISO - 4035 - M10 - N', '', ( #6750 ) ) ;
#28887 = CARTESIAN_POINT ( 'NONE',  ( 24.18219217278060995, -6.970120066757704791, -14.18070892486464629 ) ) ;
#28888 = CARTESIAN_POINT ( 'NONE',  ( 12.83097211533594439, 9.546493580781078236, -16.14156869735677446 ) ) ;
#28889 = FACE_BOUND ( 'NONE', #7194, .T. ) ;
#28890 = VERTEX_POINT ( 'NONE', #618 ) ;
#28891 = VERTEX_POINT ( 'NONE', #18770 ) ;
#28892 = CARTESIAN_POINT ( 'NONE',  ( 174.5152310637604671, -4.999999999999969802, -19.94844914048349693 ) ) ;
#28893 = CARTESIAN_POINT ( 'NONE',  ( 11.47219014545126647, 9.272428573238919114, -15.86119603109536058 ) ) ;
#28894 = PLANE ( 'NONE',  #9627 ) ;
#28895 = ORIENTED_EDGE ( 'NONE', *, *, #23730, .F. ) ;
#28896 = CARTESIAN_POINT ( 'NONE',  ( 153.6922820468853388, -1.999999999999975797, 2.247092850131519715 ) ) ;
#28897 = VERTEX_POINT ( 'NONE', #14479 ) ;
#28898 = CARTESIAN_POINT ( 'NONE',  ( 11.94706930840425407, 9.687427868553587729, -16.72481990518296158 ) ) ;
#28899 = ORIENTED_EDGE ( 'NONE', *, *, #22453, .T. ) ;
#28900 = CARTESIAN_POINT ( 'NONE',  ( 14.77169846916584461, 3.272981165966227568, -18.54959716842853723 ) ) ;
#28901 = CARTESIAN_POINT ( 'NONE',  ( 27.76312469413510442, -10.32446017237915648, -18.80420148706337358 ) ) ;
#28902 = CARTESIAN_POINT ( 'NONE',  ( 154.7287565553229172, -1.999999999999975353, 0.8205080756887930260 ) ) ;
#28903 = VERTEX_POINT ( 'NONE', #752 ) ;
#28904 = CARTESIAN_POINT ( 'NONE',  ( 36.09161981528372110, -20.13157329416283048, -20.44814669990763889 ) ) ;
#28905 = CONTEXT_DEPENDENT_SHAPE_REPRESENTATION ( #8316, #23024 ) ;
#28906 = VERTEX_POINT ( 'NONE', #12046 ) ;
#28907 = CARTESIAN_POINT ( 'NONE',  ( 17.99585798733817299, 1.806717527199089401, -17.78491074480216838 ) ) ;
#28908 = CARTESIAN_POINT ( 'NONE',  ( 21.58242789233717573, 5.264303332692052528, -18.32037006577847293 ) ) ;
#28909 = CARTESIAN_POINT ( 'NONE',  ( 147.0152310637605524, -1.999999999999976685, -17.38167787843871182 ) ) ;
#28910 = EDGE_CURVE ( 'NONE', #14415, #19921, #14024, .T. ) ;
#28911 = VECTOR ( 'NONE', #4006, 1000.000000000000000 ) ;
#28912 = EDGE_CURVE ( 'NONE', #11271, #5507, #9602, .T. ) ;
#28913 = EDGE_CURVE ( 'NONE', #12691, #23292, #7478, .T. ) ;
#28914 = CARTESIAN_POINT ( 'NONE',  ( 75.00000000000000000, -1.162403506782545970E-16, 4.188000000000025480 ) ) ;
#28915 = DIRECTION ( 'NONE',  ( -1.000000000000000000, 0.000000000000000000, 0.000000000000000000 ) ) ;
#28916 = DIRECTION ( 'NONE',  ( 1.000000000000000000, 0.000000000000000000, 0.000000000000000000 ) ) ;
#28917 = CARTESIAN_POINT ( 'NONE',  ( 152.2287565553230309, -10.00000000000000178, -29.49038105676660493 ) ) ;
#28918 = CARTESIAN_POINT ( 'NONE',  ( 11.62855932722735908, 12.46805622939721836, -15.57880556977976916 ) ) ;
#28919 = LINE ( 'NONE', #26755, #9466 ) ;
#28920 = LINE ( 'NONE', #12380, #15858 ) ;
#28921 = VERTEX_POINT ( 'NONE', #7182 ) ;
#28922 = CARTESIAN_POINT ( 'NONE',  ( 12.56861602585598980, 8.601024833420110483, -15.07548682890769243 ) ) ;
#28923 = VECTOR ( 'NONE', #11911, 1000.000000000000000 ) ;
#28924 = CARTESIAN_POINT ( 'NONE',  ( 10.67817636951947868, 9.002809132723193386, -16.40714615800424880 ) ) ;
#28925 = CARTESIAN_POINT ( 'NONE',  ( 17.19644251272489299, -5.000000000000013323, -52.92520801939408415 ) ) ;
#28926 = CARTESIAN_POINT ( 'NONE',  ( 144.5152310637605524, -10.00000000000000355, -2.627941064794695691 ) ) ;
#28927 = FACE_OUTER_BOUND ( 'NONE', #2246, .T. ) ;
#28928 = FACE_OUTER_BOUND ( 'NONE', #5311, .T. ) ;
#28929 = VERTEX_POINT ( 'NONE', #16474 ) ;
#28930 = CARTESIAN_POINT ( 'NONE',  ( 12.83160530386958342, 9.543589697453029430, -16.14130685162439249 ) ) ;
#28931 = ORIENTED_EDGE ( 'NONE', *, *, #12336, .T. ) ;
#28932 = CARTESIAN_POINT ( 'NONE',  ( 33.98852084862024725, -11.13792163938717472, -17.92802646347312034 ) ) ;
#28933 = CARTESIAN_POINT ( 'NONE',  ( 19.52227536296714305, 7.868296793410291201, -18.00468392081665669 ) ) ;
#28934 = ORIENTED_EDGE ( 'NONE', *, *, #13486, .F. ) ;
#28935 = DIRECTION ( 'NONE',  ( 0.5877852522924731371, 1.586114251531760728E-16, 0.8090169943749474513 ) ) ;
#28936 = VECTOR ( 'NONE', #14537, 1000.000000000000000 ) ;
#28937 = CARTESIAN_POINT ( 'NONE',  ( 32.15747877504752950, -11.00374777879112642, -13.30332049327740052 ) ) ;
#28938 = DIRECTION ( 'NONE',  ( -1.110223024625156540E-16, 0.000000000000000000, -1.000000000000000000 ) ) ;
#28939 = ADVANCED_FACE ( 'NONE', ( #4881, #23817, #14177, #23504, #16927, #2915, #2613, #12195, #11888, #318, #7333, #21203, #12950, #29026, #6091, #8371, #26408, #19516, #911, #15387, #21813, #29501, #17375, #12646, #8064, #1218, #24720, #1372, #14923, #10357, #3807, #17678, #29344, #13098, #5645, #19973, #8215, #17231, #22427, #17085, #12801, #28889, #5945, #26720, #21965, #10664, #27034, #1530, #10501, #10813, #24565, #17526, #24263, #15230, #20121, #19813, #26881, #3654, #1079, #19661, #14770, #10202, #5792, #3360, #5488, #24113, #3212, #12490, #7921, #15074, #29179, #26558, #24413, #3508, #22116, #22263, #1833, #25460, #9107, #20710, #4551, #3961, #4107, #13705, #13552, #22729 ), #20568, .T. ) ;
#28940 =( LENGTH_UNIT ( ) NAMED_UNIT ( * ) SI_UNIT ( .MILLI., .METRE. ) );
#28941 = CARTESIAN_POINT ( 'NONE',  ( 23.74924978780510898, -3.048960050427876656, -13.27477993493952191 ) ) ;
#28942 = CARTESIAN_POINT ( 'NONE',  ( 20.14260469057294500, 4.737385465944226048, -19.07682320266127718 ) ) ;
#28943 = ORIENTED_EDGE ( 'NONE', *, *, #17654, .T. ) ;
#28944 = EDGE_LOOP ( 'NONE', ( #7488, #20695, #5197, #3424, #20767 ) ) ;
#28945 = ORIENTED_EDGE ( 'NONE', *, *, #22417, .F. ) ;
#28946 = CARTESIAN_POINT ( 'NONE',  ( 8.500000000000088818, 17.32050807568872486, -23.00000000000000000 ) ) ;
#28947 = DIRECTION ( 'NONE',  ( 0.5877852522924731371, 1.586114251531760728E-16, 0.8090169943749474513 ) ) ;
#28948 = CARTESIAN_POINT ( 'NONE',  ( -5.354491962338129518, 6.146186931204416837, -4.931901280394566989 ) ) ;
#28949 = CARTESIAN_POINT ( 'NONE',  ( 147.0152310637605524, -10.00000000000000178, -6.958068083716895558 ) ) ;
#28950 = DIRECTION ( 'NONE',  ( 1.000000000000000000, 0.000000000000000000, 0.000000000000000000 ) ) ;
#28951 = VECTOR ( 'NONE', #26705, 1000.000000000000000 ) ;
#28952 = EDGE_LOOP ( 'NONE', ( #11808, #21213, #2024, #26890, #17981 ) ) ;
#28953 = CARTESIAN_POINT ( 'NONE',  ( 11.51951884677450266, 9.108496074915260365, -15.83757232928968683 ) ) ;
#28954 = CARTESIAN_POINT ( 'NONE',  ( 28.35258904315412920, -6.370284285516064848, -14.91745349193007364 ) ) ;
#28955 = CARTESIAN_POINT ( 'NONE',  ( 24.16496757332932788, -10.42823604606268617, -16.34834267607407909 ) ) ;
#28956 = ORIENTED_EDGE ( 'NONE', *, *, #6639, .T. ) ;
#28957 = DIRECTION ( 'NONE',  ( 0.000000000000000000, 0.000000000000000000, -1.000000000000000000 ) ) ;
#28958 = DIRECTION ( 'NONE',  ( -1.000000000000000000, 0.000000000000000000, 0.000000000000000000 ) ) ;
#28959 = DIRECTION ( 'NONE',  ( 0.000000000000000000, 0.000000000000000000, -1.000000000000000000 ) ) ;
#28960 = CARTESIAN_POINT ( 'NONE',  ( -2.000000000000032863, -3.464101615137743728, 8.673617379884035472E-16 ) ) ;
#28961 = CARTESIAN_POINT ( 'NONE',  ( 132.0152310637605524, -4.999999999999982236, -1.465663491281971624E-14 ) ) ;
#28962 = DIRECTION ( 'NONE',  ( 1.000000000000000000, 0.000000000000000000, 0.000000000000000000 ) ) ;
#28964 = ORIENTED_EDGE ( 'NONE', *, *, #3481, .T. ) ;
#28963 = CARTESIAN_POINT ( 'NONE',  ( 19.68115760211910725, 3.144890361740488860, -20.29587546762095940 ) ) ;
#28965 = ORIENTED_EDGE ( 'NONE', *, *, #17073, .F. ) ;
#28966 = DIRECTION ( 'NONE',  ( 1.110223024625156540E-16, 2.995891024602366092E-32, 1.000000000000000000 ) ) ;
#28967 = CARTESIAN_POINT ( 'NONE',  ( 12.27593128402378753, 9.499125914797495795, -15.31109449298900671 ) ) ;
#28968 = VECTOR ( 'NONE', #4254, 1000.000000000000000 ) ;
#28969 = CARTESIAN_POINT ( 'NONE',  ( 33.27037009343090546, -12.05169513820189309, -19.60996450177851713 ) ) ;
#28970 = CARTESIAN_POINT ( 'NONE',  ( 147.2287565553229740, -10.00000000000000355, -3.509618943233403510 ) ) ;
#28971 = CARTESIAN_POINT ( 'NONE',  ( 24.00918528248616468, -0.5066965781341161712, -13.81223085940890627 ) ) ;
#28972 = CARTESIAN_POINT ( 'NONE',  ( 149.7287565553230309, -10.00000000000000178, -33.82050807568879947 ) ) ;
#28973 = CARTESIAN_POINT ( 'NONE',  ( 22.45977841265724351, 4.097634946112983734, -18.47195213137534964 ) ) ;
#28974 = ORIENTED_EDGE ( 'NONE', *, *, #7623, .T. ) ;
#28975 = CARTESIAN_POINT ( 'NONE',  ( 136.1922820468854241, -1.999999999999980016, -2.083034168790677043 ) ) ;
#28976 = EDGE_CURVE ( 'NONE', #24463, #4011, #23030, .T. ) ;
#28977 =( NAMED_UNIT ( * ) PLANE_ANGLE_UNIT ( ) SI_UNIT ( $, .RADIAN. ) );
#28978 = CARTESIAN_POINT ( 'NONE',  ( 31.14759003376246582, -7.259970019232452998, -15.53234487094253069 ) ) ;
#28979 = ADVANCED_FACE ( 'NONE', ( #11116 ), #8670, .T. ) ;
#28980 = CARTESIAN_POINT ( 'NONE',  ( 23.73516035876120611, -6.831976609072074602, -19.85773546425274105 ) ) ;
#28981 = AXIS2_PLACEMENT_3D ( 'NONE', #2079, #6643, #4502 ) ;
#28982 = ORIENTED_EDGE ( 'NONE', *, *, #25616, .F. ) ;
#28983 = CARTESIAN_POINT ( 'NONE',  ( 30.24922550192677306, -10.40856591028444278, -13.02298783260255988 ) ) ;
#28984 = DIRECTION ( 'NONE',  ( -0.5877852522924731371, -1.586114251531760728E-16, -0.8090169943749474513 ) ) ;
#28985 = CARTESIAN_POINT ( 'NONE',  ( -4.175000000000003375, -1.342782412479990996E-15, -0.5776712190230064436 ) ) ;
#28986 = DIRECTION ( 'NONE',  ( 0.000000000000000000, 0.000000000000000000, -1.000000000000000000 ) ) ;
#28987 = DIRECTION ( 'NONE',  ( 0.000000000000000000, 0.000000000000000000, 1.000000000000000000 ) ) ;
#28988 = CARTESIAN_POINT ( 'NONE',  ( 36.04209255463945993, -19.90907354740926394, -20.43687144983462289 ) ) ;
#28989 = CARTESIAN_POINT ( 'NONE',  ( 11.34314632229486364, 9.864239995495806212, -15.91456019135469013 ) ) ;
#28990 = AXIS2_PLACEMENT_3D ( 'NONE', #27960, #11575, #21191 ) ;
#28991 = CARTESIAN_POINT ( 'NONE',  ( 133.6922820468854241, -10.00000000000000711, -9.266330736598357376 ) ) ;
#28992 = CARTESIAN_POINT ( 'NONE',  ( 161.1922820468853388, -1.999999999999973577, -13.59645775552055902 ) ) ;
#28993 = CARTESIAN_POINT ( 'NONE',  ( 9.661883355341293722, 16.25482528653935077, -17.91547504436015004 ) ) ;
#28994 = CARTESIAN_POINT ( 'NONE',  ( 176.1922820468852819, -9.999999999999994671, -13.59645775552055902 ) ) ;
#28995 = CARTESIAN_POINT ( 'NONE',  ( 142.0152310637605808, -1.999999999999978462, -6.958068083716895558 ) ) ;
#28996 = VERTEX_POINT ( 'NONE', #17975 ) ;
#28997 = EDGE_LOOP ( 'NONE', ( #6102, #24350 ) ) ;
#28998 = DIRECTION ( 'NONE',  ( -2.698458740408365879E-16, 1.000000000000000000, 0.000000000000000000 ) ) ;
#28999 = CARTESIAN_POINT ( 'NONE',  ( -5.000000000000001776, -1.608122649676635171E-15, -5.000000000000000888 ) ) ;
#29000 = CARTESIAN_POINT ( 'NONE',  ( 147.0152310637605808, -4.999999999999977796, -26.04193191628311155 ) ) ;
#29001 = ORIENTED_EDGE ( 'NONE', *, *, #4063, .F. ) ;
#29002 = VERTEX_POINT ( 'NONE', #6850 ) ;
#29003 = CARTESIAN_POINT ( 'NONE',  ( 13.32639783386816212, 7.603689066773378968, -15.75018979827038912 ) ) ;
#29004 = ADVANCED_FACE ( 'NONE', ( #18127 ), #13840, .T. ) ;
#29005 = CARTESIAN_POINT ( 'NONE',  ( 13.18850634723077242, 6.203946520731500769, -19.20132247218941401 ) ) ;
#29006 = EDGE_CURVE ( 'NONE', #23288, #27071, #15541, .T. ) ;
#29007 = CARTESIAN_POINT ( 'NONE',  ( 25.01196530022370368, -10.21768535905550124, -13.66937216179565517 ) ) ;
#29008 = DIRECTION ( 'NONE',  ( 0.5877852522924731371, 0.000000000000000000, 0.8090169943749474513 ) ) ;
#29009 = DIRECTION ( 'NONE',  ( -1.000000000000000000, 0.000000000000000000, 0.000000000000000000 ) ) ;
#29010 = ADVANCED_FACE ( 'NONE', ( #13259 ), #15834, .T. ) ;
#29011 = CARTESIAN_POINT ( 'NONE',  ( 134.7287565553230024, -1.999999999999980460, 0.8205080756887930260 ) ) ;
#29012 = VECTOR ( 'NONE', #1481, 1000.000000000000000 ) ;
#29013 = EDGE_LOOP ( 'NONE', ( #2036, #217, #16214, #1232 ) ) ;
#29014 = LINE ( 'NONE', #26546, #638 ) ;
#29015 = LINE ( 'NONE', #5323, #10370 ) ;
#29016 = DIRECTION ( 'NONE',  ( 0.9510565162951536422, 0.000000000000000000, -0.3090169943749475623 ) ) ;
#29017 = LINE ( 'NONE', #5631, #14154 ) ;
#29018 = CARTESIAN_POINT ( 'NONE',  ( 167.0152310637604671, -9.999999999999996447, -17.38167787843871182 ) ) ;
#29019 = VECTOR ( 'NONE', #9639, 1000.000000000000000 ) ;
#29020 = CARTESIAN_POINT ( 'NONE',  ( 13.01452397926061089, 8.532813591658360508, -15.99807864679971026 ) ) ;
#29021 = CARTESIAN_POINT ( 'NONE',  ( 35.49237112349044310, -21.93193663806729887, -19.32748734164077931 ) ) ;
#29022 = ORIENTED_EDGE ( 'NONE', *, *, #23011, .F. ) ;
#29023 = CARTESIAN_POINT ( 'NONE',  ( 8.949836677108400806, 16.92750644812532457, -17.70396109330303958 ) ) ;
#29024 = CARTESIAN_POINT ( 'NONE',  ( 22.16846437878366061, -4.107540447007581363, -19.06500358040360865 ) ) ;
#29025 = CARTESIAN_POINT ( 'NONE',  ( 12.83160530386958342, 9.543589697453029430, -16.14130685162439249 ) ) ;
#29026 = FACE_BOUND ( 'NONE', #10548, .T. ) ;
#29027 = ORIENTED_EDGE ( 'NONE', *, *, #520, .T. ) ;
#29028 = ORIENTED_EDGE ( 'NONE', *, *, #20404, .F. ) ;
#29029 = CARTESIAN_POINT ( 'NONE',  ( 176.1922820468852819, -1.999999999999969580, -13.59645775552055902 ) ) ;
#29030 = CIRCLE ( 'NONE', #21183, 5.000000000000006217 ) ;
#29031 = CARTESIAN_POINT ( 'NONE',  ( 11.97192087863669663, 8.579774655713777065, -15.53257280409644991 ) ) ;
#29032 = CARTESIAN_POINT ( 'NONE',  ( 139.7287565553230309, -10.00000000000000533, -33.82050807568879947 ) ) ;
#29033 = ORIENTED_EDGE ( 'NONE', *, *, #7837, .F. ) ;
#29034 = DIRECTION ( 'NONE',  ( -0.9510565162951536422, -2.566386769018988816E-16, -0.3090169943749472292 ) ) ;
#29035 = VERTEX_POINT ( 'NONE', #29810 ) ;
#29036 = CARTESIAN_POINT ( 'NONE',  ( 12.02406503409520333, 9.334315655862766903, -16.69297946412503819 ) ) ;
#29037 = ORIENTED_EDGE ( 'NONE', *, *, #28106, .T. ) ;
#29038 = CARTESIAN_POINT ( 'NONE',  ( 15.46132241025727083, 3.192341012408233869, -14.38206433644783111 ) ) ;
#29039 = CARTESIAN_POINT ( 'NONE',  ( 17.73099166324444553, -0.3602181158183791476, -14.74723639357852178 ) ) ;
#29040 = EDGE_CURVE ( 'NONE', #22270, #11002, #1984, .T. ) ;
#29041 = CARTESIAN_POINT ( 'NONE',  ( 130.7287565553229172, -4.999999999999983125, -36.50000000000000711 ) ) ;
#29042 = ADVANCED_FACE ( 'NONE', ( #20863 ), #13401, .T. ) ;
#29043 = VERTEX_POINT ( 'NONE', #27634 ) ;
#29044 = EDGE_CURVE ( 'NONE', #24164, #16231, #4407, .T. ) ;
#29045 = EDGE_CURVE ( 'NONE', #10906, #27188, #29951, .T. ) ;
#29046 = CARTESIAN_POINT ( 'NONE',  ( 35.88208498122789791, -19.19024427843809733, -20.38849413606966010 ) ) ;
#29047 = APPLICATION_PROTOCOL_DEFINITION ( 'draft international standard', 'automotive_design', 1998, #11423 ) ;
#29048 = CARTESIAN_POINT ( 'NONE',  ( 20.14628369065288993, 2.528829491441240584, -14.55248280469624866 ) ) ;
#29049 = CARTESIAN_POINT ( 'NONE',  ( 21.64656857049893901, 5.639188926465734220, -17.17864421186117951 ) ) ;
#29050 = LINE ( 'NONE', #19835, #24690 ) ;
#29051 = FACE_OUTER_BOUND ( 'NONE', #8016, .T. ) ;
#29052 = VECTOR ( 'NONE', #315, 1000.000000000000000 ) ;
#29053 = CARTESIAN_POINT ( 'NONE',  ( 0.000000000000000000, 0.000000000000000000, -2.450000000000000622 ) ) ;
#29054 = DIRECTION ( 'NONE',  ( 0.9510565162951535312, 2.566386769018988816E-16, -0.3090169943749475623 ) ) ;
#29055 = LINE ( 'NONE', #1106, #2423 ) ;
#29056 = EDGE_LOOP ( 'NONE', ( #16642, #24766, #29022, #17417 ) ) ;
#29057 = DIRECTION ( 'NONE',  ( 0.3090169943749475623, 8.338696094058001131E-17, 0.9510565162951536422 ) ) ;
#29058 = CARTESIAN_POINT ( 'NONE',  ( 10.98017426877725811, 15.44163275732038443, -15.84693559973663035 ) ) ;
#29059 = DIRECTION ( 'NONE',  ( -2.698458740408365879E-16, 1.000000000000000000, 0.000000000000000000 ) ) ;
#29060 = CIRCLE ( 'NONE', #10007, 2.700000000000001066 ) ;
#29061 = EDGE_CURVE ( 'NONE', #1409, #13253, #1678, .T. ) ;
#29062 = VERTEX_POINT ( 'NONE', #27347 ) ;
#29063 = CARTESIAN_POINT ( 'NONE',  ( 136.1922820468854241, -1.999999999999980460, -4.936203717676158398 ) ) ;
#29064 = ORIENTED_EDGE ( 'NONE', *, *, #23846, .F. ) ;
#29065 = CARTESIAN_POINT ( 'NONE',  ( 11.58682163191119230, 8.958038730125363003, -15.79767441425272345 ) ) ;
#29066 = ORIENTED_EDGE ( 'NONE', *, *, #24880, .F. ) ;
#29067 = CARTESIAN_POINT ( 'NONE',  ( 10.66961851098191083, 9.040384230280389843, -16.41081268017797257 ) ) ;
#29068 = DIRECTION ( 'NONE',  ( 0.000000000000000000, 0.000000000000000000, 1.000000000000000000 ) ) ;
#29069 = DIRECTION ( 'NONE',  ( 0.9510565162951535312, 2.566386769018988816E-16, -0.3090169943749475623 ) ) ;
#29070 = DIRECTION ( 'NONE',  ( -1.000000000000000000, -4.440892098500622217E-16, 0.000000000000000000 ) ) ;
#29071 = ORIENTED_EDGE ( 'NONE', *, *, #17232, .F. ) ;
#29072 = CARTESIAN_POINT ( 'NONE',  ( 12.83519646890166577, 9.531778640408997916, -16.13946648208032641 ) ) ;
#29073 = VERTEX_POINT ( 'NONE', #6545 ) ;
#29075 = CARTESIAN_POINT ( 'NONE',  ( 36.00107582698698394, -18.72480711723410352, -19.38214066600889751 ) ) ;
#29074 = AXIS2_PLACEMENT_3D ( 'NONE', #1339, #19938, #26999 ) ;
#29076 = CARTESIAN_POINT ( 'NONE',  ( 21.48529164538665981, 5.106035544247377267, -18.65531623833433628 ) ) ;
#29077 = ORIENTED_EDGE ( 'NONE', *, *, #10520, .F. ) ;
#29078 = EDGE_CURVE ( 'NONE', #22429, #29689, #20267, .T. ) ;
#29079 = ORIENTED_EDGE ( 'NONE', *, *, #7573, .T. ) ;
#29080 = VECTOR ( 'NONE', #2546, 1000.000000000000000 ) ;
#29081 = LINE ( 'NONE', #15279, #8155 ) ;
#29082 = CARTESIAN_POINT ( 'NONE',  ( 30.28288205714520132, -11.65814127372701670, -12.00898047443557459 ) ) ;
#29083 = ADVANCED_FACE ( 'NONE', ( #29654 ), #15693, .F. ) ;
#29084 = EDGE_LOOP ( 'NONE', ( #23984, #13345, #9570, #27944 ) ) ;
#29085 = ADVANCED_FACE ( 'NONE', ( #25596 ), #127, .T. ) ;
#29086 = LINE ( 'NONE', #8568, #5702 ) ;
#29087 = ORIENTED_EDGE ( 'NONE', *, *, #5125, .T. ) ;
#29088 = CARTESIAN_POINT ( 'NONE',  ( 22.16683763302808430, -0.5050174593055701822, -13.96310542101677044 ) ) ;
#29089 = CARTESIAN_POINT ( 'NONE',  ( 22.85609869791697335, 3.752015377681134467, -15.55886478590537969 ) ) ;
#29090 = ORIENTED_EDGE ( 'NONE', *, *, #15689, .F. ) ;
#29091 = CARTESIAN_POINT ( 'NONE',  ( -5.000000000000000000, 0.000000000000000000, -23.00000000000000000 ) ) ;
#29092 = SHAPE_REPRESENTATION ( 'double end studs bm=1.5d_am_AM A M10X60-N', ( #13190 ), #8326 ) ;
#29093 = CARTESIAN_POINT ( 'NONE',  ( 4.000000000000008882, -6.928203230275510549, 0.000000000000000000 ) ) ;
#29094 = TOROIDAL_SURFACE ( 'NONE', #15872, 3.149999999999996358, 0.8500000000000000888 ) ;
#29095 = LINE ( 'NONE', #8134, #14763 ) ;
#29096 = DIRECTION ( 'NONE',  ( -1.000000000000000000, 2.207829878515935943E-16, 0.000000000000000000 ) ) ;
#29097 = DIRECTION ( 'NONE',  ( 0.000000000000000000, 0.7071067811865456854, 0.7071067811865493491 ) ) ;
#29098 = LINE ( 'NONE', #24627, #20694 ) ;
#29099 = CARTESIAN_POINT ( 'NONE',  ( 11.39177520167864266, 9.641221755901229429, -15.89445043910815336 ) ) ;
#29100 = CARTESIAN_POINT ( 'NONE',  ( 14.18486973814142793, 6.324582201221724098, -17.68508340245422872 ) ) ;
#29101 = CARTESIAN_POINT ( 'NONE',  ( 28.92999000670439713, -5.550862855971650411, -17.57004703619191943 ) ) ;
#29102 = ORIENTED_EDGE ( 'NONE', *, *, #20740, .T. ) ;
#29103 = FACE_OUTER_BOUND ( 'NONE', #1070, .T. ) ;
#29104 = AXIS2_PLACEMENT_3D ( 'NONE', #23269, #2379, #80 ) ;
#29105 = DIRECTION ( 'NONE',  ( -2.698458740408365879E-16, 1.000000000000000000, 0.000000000000000000 ) ) ;
#29106 = FACE_OUTER_BOUND ( 'NONE', #15917, .T. ) ;
#29107 = CARTESIAN_POINT ( 'NONE',  ( 129.5152310637605808, -1.999999999999982236, -19.94844914048349338 ) ) ;
#29108 = FACE_OUTER_BOUND ( 'NONE', #1444, .T. ) ;
#29109 = LINE ( 'NONE', #19447, #28331 ) ;
#29110 = CARTESIAN_POINT ( 'NONE',  ( 23.86551563699305234, 2.542095107771292106, -17.79649620197707094 ) ) ;
#29111 = VERTEX_POINT ( 'NONE', #19182 ) ;
#29112 = CARTESIAN_POINT ( 'NONE',  ( 13.53844545036150393, -5.000000000000014211, -41.66705068152283786 ) ) ;
#29113 = CARTESIAN_POINT ( 'NONE',  ( 12.27584558688950978, 9.498490731067679604, -15.31120835137462244 ) ) ;
#29114 = CARTESIAN_POINT ( 'NONE',  ( 31.63980255171021483, -10.89810845426378982, -15.52824638758754183 ) ) ;
#29115 = CARTESIAN_POINT ( 'NONE',  ( 167.0152310637604671, -9.999999999999998224, -6.958068083716895558 ) ) ;
#29116 = VECTOR ( 'NONE', #22850, 1000.000000000000000 ) ;
#29117 = CARTESIAN_POINT ( 'NONE',  ( 17.55424633453837302, 0.6138019359854992585, -14.89346452969079060 ) ) ;
#29118 = LINE ( 'NONE', #19602, #11073 ) ;
#29119 = CARTESIAN_POINT ( 'NONE',  ( 18.14419664895403272, 7.915595134365798202, -13.41836860846829538 ) ) ;
#29120 = ORIENTED_EDGE ( 'NONE', *, *, #26142, .F. ) ;
#29121 = ADVANCED_FACE ( 'NONE', ( #23471 ), #13986, .F. ) ;
#29122 = DIRECTION ( 'NONE',  ( -0.000000000000000000, -0.000000000000000000, -1.000000000000000000 ) ) ;
#29123 = CARTESIAN_POINT ( 'NONE',  ( 23.31581686446907398, -5.989474659622321617, -13.63887547363156827 ) ) ;
#29124 = VECTOR ( 'NONE', #16528, 1000.000000000000000 ) ;
#29125 = CARTESIAN_POINT ( 'NONE',  ( 23.96443177966278881, -0.8440764653970969089, -20.02211457469898548 ) ) ;
#29126 = CIRCLE ( 'NONE', #25676, 2.749999999999999112 ) ;
#29127 = CARTESIAN_POINT ( 'NONE',  ( 28.75197783424699693, -9.407057218516385433, -18.70835418409691542 ) ) ;
#29128 = PLANE ( 'NONE',  #8934 ) ;
#29129 = EDGE_LOOP ( 'NONE', ( #8311, #26385, #12360, #18199 ) ) ;
#29130 = CARTESIAN_POINT ( 'NONE',  ( 142.0152310637605808, -4.999999999999979572, -1.576685793744487594E-14 ) ) ;
#29131 = CARTESIAN_POINT ( 'NONE',  ( 148.6922820468854525, -10.00000000000000178, -26.58683881228715862 ) ) ;
#29132 = LINE ( 'NONE', #15646, #9451 ) ;
#29133 = VECTOR ( 'NONE', #13341, 1000.000000000000000 ) ;
#29134 = CARTESIAN_POINT ( 'NONE',  ( 13.76974871631934860, 5.358497188706473402, -17.46738557873778674 ) ) ;
#29135 = EDGE_CURVE ( 'NONE', #1558, #10211, #16285, .T. ) ;
#29136 = CARTESIAN_POINT ( 'NONE',  ( 34.52681913409613657, -13.10175273156466069, -19.97882978310374469 ) ) ;
#29137 = VECTOR ( 'NONE', #921, 1000.000000000000000 ) ;
#29138 = CARTESIAN_POINT ( 'NONE',  ( 11.44040408106239326, 9.418203516307107392, -15.87434068686103394 ) ) ;
#29139 = CIRCLE ( 'NONE', #16849, 1.499999999999996225 ) ;
#29140 = CARTESIAN_POINT ( 'NONE',  ( 176.1922820468852819, -1.999999999999969358, -19.40354224447947473 ) ) ;
#29141 = CARTESIAN_POINT ( 'NONE',  ( 14.03260640326807085, 7.914523595725262872, -15.18742456645827588 ) ) ;
#29142 = CARTESIAN_POINT ( 'NONE',  ( 13.12362514754451759, 8.570858352459396201, -15.91189866610160841 ) ) ;
#29143 = CARTESIAN_POINT ( 'NONE',  ( 49.00000000000000000, 0.000000000000000000, 0.000000000000000000 ) ) ;
#29144 = CARTESIAN_POINT ( 'NONE',  ( 0.000000000000000000, 1.162403506782538081E-16, -4.187999999999997947 ) ) ;
#29145 = ORIENTED_EDGE ( 'NONE', *, *, #14205, .F. ) ;
#29146 = DIRECTION ( 'NONE',  ( -2.698458740408365879E-16, 1.000000000000000000, 0.000000000000000000 ) ) ;
#29147 = CARTESIAN_POINT ( 'NONE',  ( 159.5152310637604671, -1.999999999999974021, -2.627941064794695691 ) ) ;
#29148 = CARTESIAN_POINT ( 'NONE',  ( 162.2287565553229172, -4.999999999999973355, -3.509618943233400401 ) ) ;
#29149 = VERTEX_POINT ( 'NONE', #6996 ) ;
#29150 = VERTEX_POINT ( 'NONE', #7293 ) ;
#29151 = VERTEX_POINT ( 'NONE', #21474 ) ;
#29152 = CARTESIAN_POINT ( 'NONE',  ( 8.944584812045984989, 16.95159217075808655, -17.91472939532503261 ) ) ;
#29153 = CARTESIAN_POINT ( 'NONE',  ( 18.07402036735202699, 11.65617268414930940, -17.08825885362000108 ) ) ;
#29154 = CARTESIAN_POINT ( 'NONE',  ( 25.71810023473615203, -5.953606672203104466, -12.71518937071605038 ) ) ;
#29155 = CIRCLE ( 'NONE', #24724, 2.500000000000002665 ) ;
#29156 = LINE ( 'NONE', #26541, #21858 ) ;
#29157 = CARTESIAN_POINT ( 'NONE',  ( 157.0152310637605240, -4.999999999999975131, -1.743219247438260444E-14 ) ) ;
#29158 = DIRECTION ( 'NONE',  ( 0.5877852522924731371, 1.586114251531760728E-16, 0.8090169943749474513 ) ) ;
#29159 = VECTOR ( 'NONE', #16756, 1000.000000000000000 ) ;
#29160 = ORIENTED_EDGE ( 'NONE', *, *, #13523, .F. ) ;
#29161 = CARTESIAN_POINT ( 'NONE',  ( 173.6922820468852535, -9.999999999999996447, 2.247092850131519715 ) ) ;
#29163 = ORIENTED_EDGE ( 'NONE', *, *, #17546, .F. ) ;
#29162 = CARTESIAN_POINT ( 'NONE',  ( -13.00000000000000178, 0.000000000000000000, -15.00000000000000000 ) ) ;
#29164 = CARTESIAN_POINT ( 'NONE',  ( 147.0152310637605808, -1.999999999999976685, -15.61832212156129707 ) ) ;
#29165 = LINE ( 'NONE', #12482, #15289 ) ;
#29166 = CARTESIAN_POINT ( 'NONE',  ( 13.09695832212169364, 8.559710067821024282, -15.93310406974445392 ) ) ;
#29167 = ADVANCED_FACE ( 'NONE', ( #9562 ), #26073, .T. ) ;
#29168 = EDGE_CURVE ( 'NONE', #22823, #13441, #24353, .T. ) ;
#29169 = CARTESIAN_POINT ( 'NONE',  ( 33.66936448658974257, -12.74213349194280553, -18.74758104053764995 ) ) ;
#29170 = ORIENTED_EDGE ( 'NONE', *, *, #22591, .T. ) ;
#29171 = ADVANCED_FACE ( 'NONE', ( #9257 ), #1951, .F. ) ;
#29172 = CARTESIAN_POINT ( 'NONE',  ( 9.177416647856844634, 15.88379569257361190, -17.02789189981719176 ) ) ;
#29173 = EDGE_CURVE ( 'NONE', #20403, #26738, #16892, .T. ) ;
#29174 = VERTEX_POINT ( 'NONE', #19036 ) ;
#29175 = AXIS2_PLACEMENT_3D ( 'NONE', #4113, #13407, #22733 ) ;
#29176 = EDGE_CURVE ( 'NONE', #1558, #22770, #16439, .T. ) ;
#29177 = CARTESIAN_POINT ( 'NONE',  ( 22.09544204423535874, -4.864148257255451746, -14.35781331922719772 ) ) ;
#29178 = CARTESIAN_POINT ( 'NONE',  ( 10.35867142355733783, 16.97202304209818990, -17.90451223021000260 ) ) ;
#29179 = FACE_BOUND ( 'NONE', #29960, .T. ) ;
#29180 = VERTEX_POINT ( 'NONE', #584 ) ;
#29181 = ORIENTED_EDGE ( 'NONE', *, *, #5500, .T. ) ;
#29182 = AXIS2_PLACEMENT_3D ( 'NONE', #1578, #8868, #18181 ) ;
#29183 = DIRECTION ( 'NONE',  ( -0.9510565162951536422, -2.566386769018988816E-16, -0.3090169943749472292 ) ) ;
#29184 = CARTESIAN_POINT ( 'NONE',  ( 12.49271550807400999, 8.567542729147559655, -15.13597632865050535 ) ) ;
#29185 = FACE_OUTER_BOUND ( 'NONE', #2405, .T. ) ;
#29186 = VERTEX_POINT ( 'NONE', #28538 ) ;
#29187 = LINE ( 'NONE', #14934, #16910 ) ;
#29188 = ORIENTED_EDGE ( 'NONE', *, *, #5438, .F. ) ;
#29189 = CARTESIAN_POINT ( 'NONE',  ( 12.03206445085756116, 9.298183410334813104, -16.68962916345529024 ) ) ;
#29190 = ORIENTED_EDGE ( 'NONE', *, *, #28665, .F. ) ;
#29191 = CARTESIAN_POINT ( 'NONE',  ( 18.26434493437671946, 4.448125397982363616, -12.89349226661579273 ) ) ;
#29192 = CARTESIAN_POINT ( 'NONE',  ( 15.46132241025727083, 3.192341012408233869, -14.38206433644783111 ) ) ;
#29193 = LINE ( 'NONE', #21829, #8650 ) ;
#29194 = ORIENTED_EDGE ( 'NONE', *, *, #6986, .T. ) ;
#29195 = B_SPLINE_CURVE_WITH_KNOTS ( 'NONE', 3,
 ( #16394, #18691, #1519, #13391, #22717, #28038 ),
 .UNSPECIFIED., .F., .F.,
 ( 4, 2, 4 ),
 ( 0.01291313371729458682, 0.01525081363757309696, 0.01758849355785160884 ),
 .UNSPECIFIED. ) ;
#29196 = CARTESIAN_POINT ( 'NONE',  ( 36.21530066971708095, -20.68720585756345187, -20.37220581101806971 ) ) ;
#29197 = CARTESIAN_POINT ( 'NONE',  ( 14.18486973814142793, 6.324582201221724098, -17.68508340245422872 ) ) ;
#29198 = ORIENTED_EDGE ( 'NONE', *, *, #18578, .F. ) ;
#29199 = CARTESIAN_POINT ( 'NONE',  ( 0.000000000000000000, 0.000000000000000000, 0.000000000000000000 ) ) ;
#29200 = DIRECTION ( 'NONE',  ( -2.698458740408365879E-16, 1.000000000000000000, 0.000000000000000000 ) ) ;
#29201 = ORIENTED_EDGE ( 'NONE', *, *, #18481, .T. ) ;
#29202 = AXIS2_PLACEMENT_3D ( 'NONE', #9729, #25615, #13857 ) ;
#29203 = PLANE ( 'NONE',  #7793 ) ;
#29204 = EDGE_CURVE ( 'NONE', #25168, #20384, #2719, .T. ) ;
#29205 = CARTESIAN_POINT ( 'NONE',  ( 167.2287565553229456, -1.999999999999970912, -20.83012701892220520 ) ) ;
#29206 = CARTESIAN_POINT ( 'NONE',  ( 172.7287565553229456, -1.999999999999974021, 0.5000000000000029976 ) ) ;
#29207 = ORIENTED_EDGE ( 'NONE', *, *, #16897, .T. ) ;
#29208 = ADVANCED_FACE ( 'NONE', ( #26224 ), #5304, .T. ) ;
#29209 = DIRECTION ( 'NONE',  ( -2.908569913943825554E-16, 1.000000000000000000, 0.000000000000000000 ) ) ;
#29210 = EDGE_CURVE ( 'NONE', #7358, #27200, #28394, .T. ) ;
#29211 = CARTESIAN_POINT ( 'NONE',  ( 11.05541531668977662, 17.68942339022145305, -21.33333333332589632 ) ) ;
#29212 = DIRECTION ( 'NONE',  ( -0.9510565162951536422, 0.000000000000000000, -0.3090169943749472292 ) ) ;
#29213 = CARTESIAN_POINT ( 'NONE',  ( 0.000000000000000000, 1.178949249685215417, -2.042000000000002036 ) ) ;
#29214 = ORIENTED_EDGE ( 'NONE', *, *, #7665, .F. ) ;
#29215 = CARTESIAN_POINT ( 'NONE',  ( 12.50481220565295004, 8.572828783776230921, -15.12633959982445653 ) ) ;
#29216 = ORIENTED_EDGE ( 'NONE', *, *, #9443, .F. ) ;
#29217 =( REPRESENTATION_RELATIONSHIP ('NONE','NONE', #5250, #11460 ) REPRESENTATION_RELATIONSHIP_WITH_TRANSFORMATION ( #14646 )SHAPE_REPRESENTATION_RELATIONSHIP( ) );
#29218 = CARTESIAN_POINT ( 'NONE',  ( 10.66806909375856627, 9.047473561677174203, -16.41145467664113156 ) ) ;
#29219 = CARTESIAN_POINT ( 'NONE',  ( 176.1922820468852535, -9.999999999999994671, -2.083034168790677043 ) ) ;
#29220 = CARTESIAN_POINT ( 'NONE',  ( 175.7287565553229456, -4.999999999999970690, -33.50000000000000000 ) ) ;
#29221 = EDGE_LOOP ( 'NONE', ( #5830, #15286, #2056, #18595, #21547 ) ) ;
#29222 = VERTEX_POINT ( 'NONE', #14590 ) ;
#29223 = CARTESIAN_POINT ( 'NONE',  ( 420.0000000000002274, 41.64101615137744972, 12.00000000000000178 ) ) ;
#29224 = ORIENTED_EDGE ( 'NONE', *, *, #1549, .F. ) ;
#29225 = CARTESIAN_POINT ( 'NONE',  ( 12.82717298413408358, 9.563916880749394167, -16.14313977175105919 ) ) ;
#29226 = VECTOR ( 'NONE', #24697, 1000.000000000000000 ) ;
#29227 = CARTESIAN_POINT ( 'NONE',  ( 34.61906131182126245, -12.51614797404085877, -18.96439083239160439 ) ) ;
#29228 = CARTESIAN_POINT ( 'NONE',  ( 19.07848178107829540, -2.338951347401693859, -17.85627120065723616 ) ) ;
#29229 = ORIENTED_EDGE ( 'NONE', *, *, #27696, .F. ) ;
#29230 = ORIENTED_EDGE ( 'NONE', *, *, #612, .F. ) ;
#29231 = CIRCLE ( 'NONE', #27294, 13.00000000000000178 ) ;
#29232 = DIRECTION ( 'NONE',  ( 1.000000000000000000, 2.220446049250312686E-15, 0.000000000000000000 ) ) ;
#29233 = CARTESIAN_POINT ( 'NONE',  ( 13.15390973649967599, 8.859676595473322536, -14.60899741038990562 ) ) ;
#29234 = CARTESIAN_POINT ( 'NONE',  ( -4.000000000000005329, 1.935983797701048559, -0.2494693066162272932 ) ) ;
#29235 = VECTOR ( 'NONE', #9577, 1000.000000000000000 ) ;
#29236 = LINE ( 'NONE', #1580, #17378 ) ;
#29237 = CARTESIAN_POINT ( 'NONE',  ( 22.28231863826031756, 1.183864898644814811, -18.90614694914491167 ) ) ;
#29238 = CARTESIAN_POINT ( 'NONE',  ( 18.31109272121128484, -1.763409964857557188, -18.37077502410619090 ) ) ;
#29239 = VERTEX_POINT ( 'NONE', #23939 ) ;
#29240 = VERTEX_POINT ( 'NONE', #25763 ) ;
#29241 = EDGE_CURVE ( 'NONE', #20829, #13408, #16595, .T. ) ;
#29242 = LINE ( 'NONE', #7983, #1576 ) ;
#29243 = DIRECTION ( 'NONE',  ( -0.9510565162951536422, -2.566386769018988323E-16, 0.3090169943749475623 ) ) ;
#29244 = DIRECTION ( 'NONE',  ( 0.9510565162951536422, 2.566386769018988816E-16, 0.3090169943749472292 ) ) ;
#29245 = FACE_OUTER_BOUND ( 'NONE', #2205, .T. ) ;
#29246 = VECTOR ( 'NONE', #5971, 1000.000000000000000 ) ;
#29247 = CARTESIAN_POINT ( 'NONE',  ( 167.2287565553230024, -4.999999999999972466, -29.49038105676661559 ) ) ;
#29248 = EDGE_CURVE ( 'NONE', #23660, #14857, #21168, .T. ) ;
#29249 = EDGE_CURVE ( 'NONE', #4536, #17531, #12006, .T. ) ;
#29250 = LINE ( 'NONE', #13169, #9980 ) ;
#29251 = CARTESIAN_POINT ( 'NONE',  ( 11.21893088074867073, 9.114006857625895464, -17.24365706284262600 ) ) ;
#29252 = ORIENTED_EDGE ( 'NONE', *, *, #29293, .F. ) ;
#29253 = EDGE_CURVE ( 'NONE', #19707, #28625, #4389, .T. ) ;
#29254 = B_SPLINE_CURVE_WITH_KNOTS ( 'NONE', 3,
 ( #16251, #396, #2241, #11513, #11967, #18703, #21286, #14104, #23746, #23283, #13804, #4965, #7104, #25729, #19005, #23132, #23586, #4515, #16561, #555, #28208, #28363, #4658, #248, #18847, #2843, #4810, #7418, #2395, #16718, #23438, #9681, #5114, #12129, #20828, #27905, #2550, #11821, #11669, #14406, #21443, #9839, #21138, #9524, #16861, #7262, #25887, #14255, #19152, #30211, #9220, #28509, #7558, #18548, #20984, #25564, #9376, #21893, #17308, #26805, #19449, #7856, #7709, #12876, #845, #10135, #24494, #26192, #12729, #3002, #5271, #24052, #21597, #22050, #19595, #12279, #1152, #695, #10432, #28963, #17018, #22190, #29266, #10286, #19741, #26341, #28818, #1008, #14710, #5424, #17164, #5878, #8300, #7999, #3436, #15158, #10589, #5575, #3152, #24340, #19298, #23905, #9983, #29110, #26494, #8150, #14856, #3586, #12425, #14558, #26647, #24197, #3299, #17457, #28656, #15009, #21743, #5727, #1299, #19897, #12574, #17754, #13328, #1752, #6619, #10884, #1909, #6172, #20497, #17894, #25089, #8892, #15911, #3734, #10746, #27274, #24953, #15465, #11188, #4179, #27565, #6324, #15620, #30025, #20343, #11042, #29733, #8741, #17607, #13032, #4034, #8595, #29883, #27111, #18058, #3886, #22652, #27421, #18206, #20195, #29579, #29428, #4328, #22508, #15306, #25241, #13625, #1609, #20054, #22956, #24796, #2057, #6475, #15765, #13473, #13184, #22804, #11336, #22349, #20641, #26963, #6023, #8448, #24639, #1455, #9034, #9648, #2516, #14368, #11477, #6771, #7227, #23248, #25850, #18669, #28324, #18512, #18357, #9489, #2361, #58, #18813, #2204, #23704, #23551, #20793, #4779, #23399, #2654, #9186, #14069, #11784, #7382, #11632, #11929, #27872, #21251, #9342, #16525, #363, #16677, #28170, #23101, #26000, #20946, #6927, #4626, #13773, #4929, #28014, #7073, #21407, #21104, #210, #14221, #18967, #27714, #25391, #16368, #25689, #5076, #2807, #12090, #16220, #25534, #13918 ),
 .UNSPECIFIED., .F., .F.,
 ( 4, 2, 2, 2, 2, 2, 2, 2, 2, 2, 2, 2, 2, 2, 2, 2, 2, 2, 2, 2, 2, 2, 2, 2, 2, 2, 2, 2, 2, 2, 2, 2, 2, 2, 2, 2, 2, 2, 2, 2, 2, 2, 2, 2, 2, 2, 2, 2, 2, 2, 2, 2, 2, 2, 2, 2, 2, 2, 2, 2, 2, 2, 2, 2, 2, 2, 2, 2, 2, 2, 2, 2, 2, 2, 2, 2, 2, 2, 2, 2, 2, 2, 2, 2, 2, 2, 2, 2, 2, 2, 2, 2, 2, 2, 2, 2, 2, 2, 2, 2, 2, 2, 2, 2, 2, 2, 2, 2, 2, 2, 2, 2, 2, 2, 2, 2, 2, 2, 2, 2, 2, 2, 4 ),
 ( 0.000000000000000000, 0.007812500000000000000, 0.01464843750000000000, 0.02148437500000000000, 0.02832031250000000000, 0.03515625000000000000, 0.04882812500000000000, 0.05566406250000000000, 0.06250000000000000000, 0.06933593750000000000, 0.07617187500000000000, 0.08984375000000000000, 0.09667968750000000000, 0.1035156250000000000, 0.1103515625000000000, 0.1171875000000000000, 0.1240234375000000000, 0.1308593750000000000, 0.1376953125000000000, 0.1445312500000000000, 0.1513671875000000000, 0.1582031250000000000, 0.1718750000000000000, 0.1787109375000000000, 0.1855468750000000000, 0.1992187500000000000, 0.2060546875000000000, 0.2128906250000000000, 0.2197265625000000000, 0.2265625000000000000, 0.2402343750000000000, 0.2470703125000000000, 0.2539062500000000000, 0.2607421875000000000, 0.2675781250000000000, 0.2812500000000000000, 0.2880859375000000000, 0.2949218750000000000, 0.3017578125000000000, 0.3085937500000000000, 0.3154296875000000000, 0.3222656250000000000, 0.3291015625000000000, 0.3359375000000000000, 0.3496093750000000000, 0.3564453125000000000, 0.3632812500000000000, 0.3701171875000000000, 0.3769531250000000000, 0.3906250000000000000, 0.3974609375000000000, 0.4042968750000000000, 0.4179687500000000000, 0.4316406250000000000, 0.4384765625000000000, 0.4453125000000000000, 0.4521484375000000000, 0.4589843750000000000, 0.4658203125000000000, 0.4726562500000000000, 0.4794921875000000000, 0.4863281250000000000, 0.4931640625000000000, 0.5000000000000000000, 0.5078125000000000000, 0.5156250000000000000, 0.5234375000000000000, 0.5312500000000000000, 0.5390625000000000000, 0.5468750000000000000, 0.5625000000000000000, 0.5693359375000000000, 0.5761718750000000000, 0.5898437500000000000, 0.5966796875000000000, 0.6035156250000000000, 0.6103515625000000000, 0.6171875000000000000, 0.6308593750000000000, 0.6376953125000000000, 0.6445312500000000000, 0.6513671875000000000, 0.6582031250000000000, 0.6718750000000000000, 0.6787109375000000000, 0.6855468750000000000, 0.6992187500000000000, 0.7128906250000000000, 0.7197265625000000000, 0.7265625000000000000, 0.7333984375000000000, 0.7402343750000000000, 0.7470703125000000000, 0.7539062500000000000, 0.7607421875000000000, 0.7675781250000000000, 0.7744140625000000000, 0.7812500000000000000, 0.7890625000000000000, 0.7968750000000000000, 0.8046875000000000000, 0.8125000000000000000, 0.8203125000000000000, 0.8281250000000000000, 0.8437500000000000000, 0.8505859375000000000, 0.8574218750000000000, 0.8710937500000000000, 0.8779296875000000000, 0.8847656250000000000, 0.8916015625000000000, 0.8984375000000000000, 0.9121093750000000000, 0.9189453125000000000, 0.9257812500000000000, 0.9326171875000000000, 0.9394531250000000000, 0.9531250000000000000, 0.9589843750000000000, 0.9648437500000000000, 0.9765625000000000000, 0.9882812500000000000, 1.000000000000000000 ),
 .UNSPECIFIED. ) ;
#29255 = CARTESIAN_POINT ( 'NONE',  ( 11.47029057985033340, 9.281140223223081520, -15.86198156829250117 ) ) ;
#29256 = CIRCLE ( 'NONE', #5312, 3.000000000000002665 ) ;
#29257 = ADVANCED_FACE ( 'NONE', ( #10627 ), #26376, .F. ) ;
#29258 = CARTESIAN_POINT ( 'NONE',  ( 27.15293434934692129, -9.258526923162836653, -12.62629486378885701 ) ) ;
#29259 = ORIENTED_EDGE ( 'NONE', *, *, #21975, .T. ) ;
#29260 = LINE ( 'NONE', #15300, #1776 ) ;
#29261 = PLANE ( 'NONE',  #14062 ) ;
#29262 = LINE ( 'NONE', #24193, #8236 ) ;
#29263 = FACE_OUTER_BOUND ( 'NONE', #15238, .T. ) ;
#29264 = FACE_OUTER_BOUND ( 'NONE', #21322, .T. ) ;
#29265 = FACE_OUTER_BOUND ( 'NONE', #5828, .T. ) ;
#29266 = CARTESIAN_POINT ( 'NONE',  ( 18.50902107916489570, 2.085137940960992697, -20.06823964296112450 ) ) ;
#29267 = ORIENTED_EDGE ( 'NONE', *, *, #29655, .F. ) ;
#29268 = DIRECTION ( 'NONE',  ( 1.000000000000000000, 0.000000000000000000, 0.000000000000000000 ) ) ;
#29269 = CARTESIAN_POINT ( 'NONE',  ( 12.27682979692750997, 9.494989133591600350, -15.31072415319233215 ) ) ;
#29270 = LINE ( 'NONE', #8305, #791 ) ;
#29271 = FACE_OUTER_BOUND ( 'NONE', #19000, .T. ) ;
#29272 = CARTESIAN_POINT ( 'NONE',  ( 21.42923412144385509, -1.598955984811285536, -13.33006947543598741 ) ) ;
#29273 = CARTESIAN_POINT ( 'NONE',  ( 156.1922820468853956, -1.999999999999974465, -22.25671179336496053 ) ) ;
#29274 = CARTESIAN_POINT ( 'NONE',  ( 18.57953865233433532, 8.080199298666570940, -13.63460617990120838 ) ) ;
#29275 = EDGE_LOOP ( 'NONE', ( #18120, #25008, #5795, #11000, #17034 ) ) ;
#29276 = CARTESIAN_POINT ( 'NONE',  ( 35.54859390953724585, -22.18451583373416014, -16.11276402859391865 ) ) ;
#29277 = VECTOR ( 'NONE', #27375, 1000.000000000000000 ) ;
#29278 = CARTESIAN_POINT ( 'NONE',  ( 24.62608015258945215, -5.401662417846991637, -13.04198456947205820 ) ) ;
#29279 = CARTESIAN_POINT ( 'NONE',  ( 22.90368100322821121, -1.908636692139587199, -20.53213217155426662 ) ) ;
#29280 = VECTOR ( 'NONE', #1967, 1000.000000000000000 ) ;
#29281 = ORIENTED_EDGE ( 'NONE', *, *, #27767, .T. ) ;
#29282 = LINE ( 'NONE', #17771, #1015 ) ;
#29283 = EDGE_LOOP ( 'NONE', ( #22446, #17177, #16493, #2981 ) ) ;
#29284 = FACE_OUTER_BOUND ( 'NONE', #10128, .T. ) ;
#29285 = EDGE_LOOP ( 'NONE', ( #14750, #25303, #8962, #525 ) ) ;
#29286 = DIRECTION ( 'NONE',  ( 8.163404592832029035E-16, 2.202861047501738386E-31, 1.000000000000000000 ) ) ;
#29287 = LINE ( 'NONE', #24366, #10105 ) ;
#29288 = ADVANCED_FACE ( 'NONE', ( #14885 ), #26685, .T. ) ;
#29289 = DIRECTION ( 'NONE',  ( 0.5877852522924731371, 0.000000000000000000, 0.8090169943749474513 ) ) ;
#29290 = EDGE_CURVE ( 'NONE', #11499, #29523, #5760, .T. ) ;
#29291 = CARTESIAN_POINT ( 'NONE',  ( 0.000000000000000000, 2.357898499370430834, -3.469446951953614189E-15 ) ) ;
#29292 =( GEOMETRIC_REPRESENTATION_CONTEXT ( 3 ) GLOBAL_UNCERTAINTY_ASSIGNED_CONTEXT ( ( #11919 ) ) GLOBAL_UNIT_ASSIGNED_CONTEXT ( ( #25221, #29552, #20316 ) ) REPRESENTATION_CONTEXT ( 'NONE', 'WORKASPACE' ) );
#29293 = EDGE_CURVE ( 'NONE', #12642, #11550, #21780, .T. ) ;
#29294 = CARTESIAN_POINT ( 'NONE',  ( 23.95332181684718975, -6.025008234661991757, -14.41687206698971124 ) ) ;
#29295 = LINE ( 'NONE', #3764, #10222 ) ;
#29296 = CARTESIAN_POINT ( 'NONE',  ( 34.15817405333866219, -12.44562566045073204, -20.90971876709214783 ) ) ;
#29298 = LINE ( 'NONE', #22685, #22211 ) ;
#29297 = AXIS2_PLACEMENT_3D ( 'NONE', #29143, #10014, #12762 ) ;
#29299 = CARTESIAN_POINT ( 'NONE',  ( 9.919231947839115549, 16.39449282361540483, -16.50339887433786501 ) ) ;
#29300 = TOROIDAL_SURFACE ( 'NONE', #17, 2.700000000000001066, 0.2000000000000000111 ) ;
#29301 = CARTESIAN_POINT ( 'NONE',  ( 172.2287565553228603, -4.999999999999970690, -3.509618943233400401 ) ) ;
#29302 = CARTESIAN_POINT ( 'NONE',  ( 144.5152310637605808, -10.00000000000000178, -30.37205893520530964 ) ) ;
#29304 = CARTESIAN_POINT ( 'NONE',  ( 9.661883062155979474, 16.25482663112457971, -17.91578995581314260 ) ) ;
#29303 = VECTOR ( 'NONE', #271, 1000.000000000000000 ) ;
#29305 = PLANE ( 'NONE',  #17066 ) ;
#29306 = CARTESIAN_POINT ( 'NONE',  ( 136.1922820468854241, -1.999999999999980016, -28.06379628232387446 ) ) ;
#29307 = CARTESIAN_POINT ( 'NONE',  ( 11.47276097331165623, 9.269810413962238371, -15.86095999428340697 ) ) ;
#29308 = ORIENTED_EDGE ( 'NONE', *, *, #28285, .F. ) ;
#29309 = VERTEX_POINT ( 'NONE', #22227 ) ;
#29310 = DIRECTION ( 'NONE',  ( -1.110223024625156540E-16, 0.000000000000000000, -1.000000000000000000 ) ) ;
#29311 = CARTESIAN_POINT ( 'NONE',  ( 177.2287565553228319, -9.999999999999994671, -3.509618943233403510 ) ) ;
#29312 = DIRECTION ( 'NONE',  ( 0.5877852522924731371, 1.586114251531760728E-16, -0.8090169943749474513 ) ) ;
#29313 = ORIENTED_EDGE ( 'NONE', *, *, #2717, .F. ) ;
#29314 = CARTESIAN_POINT ( 'NONE',  ( 13.38606102883407445, 7.628803627606831839, -15.70273264218319120 ) ) ;
#29316 = AXIS2_PLACEMENT_3D ( 'NONE', #14101, #244, #552 ) ;
#29315 = CARTESIAN_POINT ( 'NONE',  ( 31.50466570323033011, -10.22776944099620877, -17.14799365788790553 ) ) ;
#29317 = VECTOR ( 'NONE', #5574, 1000.000000000000000 ) ;
#29318 = CARTESIAN_POINT ( 'NONE',  ( 26.55477173981947914, -11.17418396328012342, -19.38009549175560053 ) ) ;
#29319 = VECTOR ( 'NONE', #25848, 1000.000000000000000 ) ;
#29320 = CARTESIAN_POINT ( 'NONE',  ( 30.02037170576755187, -9.505783518442527225, -18.49971606337314967 ) ) ;
#29321 = CARTESIAN_POINT ( 'NONE',  ( 139.5152310637605808, -1.999999999999979128, -2.627941064794695691 ) ) ;
#29322 = DIRECTION ( 'NONE',  ( -0.8090169943749474513, -2.183098979609982436E-16, 0.5877852522924731371 ) ) ;
#29323 = DIRECTION ( 'NONE',  ( 1.000000000000000000, 4.440892098500622217E-16, 0.000000000000000000 ) ) ;
#29324 = EDGE_CURVE ( 'NONE', #15781, #18049, #24376, .T. ) ;
#29325 = ADVANCED_FACE ( 'NONE', ( #12609 ), #29305, .T. ) ;
#29326 = CIRCLE ( 'NONE', #14629, 5.000000000000006217 ) ;
#29327 = ORIENTED_EDGE ( 'NONE', *, *, #2382, .T. ) ;
#29328 = VERTEX_POINT ( 'NONE', #26998 ) ;
#29329 = DIRECTION ( 'NONE',  ( 0.000000000000000000, 0.000000000000000000, 1.000000000000000000 ) ) ;
#29331 = EDGE_LOOP ( 'NONE', ( #11053, #3694 ) ) ;
#29330 = PLANE ( 'NONE',  #5835 ) ;
#29332 = ORIENTED_EDGE ( 'NONE', *, *, #22362, .F. ) ;
#29333 = CARTESIAN_POINT ( 'NONE',  ( 144.5152310637606092, -1.999999999999977129, -28.60870317832789311 ) ) ;
#29334 = VECTOR ( 'NONE', #13524, 1000.000000000000000 ) ;
#29335 = CARTESIAN_POINT ( 'NONE',  ( 13.12808413666193275, 8.572828783776230921, -15.90834477884588516 ) ) ;
#29336 = ORIENTED_EDGE ( 'NONE', *, *, #24742, .F. ) ;
#29337 = CARTESIAN_POINT ( 'NONE',  ( 33.30991885831043220, -11.83535627117299960, -18.22721479198959926 ) ) ;
#29338 = ORIENTED_EDGE ( 'NONE', *, *, #29040, .T. ) ;
#29339 = VECTOR ( 'NONE', #16330, 1000.000000000000000 ) ;
#29340 = CARTESIAN_POINT ( 'NONE',  ( 9.760963200462100531, 13.20757681744125911, -16.78657487285272509 ) ) ;
#29341 = VERTEX_POINT ( 'NONE', #720 ) ;
#29342 = CARTESIAN_POINT ( 'NONE',  ( 26.85315702054868936, -3.432285194908070380, -17.01323758698984889 ) ) ;
#29343 = CARTESIAN_POINT ( 'NONE',  ( 15.98547205987755149, 10.89358938796158149, -13.63095616771664709 ) ) ;
#29344 = FACE_BOUND ( 'NONE', #23976, .T. ) ;
#29345 = ORIENTED_EDGE ( 'NONE', *, *, #3608, .T. ) ;
#29346 = ORIENTED_EDGE ( 'NONE', *, *, #14477, .T. ) ;
#29347 =( GEOMETRIC_REPRESENTATION_CONTEXT ( 3 ) GLOBAL_UNCERTAINTY_ASSIGNED_CONTEXT ( ( #18043 ) ) GLOBAL_UNIT_ASSIGNED_CONTEXT ( ( #29441, #15481, #10898 ) ) REPRESENTATION_CONTEXT ( 'NONE', 'WORKASPACE' ) );
#29348 = ORIENTED_EDGE ( 'NONE', *, *, #957, .F. ) ;
#29349 = DIRECTION ( 'NONE',  ( 1.000000000000000000, 2.698458740408365879E-16, 0.000000000000000000 ) ) ;
#29350 = CARTESIAN_POINT ( 'NONE',  ( 11.47231678315799464, 9.271847796573304379, -15.86114366194887815 ) ) ;
#29351 = CARTESIAN_POINT ( 'NONE',  ( 151.1922820468854241, -10.00000000000000178, -19.40354224447947828 ) ) ;
#29352 = VERTEX_POINT ( 'NONE', #5455 ) ;
#29353 = DIRECTION ( 'NONE',  ( 1.000000000000000000, 2.698458740408365879E-16, -1.110223024625156540E-16 ) ) ;
#29354 = ORIENTED_EDGE ( 'NONE', *, *, #21857, .T. ) ;
#29355 = CARTESIAN_POINT ( 'NONE',  ( 9.661883066202028303, 16.25482661256886630, -17.91573536996246929 ) ) ;
#29356 = EDGE_LOOP ( 'NONE', ( #12073, #16221, #24914, #19596, #6551 ) ) ;
#29357 = CARTESIAN_POINT ( 'NONE',  ( 18.01687101988986583, 8.608027666922664523, -14.27462087050975015 ) ) ;
#29358 = CARTESIAN_POINT ( 'NONE',  ( 20.85347709306256547, 5.504344946561741558, -13.72608531385973407 ) ) ;
#29359 = CARTESIAN_POINT ( 'NONE',  ( 0.2500000000000002220, 0.000000000000000000, 4.250000000000000000 ) ) ;
#29360 = ORIENTED_EDGE ( 'NONE', *, *, #9581, .F. ) ;
#29361 = CARTESIAN_POINT ( 'NONE',  ( 36.54859390953724585, -22.18451583373416014, -18.19919658220850778 ) ) ;
#29362 = AXIS2_PLACEMENT_3D ( 'NONE', #394, #20826, #23280 ) ;
#29363 = ADVANCED_FACE ( 'NONE', ( #6059 ), #17339, .T. ) ;
#29364 = AXIS2_PLACEMENT_3D ( 'NONE', #6177, #8747, #13335 ) ;
#29365 = EDGE_CURVE ( 'NONE', #24258, #13389, #21449, .T. ) ;
#29366 = CARTESIAN_POINT ( 'NONE',  ( 14.73401617531889229, 6.408058468588501810, -15.60580005407095960 ) ) ;
#29367 = DIRECTION ( 'NONE',  ( 0.3090169943749475623, 8.338696094058001131E-17, 0.9510565162951536422 ) ) ;
#29368 = FACE_BOUND ( 'NONE', #7413, .T. ) ;
#29369 = ORIENTED_EDGE ( 'NONE', *, *, #11245, .F. ) ;
#29370 = ORIENTED_EDGE ( 'NONE', *, *, #10502, .T. ) ;
#29371 = FACE_OUTER_BOUND ( 'NONE', #5793, .T. ) ;
#29372 = CARTESIAN_POINT ( 'NONE',  ( 31.75084456790824206, -10.91497342604502307, -15.84208767625797165 ) ) ;
#29373 = CARTESIAN_POINT ( 'NONE',  ( 174.7287565553228319, -4.999999999999969802, 0.8205080756888000204 ) ) ;
#29374 = ORIENTED_EDGE ( 'NONE', *, *, #823, .F. ) ;
#29375 = CARTESIAN_POINT ( 'NONE',  ( 130.7287565553229456, -4.999999999999983125, 3.500000000000003109 ) ) ;
#29376 = CARTESIAN_POINT ( 'NONE',  ( 12.24611073458536836, 9.516504178424655791, -15.33253149294119311 ) ) ;
#29377 = CARTESIAN_POINT ( 'NONE',  ( 34.81339731023632567, -19.88166695754494384, -21.17803781427711840 ) ) ;
#29378 = CARTESIAN_POINT ( 'NONE',  ( 174.5152310637604671, -9.999999999999994671, -30.37205893520531319 ) ) ;
#29379 = EDGE_LOOP ( 'NONE', ( #16954, #18161, #14258, #10145 ) ) ;
#29380 = VECTOR ( 'NONE', #27528, 1000.000000000000000 ) ;
#29381 = CARTESIAN_POINT ( 'NONE',  ( 9.641350810849047548, 17.66889113945805789, -21.33333333332589277 ) ) ;
#29382 = ORIENTED_EDGE ( 'NONE', *, *, #12891, .F. ) ;
#29383 = CARTESIAN_POINT ( 'NONE',  ( 12.70479305047265761, 7.604386330824797646, -14.96685888413283294 ) ) ;
#29384 = CARTESIAN_POINT ( 'NONE',  ( 138.6922820468854525, -10.00000000000000533, -15.07341522555727309 ) ) ;
#29385 = CARTESIAN_POINT ( 'NONE',  ( 99.97015463715061401, -4.999999999999990230, 72.63256887516226357 ) ) ;
#29386 = LINE ( 'NONE', #15732, #28660 ) ;
#29387 = EDGE_LOOP ( 'NONE', ( #5143, #13956, #5768, #3980 ) ) ;
#29388 = CARTESIAN_POINT ( 'NONE',  ( 12.86840956200995301, 9.516103707707461723, -16.11530999810414500 ) ) ;
#29389 = CARTESIAN_POINT ( 'NONE',  ( 34.61014508914255572, -12.47609210860084161, -18.96169567217477692 ) ) ;
#29390 = CARTESIAN_POINT ( 'NONE',  ( 19.02541433733466647, 1.263421280649871248, -13.57496312174407826 ) ) ;
#29391 = VERTEX_POINT ( 'NONE', #24682 ) ;
#29392 = VERTEX_POINT ( 'NONE', #24081 ) ;
#29393 = VERTEX_POINT ( 'NONE', #21624 ) ;
#29394 = ORIENTED_EDGE ( 'NONE', *, *, #26709, .T. ) ;
#29395 = PRODUCT ( 'bushing', 'bushing', '', ( #7937 ) ) ;
#29396 = AXIS2_PLACEMENT_3D ( 'NONE', #13902, #8723, #27546 ) ;
#29397 = ORIENTED_EDGE ( 'NONE', *, *, #12031, .F. ) ;
#29398 = CARTESIAN_POINT ( 'NONE',  ( 21.25294847316966695, -5.000000000000011546, -65.40984963230826565 ) ) ;
#29399 = DIRECTION ( 'NONE',  ( 0.000000000000000000, 0.000000000000000000, 1.000000000000000000 ) ) ;
#29400 = DIRECTION ( 'NONE',  ( 0.3090169943749475623, 8.338696094058001131E-17, 0.9510565162951536422 ) ) ;
#29401 = EDGE_CURVE ( 'NONE', #25636, #26738, #10233, .T. ) ;
#29402 = CARTESIAN_POINT ( 'NONE',  ( 24.59975295023496855, -6.462932407320696626, -12.83695652901824147 ) ) ;
#29403 = EDGE_CURVE ( 'NONE', #4895, #4321, #3182, .T. ) ;
#29404 = CARTESIAN_POINT ( 'NONE',  ( 18.63699955181457923, 5.162464354397502397, -14.86688106074863569 ) ) ;
#29405 = ORIENTED_EDGE ( 'NONE', *, *, #17446, .T. ) ;
#29406 = VECTOR ( 'NONE', #27844, 1000.000000000000000 ) ;
#29407 = ADVANCED_FACE ( 'NONE', ( #22083 ), #7739, .T. ) ;
#29408 = VERTEX_POINT ( 'NONE', #19772 ) ;
#29409 = VERTEX_POINT ( 'NONE', #15195 ) ;
#29410 = PLANE ( 'NONE',  #4977 ) ;
#29411 = DIRECTION ( 'NONE',  ( -0.5877852522924731371, 0.000000000000000000, 0.8090169943749474513 ) ) ;
#29412 = CARTESIAN_POINT ( 'NONE',  ( 0.000000000000000000, 0.000000000000000000, 0.000000000000000000 ) ) ;
#29413 = CARTESIAN_POINT ( 'NONE',  ( 139.5152310637606092, -10.00000000000000533, -19.94844914048349338 ) ) ;
#29414 = CARTESIAN_POINT ( 'NONE',  ( 147.0152310637605240, -1.999999999999977129, -8.721423840594312082 ) ) ;
#29415 = AXIS2_PLACEMENT_3D ( 'NONE', #20769, #22784, #2341 ) ;
#29416 = DIRECTION ( 'NONE',  ( -1.110223024625156540E-16, 0.000000000000000000, -1.000000000000000000 ) ) ;
#29417 = CARTESIAN_POINT ( 'NONE',  ( 11.20778676255656059, 9.165115204199564047, -17.24826554773256149 ) ) ;
#29418 = CARTESIAN_POINT ( 'NONE',  ( 12.07641845611955489, 8.540206757827041528, -15.45582622123028216 ) ) ;
#29419 = CARTESIAN_POINT ( 'NONE',  ( 151.1922820468853956, -10.00000000000000178, -10.74328820663507678 ) ) ;
#29420 = VERTEX_POINT ( 'NONE', #5608 ) ;
#29421 = CARTESIAN_POINT ( 'NONE',  ( 2.500000000000000444, 2.357898499370430834, -3.469446951953614189E-15 ) ) ;
#29422 = FACE_OUTER_BOUND ( 'NONE', #21131, .T. ) ;
#29423 = EDGE_LOOP ( 'NONE', ( #13161, #22003, #14019, #16531 ) ) ;
#29424 = CARTESIAN_POINT ( 'NONE',  ( 9.912057827679275235, 16.42739425315605928, -16.50652470164456531 ) ) ;
#29425 = CIRCLE ( 'NONE', #21084, 5.000000000000000000 ) ;
#29426 = DIRECTION ( 'NONE',  ( 0.9510565162951536422, 0.000000000000000000, -0.3090169943749475623 ) ) ;
#29427 = LINE ( 'NONE', #1151, #4872 ) ;
#29428 = CARTESIAN_POINT ( 'NONE',  ( 26.87257363757477435, -3.324124212371978082, -16.68573618535388547 ) ) ;
#29429 = EDGE_LOOP ( 'NONE', ( #26503, #22862, #24249, #3725 ) ) ;
#29430 = LINE ( 'NONE', #15468, #9053 ) ;
#29431 = CARTESIAN_POINT ( 'NONE',  ( 12.27341590537944249, 9.504120828508773045, -15.31263355901650947 ) ) ;
#29432 = CARTESIAN_POINT ( 'NONE',  ( 32.36240160181304759, -11.00785621467150044, -17.57054915585148436 ) ) ;
#29433 = PLANE ( 'NONE',  #14665 ) ;
#29434 = ORIENTED_EDGE ( 'NONE', *, *, #3072, .F. ) ;
#29435 = CARTESIAN_POINT ( 'NONE',  ( 23.11440248821028831, -7.346120041196752659, -16.32852059634029018 ) ) ;
#29436 = DIRECTION ( 'NONE',  ( -1.110223024625156540E-16, 0.000000000000000000, -1.000000000000000000 ) ) ;
#29437 = CARTESIAN_POINT ( 'NONE',  ( 17.27385296224481337, 7.553222137591894203, -13.16260341916398069 ) ) ;
#29438 = ORIENTED_EDGE ( 'NONE', *, *, #175, .F. ) ;
#29439 = CARTESIAN_POINT ( 'NONE',  ( 174.5152310637604671, -1.999999999999969358, -19.94844914048349693 ) ) ;
#29440 = VERTEX_POINT ( 'NONE', #12454 ) ;
#29441 =( LENGTH_UNIT ( ) NAMED_UNIT ( * ) SI_UNIT ( .MILLI., .METRE. ) );
#29442 = CARTESIAN_POINT ( 'NONE',  ( 13.76974871631934860, 5.358497188706473402, -17.46738557873778674 ) ) ;
#29443 = VECTOR ( 'NONE', #9014, 1000.000000000000000 ) ;
#29444 = CARTESIAN_POINT ( 'NONE',  ( 20.85427418779519826, -0.3072727129311651484, -13.36207100503020584 ) ) ;
#29445 = EDGE_CURVE ( 'NONE', #25049, #18808, #24530, .T. ) ;
#29446 = ADVANCED_FACE ( 'NONE', ( #880 ), #24370, .T. ) ;
#29447 = EDGE_CURVE ( 'NONE', #30215, #14937, #17198, .T. ) ;
#29448 = EDGE_CURVE ( 'NONE', #22518, #4151, #22845, .T. ) ;
#29449 = VERTEX_POINT ( 'NONE', #30060 ) ;
#29450 = ORIENTED_EDGE ( 'NONE', *, *, #15722, .F. ) ;
#29451 = CARTESIAN_POINT ( 'NONE',  ( 28.01381056668970260, -10.10121741814351459, -18.82353034625045041 ) ) ;
#29452 = AXIS2_PLACEMENT_3D ( 'NONE', #114, #11251, #20553 ) ;
#29453 = FACE_OUTER_BOUND ( 'NONE', #21370, .T. ) ;
#29454 = ORIENTED_EDGE ( 'NONE', *, *, #13724, .T. ) ;
#29455 = CARTESIAN_POINT ( 'NONE',  ( 8.000000000000010658, 4.618802153517005848, -5.000000000000000888 ) ) ;
#29456 = DIRECTION ( 'NONE',  ( -1.110223024625156540E-16, 0.000000000000000000, -1.000000000000000000 ) ) ;
#29457 = CARTESIAN_POINT ( 'NONE',  ( 132.2287565553230024, -10.00000000000000888, -12.16987298107780013 ) ) ;
#29458 = DIRECTION ( 'NONE',  ( 0.000000000000000000, 0.000000000000000000, -1.000000000000000000 ) ) ;
#29459 = CARTESIAN_POINT ( 'NONE',  ( 27.39421632154990505, -5.413734532252513887, -17.93514013592066902 ) ) ;
#29460 = CARTESIAN_POINT ( 'NONE',  ( 47.87499999999999289, 7.328119615409992624E-16, -4.756499999999998174 ) ) ;
#29461 = CARTESIAN_POINT ( 'NONE',  ( 34.21167138940940333, -12.68596085309027899, -20.92588972839351058 ) ) ;
#29462 = CARTESIAN_POINT ( 'NONE',  ( 130.7287565553229172, -4.999999999999983125, -33.50000000000000000 ) ) ;
#29463 = CARTESIAN_POINT ( 'NONE',  ( 12.48799528366842360, 8.565546312597838607, -15.13973160209665991 ) ) ;
#29464 = LINE ( 'NONE', #1491, #13696 ) ;
#29465 = CARTESIAN_POINT ( 'NONE',  ( 166.1922820468853104, -1.999999999999972244, -2.083034168790677043 ) ) ;
#29466 = CARTESIAN_POINT ( 'NONE',  ( 13.39606018151479461, 8.691252192278360766, -15.69476314099692971 ) ) ;
#29467 = CARTESIAN_POINT ( 'NONE',  ( 130.7287565553229172, -9.999999999999982236, -33.50000000000000000 ) ) ;
#29468 = VERTEX_POINT ( 'NONE', #22545 ) ;
#29469 = CARTESIAN_POINT ( 'NONE',  ( 162.2287565553229456, -1.999999999999972244, -20.83012701892220520 ) ) ;
#29470 = CARTESIAN_POINT ( 'NONE',  ( 9.949118446627077006, 16.25742953053141804, -16.49103975576934644 ) ) ;
#29471 = ADVANCED_FACE ( 'NONE', ( #11230 ), #6659, .T. ) ;
#29472 = ORIENTED_EDGE ( 'NONE', *, *, #28880, .F. ) ;
#29473 = DIRECTION ( 'NONE',  ( 1.110223024625156540E-16, 2.995891024602366092E-32, 1.000000000000000000 ) ) ;
#29474 = DIRECTION ( 'NONE',  ( 0.000000000000000000, 0.000000000000000000, -1.000000000000000000 ) ) ;
#29475 = CARTESIAN_POINT ( 'NONE',  ( 163.6922820468853104, -1.999999999999973133, -9.266330736598359152 ) ) ;
#29476 = VECTOR ( 'NONE', #23268, 1000.000000000000000 ) ;
#29477 = ORIENTED_EDGE ( 'NONE', *, *, #15411, .F. ) ;
#29478 = CARTESIAN_POINT ( 'NONE',  ( 8.944667066222118379, 16.95121494262130213, -17.88907156968992496 ) ) ;
#29479 = CARTESIAN_POINT ( 'NONE',  ( 36.54859390953724585, -23.18451583373416014, -17.99055332684694974 ) ) ;
#29480 = CARTESIAN_POINT ( 'NONE',  ( 17.34455430865552472, 11.59597468841007384, -15.61519298676701695 ) ) ;
#29481 = ADVANCED_FACE ( 'NONE', ( #25426 ), #25278, .T. ) ;
#29482 = CARTESIAN_POINT ( 'NONE',  ( 28.40444427461093113, -11.06999723682266179, -18.98653349803348078 ) ) ;
#29483 = CARTESIAN_POINT ( 'NONE',  ( 14.09485158040538266, -5.000000000000014211, -43.37949266794227299 ) ) ;
#29484 = DIRECTION ( 'NONE',  ( 0.9510565162951536422, 2.566386769018988816E-16, 0.3090169943749472292 ) ) ;
#29485 = EDGE_CURVE ( 'NONE', #6726, #27863, #27785, .T. ) ;
#29486 = DIRECTION ( 'NONE',  ( 0.5877852522924731371, 1.586114251531760728E-16, 0.8090169943749474513 ) ) ;
#29487 = EDGE_CURVE ( 'NONE', #24269, #5616, #4367, .T. ) ;
#29488 = ORIENTED_EDGE ( 'NONE', *, *, #18366, .F. ) ;
#29489 = ORIENTED_EDGE ( 'NONE', *, *, #17743, .T. ) ;
#29490 = DIRECTION ( 'NONE',  ( -0.000000000000000000, 1.000000000000000000, -0.000000000000000000 ) ) ;
#29491 = LINE ( 'NONE', #20253, #4378 ) ;
#29492 = VERTEX_POINT ( 'NONE', #2095 ) ;
#29493 = DIRECTION ( 'NONE',  ( 0.5877852522924731371, 1.586114251531760728E-16, -0.8090169943749474513 ) ) ;
#29494 = AXIS2_PLACEMENT_3D ( 'NONE', #17363, #7913, #21955 ) ;
#29495 = CARTESIAN_POINT ( 'NONE',  ( 12.40302661446015264, 8.678734247659738443, -16.45371344743900366 ) ) ;
#29496 = CARTESIAN_POINT ( 'NONE',  ( 35.54859477393411993, -21.18451971701249548, -18.28760485896911803 ) ) ;
#29497 = CARTESIAN_POINT ( 'NONE',  ( 9.026809008904539411, 16.57450152281700184, -17.18797639273109112 ) ) ;
#29498 = ORIENTED_EDGE ( 'NONE', *, *, #1379, .T. ) ;
#29499 = CARTESIAN_POINT ( 'NONE',  ( 21.65145737125105541, -5.000000000000011546, -66.63633390735121509 ) ) ;
#29500 = CARTESIAN_POINT ( 'NONE',  ( 12.86884521499632150, 9.516296226583106588, -16.11496277528728527 ) ) ;
#29501 = FACE_BOUND ( 'NONE', #4161, .T. ) ;
#29502 = EDGE_CURVE ( 'NONE', #619, #3067, #11080, .T. ) ;
#29503 = VERTEX_POINT ( 'NONE', #6364 ) ;
#29504 = LINE ( 'NONE', #25025, #10518 ) ;
#29505 = ORIENTED_EDGE ( 'NONE', *, *, #22462, .F. ) ;
#29506 = CARTESIAN_POINT ( 'NONE',  ( 11.65548303173490652, 8.849831895876286936, -15.75351705932409985 ) ) ;
#29507 = DIRECTION ( 'NONE',  ( -0.5877852522924731371, -1.586114251531760728E-16, -0.8090169943749474513 ) ) ;
#29508 = CARTESIAN_POINT ( 'NONE',  ( 137.0152310637605808, -10.00000000000000533, -8.721423840594312082 ) ) ;
#29509 = VERTEX_POINT ( 'NONE', #20677 ) ;
#29510 = CARTESIAN_POINT ( 'NONE',  ( 9.661883245193708447, 16.25482579169019459, -17.91553454599451101 ) ) ;
#29511 = CARTESIAN_POINT ( 'NONE',  ( 19.63206833423595299, 9.033623817254925470, -16.13982763006638166 ) ) ;
#29512 = CARTESIAN_POINT ( 'NONE',  ( 15.79264427988833219, 7.655968387373099482, -13.90199225654327897 ) ) ;
#29513 = CARTESIAN_POINT ( 'NONE',  ( 20.00000000000000355, 55.00000000000000711, -24.99999999999999645 ) ) ;
#29514 = CIRCLE ( 'NONE', #16276, 2.000000000000000000 ) ;
#29515 = ORIENTED_EDGE ( 'NONE', *, *, #2565, .T. ) ;
#29516 = LINE ( 'NONE', #6563, #10335 ) ;
#29517 = EDGE_CURVE ( 'NONE', #5352, #20011, #9072, .T. ) ;
#29518 = CONTEXT_DEPENDENT_SHAPE_REPRESENTATION ( #22367, #25217 ) ;
#29519 = CARTESIAN_POINT ( 'NONE',  ( 21.19279910686179846, 4.720633506281588510, -19.26595127233560234 ) ) ;
#29520 = VECTOR ( 'NONE', #23131, 1000.000000000000000 ) ;
#29521 = CARTESIAN_POINT ( 'NONE',  ( 146.1922820468854525, -4.999999999999978684, -22.25671179336496053 ) ) ;
#29522 = DIRECTION ( 'NONE',  ( -1.000000000000000000, 0.000000000000000000, 0.000000000000000000 ) ) ;
#29523 = VERTEX_POINT ( 'NONE', #22388 ) ;
#29524 = CARTESIAN_POINT ( 'NONE',  ( -8.000000000000000000, 0.000000000000000000, -15.00000000000000355 ) ) ;
#29525 = CARTESIAN_POINT ( 'NONE',  ( 34.54007435814109783, -17.65377171698271752, -20.05309729467257540 ) ) ;
#29526 = CARTESIAN_POINT ( 'NONE',  ( 20.77549095910703869, -5.000000000000012434, -63.94038650157708759 ) ) ;
#29527 = ORIENTED_EDGE ( 'NONE', *, *, #3402, .T. ) ;
#29528 = ORIENTED_EDGE ( 'NONE', *, *, #16619, .F. ) ;
#29529 = FACE_OUTER_BOUND ( 'NONE', #21354, .T. ) ;
#29530 = AXIS2_PLACEMENT_3D ( 'NONE', #14054, #27703, #27409 ) ;
#29531 = CARTESIAN_POINT ( 'NONE',  ( 12.24591402697972775, 9.516428332920080280, -15.33268742708093235 ) ) ;
#29532 = CARTESIAN_POINT ( 'NONE',  ( 35.54859390953724585, -23.18451583373416014, -18.06010107863414405 ) ) ;
#29533 = EDGE_CURVE ( 'NONE', #22806, #29940, #6810, .T. ) ;
#29534 = ORIENTED_EDGE ( 'NONE', *, *, #14874, .F. ) ;
#29535 = CARTESIAN_POINT ( 'NONE',  ( 172.0152310637604103, -1.999999999999970468, -8.721423840594312082 ) ) ;
#29536 = CARTESIAN_POINT ( 'NONE',  ( 10.66768918063838179, 9.049215891674000645, -16.41161178408055932 ) ) ;
#29537 = CARTESIAN_POINT ( 'NONE',  ( 15.52722412259326745, -5.000000000000013323, -47.78788206013580009 ) ) ;
#29538 = CARTESIAN_POINT ( 'NONE',  ( 0.000000000000000000, 0.000000000000000000, 0.000000000000000000 ) ) ;
#29539 = EDGE_LOOP ( 'NONE', ( #24901, #11414, #24295, #16023 ) ) ;
#29540 = DIRECTION ( 'NONE',  ( -1.000000000000000000, 0.000000000000000000, 0.000000000000000000 ) ) ;
#29541 = ORIENTED_EDGE ( 'NONE', *, *, #17176, .F. ) ;
#29542 = CARTESIAN_POINT ( 'NONE',  ( 12.86662121207793241, 9.515397394723519753, -16.11672893869402756 ) ) ;
#29543 = VERTEX_POINT ( 'NONE', #16104 ) ;
#29544 = CARTESIAN_POINT ( 'NONE',  ( 34.52681913409613657, -13.10175273156466069, -19.97882978310374469 ) ) ;
#29545 = CARTESIAN_POINT ( 'NONE',  ( 21.43917814492346707, -4.799604530101110988, -17.97822123721208243 ) ) ;
#29546 = ORIENTED_EDGE ( 'NONE', *, *, #16103, .F. ) ;
#29547 = ORIENTED_EDGE ( 'NONE', *, *, #25839, .T. ) ;
#29548 = ORIENTED_EDGE ( 'NONE', *, *, #25662, .T. ) ;
#29549 = CARTESIAN_POINT ( 'NONE',  ( 8.000000000000003553, 4.618802153517037823, -4.285468820183664818 ) ) ;
#29550 = CARTESIAN_POINT ( 'NONE',  ( -4.000000000000005329, 0.7862748000877981536, -0.03447227762756752828 ) ) ;
#29551 = CARTESIAN_POINT ( 'NONE',  ( 174.7287565553229172, -1.999999999999968914, -25.16025403784440329 ) ) ;
#29552 =( NAMED_UNIT ( * ) PLANE_ANGLE_UNIT ( ) SI_UNIT ( $, .RADIAN. ) );
#29553 = CARTESIAN_POINT ( 'NONE',  ( 28.56881743257453721, -8.627791766613455593, -12.78522491232925873 ) ) ;
#29554 = CARTESIAN_POINT ( 'NONE',  ( 20.87485249991972580, -5.094386175754089585, -18.86169636093909219 ) ) ;
#29555 = VECTOR ( 'NONE', #7808, 1000.000000000000000 ) ;
#29556 = ORIENTED_EDGE ( 'NONE', *, *, #5635, .T. ) ;
#29557 = FACE_OUTER_BOUND ( 'NONE', #14918, .T. ) ;
#29558 = FACE_OUTER_BOUND ( 'NONE', #252, .T. ) ;
#29559 = DIRECTION ( 'NONE',  ( -2.698458740408365879E-16, 1.000000000000000000, 0.000000000000000000 ) ) ;
#29560 = AXIS2_PLACEMENT_3D ( 'NONE', #2579, #878, #28391 ) ;
#29561 = DIRECTION ( 'NONE',  ( -0.8090169943749474513, -2.183098979609982436E-16, 0.5877852522924731371 ) ) ;
#29562 = DIRECTION ( 'NONE',  ( -2.698458740408365879E-16, 1.000000000000000000, 0.000000000000000000 ) ) ;
#29563 = DIRECTION ( 'NONE',  ( -2.698458740408365879E-16, 1.000000000000000000, 0.000000000000000000 ) ) ;
#29564 = CARTESIAN_POINT ( 'NONE',  ( 10.89980385979276356, 10.57756405496316710, -17.37562731196375410 ) ) ;
#29565 = CARTESIAN_POINT ( 'NONE',  ( 12.23783994716398560, 8.515526397163364791, -15.33449341356891615 ) ) ;
#29566 = DIRECTION ( 'NONE',  ( -1.000000000000000000, 0.000000000000000000, 0.000000000000000000 ) ) ;
#29567 = EDGE_CURVE ( 'NONE', #7358, #23017, #13065, .T. ) ;
#29568 = EDGE_CURVE ( 'NONE', #8986, #6652, #1494, .T. ) ;
#29569 = DIRECTION ( 'NONE',  ( -2.698458740408365879E-16, 1.000000000000000000, 0.000000000000000000 ) ) ;
#29570 = DIRECTION ( 'NONE',  ( -2.698458740408365879E-16, 1.000000000000000000, 0.000000000000000000 ) ) ;
#29571 = VERTEX_POINT ( 'NONE', #29467 ) ;
#29572 = CARTESIAN_POINT ( 'NONE',  ( 9.641351338355821810, 17.66888872024471624, -17.91303689663363130 ) ) ;
#29573 = EDGE_CURVE ( 'NONE', #6973, #6726, #10607, .T. ) ;
#29574 = AXIS2_PLACEMENT_3D ( 'NONE', #28917, #6120, #15568 ) ;
#29575 = DIRECTION ( 'NONE',  ( -0.8090169943749474513, -2.183098979609982436E-16, -0.5877852522924731371 ) ) ;
#29576 = CARTESIAN_POINT ( 'NONE',  ( 120.0000000000000000, 20.00000000000000355, -186.4312945166758482 ) ) ;
#29577 = CARTESIAN_POINT ( 'NONE',  ( 167.0152310637604387, -4.999999999999972466, -8.721423840594312082 ) ) ;
#29578 = EDGE_CURVE ( 'NONE', #14185, #3020, #10923, .T. ) ;
#29579 = CARTESIAN_POINT ( 'NONE',  ( 26.80628776457338347, -3.176708023846821494, -16.02594779711905559 ) ) ;
#29580 = ORIENTED_EDGE ( 'NONE', *, *, #17582, .T. ) ;
#29581 = DIRECTION ( 'NONE',  ( 0.9510565162951536422, 2.566386769018988816E-16, 0.3090169943749472292 ) ) ;
#29582 = CARTESIAN_POINT ( 'NONE',  ( 12.24683531348137144, 9.516853939945930208, -15.33195173648645593 ) ) ;
#29583 = FACE_OUTER_BOUND ( 'NONE', #8966, .T. ) ;
#29584 = CARTESIAN_POINT ( 'NONE',  ( -4.000000000000003553, -1.933795701539603895, -0.2488376576622973180 ) ) ;
#29585 = CARTESIAN_POINT ( 'NONE',  ( 22.90372073960079646, -4.505259139820817715, -13.75793632099288111 ) ) ;
#29586 = LINE ( 'NONE', #15475, #8629 ) ;
#29587 = CARTESIAN_POINT ( 'NONE',  ( 23.04877348721027630, -0.9239720737610787049, -14.85003467231304342 ) ) ;
#29588 = ORIENTED_EDGE ( 'NONE', *, *, #21763, .F. ) ;
#29589 = CARTESIAN_POINT ( 'NONE',  ( 91.42100672702999020, -4.999999999999992895, 66.42124934025146388 ) ) ;
#29590 = ORIENTED_EDGE ( 'NONE', *, *, #19141, .F. ) ;
#29591 = AXIS2_PLACEMENT_3D ( 'NONE', #4657, #27597, #20983 ) ;
#29592 = VERTEX_POINT ( 'NONE', #13221 ) ;
#29593 = CARTESIAN_POINT ( 'NONE',  ( 17.25677449038176547, 8.733363079223632752, -20.54546673180767158 ) ) ;
#29594 = CARTESIAN_POINT ( 'NONE',  ( 30.09709056228524204, -9.598102759715754217, -17.07777997130633807 ) ) ;
#29595 = VECTOR ( 'NONE', #24417, 1000.000000000000000 ) ;
#29596 = ADVANCED_BREP_SHAPE_REPRESENTATION ( '', ( #21231, #13190 ), #3942 ) ;
#29597 = ORIENTED_EDGE ( 'NONE', *, *, #26323, .T. ) ;
#29598 = EDGE_LOOP ( 'NONE', ( #23624, #20636, #25358, #11923 ) ) ;
#29599 = CARTESIAN_POINT ( 'NONE',  ( 28.67486520862709654, -7.888541471525570614, -13.83454100519475105 ) ) ;
#29600 = VECTOR ( 'NONE', #3737, 1000.000000000000000 ) ;
#29601 = MECHANICAL_DESIGN_GEOMETRIC_PRESENTATION_REPRESENTATION (  '', ( #21227 ), #3209 ) ;
#29602 = CARTESIAN_POINT ( 'NONE',  ( 161.1922820468853104, -4.999999999999975131, -4.936203717676158398 ) ) ;
#29603 = ORIENTED_EDGE ( 'NONE', *, *, #4777, .F. ) ;
#29604 = CARTESIAN_POINT ( 'NONE',  ( 177.2287565553228887, -1.999999999999968470, -20.83012701892220520 ) ) ;
#29605 = VECTOR ( 'NONE', #19282, 1000.000000000000000 ) ;
#29606 = CARTESIAN_POINT ( 'NONE',  ( 74.18800000000001660, 0.000000000000000000, 0.000000000000000000 ) ) ;
#29607 = DIRECTION ( 'NONE',  ( 1.110223024625156540E-16, 2.995891024602366092E-32, 1.000000000000000000 ) ) ;
#29608 = CARTESIAN_POINT ( 'NONE',  ( 9.641350810849047548, 17.66889113945805789, -17.98596209335946128 ) ) ;
#29609 = CARTESIAN_POINT ( 'NONE',  ( 27.64917536653120678, -4.837437286474155052, -16.54522848743341967 ) ) ;
#29610 = CARTESIAN_POINT ( 'NONE',  ( 17.70500667399921824, 3.403337836861581867, -14.36321643528369663 ) ) ;
#29611 = CARTESIAN_POINT ( 'NONE',  ( 35.47777500975636400, -18.37389374556380517, -21.30860247919107664 ) ) ;
#29612 = LINE ( 'NONE', #17637, #1748 ) ;
#29613 = CARTESIAN_POINT ( 'NONE',  ( 11.47276097331165623, 9.269810413962238371, -15.86095999428340697 ) ) ;
#29614 = EDGE_CURVE ( 'NONE', #11825, #2371, #29620, .T. ) ;
#29615 = AXIS2_PLACEMENT_3D ( 'NONE', #19905, #8156, #6176 ) ;
#29616 = LINE ( 'NONE', #24679, #76 ) ;
#29617 = PLANE ( 'NONE',  #15366 ) ;
#29618 = ADVANCED_FACE ( 'NONE', ( #13516 ), #17935, .T. ) ;
#29619 = CARTESIAN_POINT ( 'NONE',  ( 13.12595734265553205, 8.571888915454989544, -15.91003987120930319 ) ) ;
#29620 = LINE ( 'NONE', #1643, #11201 ) ;
#29621 = CARTESIAN_POINT ( 'NONE',  ( 130.7287565553229172, -9.999999999999982236, -36.50000000000000711 ) ) ;
#29622 = CARTESIAN_POINT ( 'NONE',  ( 10.33811693838771717, 18.38618951776012267, -17.92454625180715411 ) ) ;
#29623 = ORIENTED_EDGE ( 'NONE', *, *, #28801, .T. ) ;
#29624 = VECTOR ( 'NONE', #24157, 1000.000000000000000 ) ;
#29625 = DIRECTION ( 'NONE',  ( -1.000000000000000000, 0.000000000000000000, 0.000000000000000000 ) ) ;
#29626 = CARTESIAN_POINT ( 'NONE',  ( 22.12891488531368367, -5.000000000000011546, -68.10579703808238605 ) ) ;
#29627 = AXIS2_PLACEMENT_3D ( 'NONE', #639, #15100, #23842 ) ;
#29628 = DIRECTION ( 'NONE',  ( -1.000000000000000000, 0.000000000000000000, -0.000000000000000000 ) ) ;
#29629 = ORIENTED_EDGE ( 'NONE', *, *, #19686, .F. ) ;
#29630 = CARTESIAN_POINT ( 'NONE',  ( 8.944605280299260386, 16.95149830073946617, -17.90242062344065843 ) ) ;
#29631 = CARTESIAN_POINT ( 'NONE',  ( 36.54742519285235858, -23.17926540875556896, -18.54852884019370762 ) ) ;
#29632 = CARTESIAN_POINT ( 'NONE',  ( 17.05458169553830317, 2.837819561348359887, -13.69156784695313611 ) ) ;
#29633 = CARTESIAN_POINT ( 'NONE',  ( 30.50670359208957905, -8.903545733563623443, -17.67935522427464079 ) ) ;
#29634 = DIRECTION ( 'NONE',  ( -0.5877852522924731371, -1.586114251531760728E-16, -0.8090169943749474513 ) ) ;
#29635 = LINE ( 'NONE', #27329, #12797 ) ;
#29636 = CARTESIAN_POINT ( 'NONE',  ( 27.48568275346891809, -3.109927088581168952, -18.71928346135984711 ) ) ;
#29637 = VECTOR ( 'NONE', #13157, 1000.000000000000000 ) ;
#29638 = ORIENTED_EDGE ( 'NONE', *, *, #6474, .T. ) ;
#29639 = DIRECTION ( 'NONE',  ( -0.8090169943749474513, -2.183098979609982436E-16, -0.5877852522924731371 ) ) ;
#29640 = LINE ( 'NONE', #6388, #29280 ) ;
#29641 = VECTOR ( 'NONE', #6552, 1000.000000000000000 ) ;
#29642 = DIRECTION ( 'NONE',  ( 1.000000000000000000, 0.000000000000000000, 0.000000000000000000 ) ) ;
#29643 = CARTESIAN_POINT ( 'NONE',  ( 131.1922820468854241, -1.999999999999981792, -19.40354224447947473 ) ) ;
#29644 = LINE ( 'NONE', #13976, #8759 ) ;
#29645 = CARTESIAN_POINT ( 'NONE',  ( 35.32370156268159178, -20.17419364810216109, -19.24765216636316723 ) ) ;
#29646 = VERTEX_POINT ( 'NONE', #2686 ) ;
#29647 = CARTESIAN_POINT ( 'NONE',  ( 10.83941243988239833, 8.530520621650927282, -16.32009337531726345 ) ) ;
#29648 = EDGE_LOOP ( 'NONE', ( #1773, #20909, #3034, #26164, #10509 ) ) ;
#29649 = EDGE_CURVE ( 'NONE', #8074, #20055, #26039, .T. ) ;
#29650 = EDGE_CURVE ( 'NONE', #24264, #22459, #29254, .T. ) ;
#29651 = CARTESIAN_POINT ( 'NONE',  ( 28.75197783424699693, -9.407057218516385433, -18.70835418409691542 ) ) ;
#29652 = EDGE_CURVE ( 'NONE', #25166, #9388, #16065, .T. ) ;
#29653 = CARTESIAN_POINT ( 'NONE',  ( 10.35864918915110877, 16.97212501191939538, -17.91752729848689185 ) ) ;
#29654 = FACE_OUTER_BOUND ( 'NONE', #21532, .T. ) ;
#29655 = EDGE_CURVE ( 'NONE', #1559, #7167, #12534, .T. ) ;
#29656 = VERTEX_POINT ( 'NONE', #10093 ) ;
#29657 = LINE ( 'NONE', #15234, #21237 ) ;
#29658 = VECTOR ( 'NONE', #27420, 1000.000000000000000 ) ;
#29659 = CARTESIAN_POINT ( 'NONE',  ( 12.50396148805030627, 8.572452836447732594, -15.12701763676990119 ) ) ;
#29660 = LINE ( 'NONE', #10818, #2339 ) ;
#29661 = PLANE ( 'NONE',  #27175 ) ;
#29662 = ORIENTED_EDGE ( 'NONE', *, *, #29650, .F. ) ;
#29663 = CARTESIAN_POINT ( 'NONE',  ( 9.661883062008595147, 16.25482663180050835, -17.91564816060341769 ) ) ;
#29664 = VECTOR ( 'NONE', #22965, 1000.000000000000000 ) ;
#29665 = CARTESIAN_POINT ( 'NONE',  ( 22.00422591904570879, -4.533096263764313072, -16.84388275221259690 ) ) ;
#29666 = CARTESIAN_POINT ( 'NONE',  ( 19.13824544459052035, 4.841912194177635520, -12.94453987625427160 ) ) ;
#29667 = ORIENTED_EDGE ( 'NONE', *, *, #14990, .F. ) ;
#29668 = DIRECTION ( 'NONE',  ( -0.9510565162951536422, -2.566386769018988323E-16, 0.3090169943749475623 ) ) ;
#29669 = CARTESIAN_POINT ( 'NONE',  ( 174.5152310637604387, -1.999999999999969580, -11.28819510263909542 ) ) ;
#29670 = VECTOR ( 'NONE', #6005, 1000.000000000000000 ) ;
#29671 = CARTESIAN_POINT ( 'NONE',  ( 20.24985932600369409, 3.694099309552050237, -20.13309853732883781 ) ) ;
#29672 = VERTEX_POINT ( 'NONE', #24302 ) ;
#29673 = LINE ( 'NONE', #24894, #336 ) ;
#29674 = DIRECTION ( 'NONE',  ( -0.8090169943749474513, -2.183098979609982436E-16, 0.5877852522924731371 ) ) ;
#29675 = AXIS2_PLACEMENT_3D ( 'NONE', #22073, #3606, #19470 ) ;
#29676 = ORIENTED_EDGE ( 'NONE', *, *, #3406, .F. ) ;
#29677 = FACE_OUTER_BOUND ( 'NONE', #7522, .T. ) ;
#29678 = CARTESIAN_POINT ( 'NONE',  ( 33.38708106686501509, -12.47399286361455850, -19.70456970583452616 ) ) ;
#29679 = DIRECTION ( 'NONE',  ( 1.000000000000000000, 0.000000000000000000, 0.000000000000000000 ) ) ;
#29680 = AXIS2_PLACEMENT_3D ( 'NONE', #19532, #17245, #8230 ) ;
#29681 = ORIENTED_EDGE ( 'NONE', *, *, #23879, .F. ) ;
#29682 = ORIENTED_EDGE ( 'NONE', *, *, #27554, .F. ) ;
#29683 = CARTESIAN_POINT ( 'NONE',  ( 132.0152310637605808, -4.999999999999982236, 1.702185954127501066 ) ) ;
#29684 = CARTESIAN_POINT ( 'NONE',  ( 17.78594395145776019, 10.14170102421038422, -17.68001733040774681 ) ) ;
#29685 = CARTESIAN_POINT ( 'NONE',  ( 12.24853674868645292, 9.517605834602926862, -15.33059566259575668 ) ) ;
#29686 = CARTESIAN_POINT ( 'NONE',  ( 35.54859215833182873, -22.18450796649496226, -18.40462262104107083 ) ) ;
#29687 = EDGE_CURVE ( 'NONE', #12877, #10296, #3259, .T. ) ;
#29688 = VECTOR ( 'NONE', #14954, 1000.000000000000000 ) ;
#29689 = VERTEX_POINT ( 'NONE', #7669 ) ;
#29690 = CARTESIAN_POINT ( 'NONE',  ( 9.641350810849047548, 17.66889113945805789, -17.97192418671891190 ) ) ;
#29691 = CARTESIAN_POINT ( 'NONE',  ( 12.78320632028979809, 7.637826363492710158, -14.90445457646871574 ) ) ;
#29692 = PLANE ( 'NONE',  #12221 ) ;
#29693 = CARTESIAN_POINT ( 'NONE',  ( 159.5152310637604387, -10.00000000000000000, -4.391296821672111328 ) ) ;
#29694 = ORIENTED_EDGE ( 'NONE', *, *, #5154, .F. ) ;
#29695 = LINE ( 'NONE', #18024, #12022 ) ;
#29696 = VERTEX_POINT ( 'NONE', #3114 ) ;
#29697 = CARTESIAN_POINT ( 'NONE',  ( 10.35864918915110877, 16.97212501191939538, -23.00000000000000711 ) ) ;
#29698 = CARTESIAN_POINT ( 'NONE',  ( 36.54859497913844990, -21.18452063888661385, -18.28382709584098720 ) ) ;
#29699 = CARTESIAN_POINT ( 'NONE',  ( 21.10023079691774228, -0.4353598523292347422, -20.14113737667230097 ) ) ;
#29700 = ORIENTED_EDGE ( 'NONE', *, *, #8754, .T. ) ;
#29701 = VECTOR ( 'NONE', #17774, 1000.000000000000000 ) ;
#29702 = PLANE ( 'NONE',  #29182 ) ;
#29703 = DIRECTION ( 'NONE',  ( 1.110223024625156540E-16, 2.995891024602366092E-32, 1.000000000000000000 ) ) ;
#29704 = DIRECTION ( 'NONE',  ( 0.000000000000000000, -1.000000000000000000, 0.000000000000000000 ) ) ;
#29705 =( NAMED_UNIT ( * ) PLANE_ANGLE_UNIT ( ) SI_UNIT ( $, .RADIAN. ) );
#29706 = CARTESIAN_POINT ( 'NONE',  ( 25.66600519952783799, -8.909200411882650883, -19.30012332941604924 ) ) ;
#29707 = AXIS2_PLACEMENT_3D ( 'NONE', #26237, #24391, #5317 ) ;
#29708 = CARTESIAN_POINT ( 'NONE',  ( 21.64995824428719828, -4.359751022247916552, -19.89060884261010287 ) ) ;
#29709 = ORIENTED_EDGE ( 'NONE', *, *, #2896, .F. ) ;
#29710 = VERTEX_POINT ( 'NONE', #12387 ) ;
#29711 = EDGE_CURVE ( 'NONE', #7341, #11438, #3396, .T. ) ;
#29712 = DIRECTION ( 'NONE',  ( 0.000000000000000000, 0.000000000000000000, -1.000000000000000000 ) ) ;
#29713 = VECTOR ( 'NONE', #21051, 1000.000000000000000 ) ;
#29714 = DIRECTION ( 'NONE',  ( 0.000000000000000000, 2.775557561562890735E-17, -1.000000000000000000 ) ) ;
#29715 = CARTESIAN_POINT ( 'NONE',  ( 168.6922820468853104, -4.999999999999972466, -6.413161187712876909 ) ) ;
#29716 = DIRECTION ( 'NONE',  ( 0.5840962589317576503, -0.8116843969807016057, 0.000000000000000000 ) ) ;
#29717 = DIRECTION ( 'NONE',  ( 1.000000000000000000, 4.440892098500622217E-16, 0.000000000000000000 ) ) ;
#29718 = VECTOR ( 'NONE', #21363, 1000.000000000000000 ) ;
#29719 = UNCERTAINTY_MEASURE_WITH_UNIT (LENGTH_MEASURE( 1.000000000000000082E-05 ), #12587, 'distance_accuracy_value', 'NONE');
#29720 = CARTESIAN_POINT ( 'NONE',  ( 11.22336320048417591, 9.093679674329528950, -17.24182414271593800 ) ) ;
#29721 = CARTESIAN_POINT ( 'NONE',  ( 10.33811693838771717, 18.38618951776012267, -17.95086732675816776 ) ) ;
#29722 = DIRECTION ( 'NONE',  ( -2.698458740408365879E-16, 1.000000000000000000, 0.000000000000000000 ) ) ;
#29723 = VERTEX_POINT ( 'NONE', #26153 ) ;
#29724 = LINE ( 'NONE', #6317, #27630 ) ;
#29725 = VECTOR ( 'NONE', #13027, 1000.000000000000000 ) ;
#29726 = PLANE ( 'NONE',  #11522 ) ;
#29727 = ORIENTED_EDGE ( 'NONE', *, *, #24466, .F. ) ;
#29728 = CARTESIAN_POINT ( 'NONE',  ( 9.776119957569173735, 17.05082265352876547, -16.72288386497739765 ) ) ;
#29729 = LINE ( 'NONE', #18927, #12085 ) ;
#29730 = CARTESIAN_POINT ( 'NONE',  ( 15.83821057800014920, 6.120979864746498578, -15.70533851924537672 ) ) ;
#29731 = DIRECTION ( 'NONE',  ( -1.779203565104417375E-16, -4.801107411221739977E-32, -1.000000000000000000 ) ) ;
#29732 = LINE ( 'NONE', #1907, #2072 ) ;
#29734 = VERTEX_POINT ( 'NONE', #10244 ) ;
#29733 = CARTESIAN_POINT ( 'NONE',  ( 21.18945582756405344, -5.194394521544061227, -16.21196392551894405 ) ) ;
#29735 = AXIS2_PLACEMENT_3D ( 'NONE', #17214, #14602, #14756 ) ;
#29736 = EDGE_LOOP ( 'NONE', ( #17274, #17502, #1872, #7065 ) ) ;
#29737 = CARTESIAN_POINT ( 'NONE',  ( 2.500000000000000444, 1.110223024625155752E-15, -2.450000000000000622 ) ) ;
#29738 = CARTESIAN_POINT ( 'NONE',  ( 11.05541531668977662, 17.68942339022145305, -17.91664992932185996 ) ) ;
#29739 = AXIS2_PLACEMENT_3D ( 'NONE', #6802, #20522, #16091 ) ;
#29740 = CARTESIAN_POINT ( 'NONE',  ( 35.54287943964028784, -22.15884374752674546, -18.65915260879160797 ) ) ;
#29741 = DIRECTION ( 'NONE',  ( 0.9510565162951536422, 0.000000000000000000, -0.3090169943749475623 ) ) ;
#29742 = CARTESIAN_POINT ( 'NONE',  ( 23.56138260001205964, -6.829566487537672259, -18.05074380722902916 ) ) ;
#29743 = CARTESIAN_POINT ( 'NONE',  ( 142.0152310637605240, -10.00000000000000533, -0.06116980274991495881 ) ) ;
#29744 = CARTESIAN_POINT ( 'NONE',  ( 21.68595642006795288, -3.720678421232956445, -15.48850127590278980 ) ) ;
#29745 = ORIENTED_EDGE ( 'NONE', *, *, #10485, .T. ) ;
#29746 = FACE_OUTER_BOUND ( 'NONE', #1112, .T. ) ;
#29747 =( LENGTH_UNIT ( ) NAMED_UNIT ( * ) SI_UNIT ( .MILLI., .METRE. ) );
#29748 = CARTESIAN_POINT ( 'NONE',  ( 14.50439321891314925, 5.533609182599570353, -15.17065254761420512 ) ) ;
#29749 = CARTESIAN_POINT ( 'NONE',  ( 29.53935142057454755, -5.962610374456907003, -16.12847026952743690 ) ) ;
#29750 = ORIENTED_EDGE ( 'NONE', *, *, #21721, .T. ) ;
#29751 = EDGE_CURVE ( 'NONE', #30179, #9897, #26301, .T. ) ;
#29752 = ADVANCED_FACE ( 'NONE', ( #14818 ), #26454, .T. ) ;
#29753 = FACE_OUTER_BOUND ( 'NONE', #1472, .T. ) ;
#29754 = ADVANCED_FACE ( 'NONE', ( #14671 ), #9801, .T. ) ;
#29755 = PLANE ( 'NONE',  #28492 ) ;
#29756 = AXIS2_PLACEMENT_3D ( 'NONE', #1361, #26398, #10649 ) ;
#29757 = EDGE_LOOP ( 'NONE', ( #19553, #13981, #20299, #23094 ) ) ;
#29758 = DIRECTION ( 'NONE',  ( -0.9510565162951536422, -2.566386769018988816E-16, -0.3090169943749472292 ) ) ;
#29759 = CARTESIAN_POINT ( 'NONE',  ( 133.7287565553229172, -9.999999999999982236, -36.50000000000000711 ) ) ;
#29760 = CARTESIAN_POINT ( 'NONE',  ( 420.0000000000002274, 27.64101615137744972, 10.00000000000000178 ) ) ;
#29761 = DIRECTION ( 'NONE',  ( -2.698458740408365879E-16, 1.000000000000000000, 0.000000000000000000 ) ) ;
#29762 = CARTESIAN_POINT ( 'NONE',  ( 26.11288949521356528, -6.777652795969290267, -18.96966820991230662 ) ) ;
#29763 = CARTESIAN_POINT ( 'NONE',  ( 14.30110556002302680, 5.443193088601498530, -15.49285935407157666 ) ) ;
#29764 = CARTESIAN_POINT ( 'NONE',  ( 35.74526169011073762, -19.57556970876266433, -21.38945728569726867 ) ) ;
#29765 = CARTESIAN_POINT ( 'NONE',  ( 15.00000000000000000, 0.000000000000000000, 0.000000000000000000 ) ) ;
#29766 = CARTESIAN_POINT ( 'NONE',  ( 12.49957999542663600, 8.570517509188613658, -15.13050969259218981 ) ) ;
#29767 = FACE_OUTER_BOUND ( 'NONE', #18261, .T. ) ;
#29768 = DIRECTION ( 'NONE',  ( -1.000000000000000000, -0.000000000000000000, -0.000000000000000000 ) ) ;
#29769 = CARTESIAN_POINT ( 'NONE',  ( 9.684081875198721434, 16.15302004482010645, -17.87837111813898616 ) ) ;
#29770 = CARTESIAN_POINT ( 'NONE',  ( 147.0152310637605240, -10.00000000000000178, -8.721423840594312082 ) ) ;
#29771 = VERTEX_POINT ( 'NONE', #21699 ) ;
#29772 = CARTESIAN_POINT ( 'NONE',  ( 63.44486372867152824, 109.8897274573438096, -17.99999999999998934 ) ) ;
#29773 = CARTESIAN_POINT ( 'NONE',  ( 12.49899259368311988, 8.570259324921714494, -15.13097775544467005 ) ) ;
#29774 = VERTEX_POINT ( 'NONE', #19115 ) ;
#29775 = VECTOR ( 'NONE', #16506, 1000.000000000000000 ) ;
#29776 = LINE ( 'NONE', #6516, #3248 ) ;
#29777 = LINE ( 'NONE', #25284, #9792 ) ;
#29778 = DIRECTION ( 'NONE',  ( -1.110223024625156540E-16, 0.000000000000000000, -1.000000000000000000 ) ) ;
#29779 = AXIS2_PLACEMENT_3D ( 'NONE', #2705, #21153, #572 ) ;
#29780 = VERTEX_POINT ( 'NONE', #5228 ) ;
#29781 = CARTESIAN_POINT ( 'NONE',  ( 13.38776246403941350, 7.629555522264023892, -15.70137656829213491 ) ) ;
#29782 = CARTESIAN_POINT ( 'NONE',  ( 35.79875902618127270, -19.81590490140210647, -21.40562824699871314 ) ) ;
#29783 = CARTESIAN_POINT ( 'NONE',  ( 21.20591713499851849, 2.664298913801621538, -19.97344039048299891 ) ) ;
#29784 = CARTESIAN_POINT ( 'NONE',  ( 30.50415327504139285, -11.36213899161910135, -13.19862950667920565 ) ) ;
#29785 = CARTESIAN_POINT ( 'NONE',  ( 158.6922820468853104, -10.00000000000000000, -0.6060766987539614181 ) ) ;
#29786 = DIRECTION ( 'NONE',  ( -0.5877852522924731371, -1.586114251531760728E-16, -0.8090169943749474513 ) ) ;
#29787 = CARTESIAN_POINT ( 'NONE',  ( 21.21264933382939333, -0.1440395243212932441, -13.28659446924270959 ) ) ;
#29788 = ADVANCED_FACE ( 'NONE', ( #28927 ), #2963, .T. ) ;
#29789 = ADVANCED_FACE ( 'NONE', ( #28470 ), #21559, .T. ) ;
#29790 = EDGE_LOOP ( 'NONE', ( #8665, #15614, #29037, #14933, #18002 ) ) ;
#29791 = ADVANCED_FACE ( 'NONE', ( #17127 ), #22012, .T. ) ;
#29792 = DIRECTION ( 'NONE',  ( 0.9510565162951536422, 2.566386769018988816E-16, 0.3090169943749472292 ) ) ;
#29793 = ORIENTED_EDGE ( 'NONE', *, *, #9796, .F. ) ;
#29794 = PLANE ( 'NONE',  #24287 ) ;
#29795 = VECTOR ( 'NONE', #5342, 1000.000000000000000 ) ;
#29797 = ORIENTED_EDGE ( 'NONE', *, *, #27005, .F. ) ;
#29796 = CARTESIAN_POINT ( 'NONE',  ( 31.84774147790582433, -10.54213090804960018, -15.00000000011102763 ) ) ;
#29798 = LINE ( 'NONE', #27178, #2978 ) ;
#29799 = DIRECTION ( 'NONE',  ( -0.5877852522924731371, 0.000000000000000000, 0.8090169943749474513 ) ) ;
#29800 = AXIS2_PLACEMENT_3D ( 'NONE', #28681, #21468, #7284 ) ;
#29801 = AXIS2_PLACEMENT_3D ( 'NONE', #13051, #10767, #22375 ) ;
#29802 = CARTESIAN_POINT ( 'NONE',  ( 133.7287565553229740, -84.33034373659253902, 8.500000000000007105 ) ) ;
#29803 = CARTESIAN_POINT ( 'NONE',  ( 33.33106278064285277, -11.02967194543584029, -16.07471553095689742 ) ) ;
#29804 = EDGE_LOOP ( 'NONE', ( #6218, #25668, #22918, #4919, #4108 ) ) ;
#29805 = CARTESIAN_POINT ( 'NONE',  ( 10.66844579733420062, 9.045745945026473223, -16.41129889692150812 ) ) ;
#29806 = ORIENTED_EDGE ( 'NONE', *, *, #20685, .T. ) ;
#29807 = CARTESIAN_POINT ( 'NONE',  ( 31.81434894052502571, -10.04473835610349575, -15.03854332269495764 ) ) ;
#29808 = CARTESIAN_POINT ( 'NONE',  ( 0.000000000000000000, 0.000000000000000000, -18.00000000000000000 ) ) ;
#29809 = CARTESIAN_POINT ( 'NONE',  ( 10.35864918915110877, 16.97212501191939538, -17.92279151347709032 ) ) ;
#29810 = CARTESIAN_POINT ( 'NONE',  ( 4.000000000000003553, 2.309401076758525573, -0.3572655899081716435 ) ) ;
#29811 = ORIENTED_EDGE ( 'NONE', *, *, #18976, .F. ) ;
#29812 = VECTOR ( 'NONE', #23903, 1000.000000000000000 ) ;
#29813 = DIRECTION ( 'NONE',  ( -0.9510565162951536422, -2.566386769018988816E-16, -0.3090169943749472292 ) ) ;
#29814 = CARTESIAN_POINT ( 'NONE',  ( 152.0152310637605808, -10.00000000000000000, -24.27857615940569502 ) ) ;
#29816 = ORIENTED_EDGE ( 'NONE', *, *, #951, .T. ) ;
#29815 = CARTESIAN_POINT ( 'NONE',  ( 173.6922820468853104, -4.999999999999970690, -15.07341522555727664 ) ) ;
#29817 = EDGE_LOOP ( 'NONE', ( #837, #23505, #11488, #10907 ) ) ;
#29818 = DIRECTION ( 'NONE',  ( 0.000000000000000000, 0.000000000000000000, 1.000000000000000000 ) ) ;
#29819 = ORIENTED_EDGE ( 'NONE', *, *, #10695, .F. ) ;
#29820 = CARTESIAN_POINT ( 'NONE',  ( 13.12808413666193275, 8.572828783776230921, -15.90834477884588516 ) ) ;
#29821 = VECTOR ( 'NONE', #1791, 1000.000000000000000 ) ;
#29822 = CARTESIAN_POINT ( 'NONE',  ( 22.09051738352356153, 1.573095004317974333, -13.27920415769822426 ) ) ;
#29823 = CARTESIAN_POINT ( 'NONE',  ( 22.68697051328012293, -3.855329871767240402, -18.23939831819710733 ) ) ;
#29824 = ORIENTED_EDGE ( 'NONE', *, *, #16549, .T. ) ;
#29825 = CARTESIAN_POINT ( 'NONE',  ( 17.94193213664724951, 0.5400182743772068417, -16.55803501089447849 ) ) ;
#29826 = CARTESIAN_POINT ( 'NONE',  ( -20.00000000000017053, 34.64101615137744972, 9.999999999999998224 ) ) ;
#29827 = CARTESIAN_POINT ( 'NONE',  ( 133.7287565553229172, -4.999999999999982236, -33.50000000000000000 ) ) ;
#29828 = CARTESIAN_POINT ( 'NONE',  ( 18.98200677837107264, -2.562081333921657933, -16.63161468174866187 ) ) ;
#29829 = EDGE_CURVE ( 'NONE', #9909, #3561, #962, .T. ) ;
#29830 = EDGE_CURVE ( 'NONE', #23305, #25136, #7806, .T. ) ;
#29831 = EDGE_CURVE ( 'NONE', #17674, #30043, #28612, .T. ) ;
#29832 = CARTESIAN_POINT ( 'NONE',  ( 175.7287565553229456, -4.999999999999970690, -33.50000000000000000 ) ) ;
#29833 = ADVANCED_FACE ( 'NONE', ( #6877 ), #11574, .T. ) ;
#29834 = AXIS2_PLACEMENT_3D ( 'NONE', #6373, #16113, #8494 ) ;
#29835 = PLANE ( 'NONE',  #4523 ) ;
#29836 = VECTOR ( 'NONE', #2168, 1000.000000000000000 ) ;
#29837 = EDGE_LOOP ( 'NONE', ( #26958, #673, #29590, #21212 ) ) ;
#29838 = CARTESIAN_POINT ( 'NONE',  ( 10.35864940629342890, 16.97212401607702148, -17.91464645457531191 ) ) ;
#29839 = CARTESIAN_POINT ( 'NONE',  ( 167.2287565553228887, -1.999999999999971800, -3.509618943233403510 ) ) ;
#29840 = CARTESIAN_POINT ( 'NONE',  ( 2.500000000000000444, 0.000000000000000000, 0.000000000000000000 ) ) ;
#29841 = ORIENTED_EDGE ( 'NONE', *, *, #3068, .F. ) ;
#29842 = CARTESIAN_POINT ( 'NONE',  ( 172.0152310637603819, -4.999999999999970690, -1.909752701132032347E-14 ) ) ;
#29843 = CARTESIAN_POINT ( 'NONE',  ( 18.76632379254337835, 6.868107169226369102, -19.55161205380106892 ) ) ;
#29844 = CARTESIAN_POINT ( 'NONE',  ( 12.25193961909737794, 9.519109623917222152, -15.32788351481347355 ) ) ;
#29845 = CARTESIAN_POINT ( 'NONE',  ( 35.54859390953724585, -22.18451583373416014, -17.64281456791166036 ) ) ;
#29846 = ORIENTED_EDGE ( 'NONE', *, *, #17440, .F. ) ;
#29847 = CARTESIAN_POINT ( 'NONE',  ( 172.0152310637604103, -9.999999999999996447, 1.702185954127501066 ) ) ;
#29848 = CARTESIAN_POINT ( 'NONE',  ( 9.641350810849047548, 17.66889113945805789, -17.91752729848689185 ) ) ;
#29849 = LINE ( 'NONE', #11303, #29339 ) ;
#29850 =( NAMED_UNIT ( * ) PLANE_ANGLE_UNIT ( ) SI_UNIT ( $, .RADIAN. ) );
#29851 = EDGE_LOOP ( 'NONE', ( #21661, #11181, #15080, #23310 ) ) ;
#29852 = CARTESIAN_POINT ( 'NONE',  ( 95.60450572449933304, -4.999999999999991118, -69.46073927778073198 ) ) ;
#29853 = VERTEX_POINT ( 'NONE', #603 ) ;
#29854 = CARTESIAN_POINT ( 'NONE',  ( 10.35864918915110877, 16.97212501191939538, -17.95086732675817132 ) ) ;
#29856 = VECTOR ( 'NONE', #19918, 1000.000000000000000 ) ;
#29855 = CARTESIAN_POINT ( 'NONE',  ( 36.54859390953724585, -21.18451583373416014, -17.78191007148576119 ) ) ;
#29857 = CARTESIAN_POINT ( 'NONE',  ( 22.97938783112199701, -3.359759438970757017, -19.62490732200095067 ) ) ;
#29858 = FACE_OUTER_BOUND ( 'NONE', #9073, .T. ) ;
#29859 = CARTESIAN_POINT ( 'NONE',  ( -5.000000000000000000, 0.000000000000000000, 23.00000000000000000 ) ) ;
#29860 = DIRECTION ( 'NONE',  ( 0.000000000000000000, 0.000000000000000000, 1.000000000000000000 ) ) ;
#29861 = COLOUR_RGB ( '', 0.09019608, 0.27058824, 0.51372549) ;
#29862 = CARTESIAN_POINT ( 'NONE',  ( 23.72517123929712213, -5.798560033841243744, -19.46542475990168342 ) ) ;
#29863 = CARTESIAN_POINT ( 'NONE',  ( 27.35978538551520245, -3.059420540688277956, -14.62525642202852971 ) ) ;
#29864 = EDGE_CURVE ( 'NONE', #21320, #15396, #16166, .T. ) ;
#29865 = ADVANCED_FACE ( 'NONE', ( #12032 ), #28264, .T. ) ;
#29867 = ORIENTED_EDGE ( 'NONE', *, *, #20621, .F. ) ;
#29866 = EDGE_CURVE ( 'NONE', #21590, #25250, #152, .T. ) ;
#29868 = LINE ( 'NONE', #11612, #10810 ) ;
#29869 = VECTOR ( 'NONE', #2092, 1000.000000000000000 ) ;
#29870 = DIRECTION ( 'NONE',  ( 2.207829878515935943E-16, 1.000000000000000000, 0.000000000000000000 ) ) ;
#29871 = LINE ( 'NONE', #13459, #11160 ) ;
#29872 = VECTOR ( 'NONE', #2284, 1000.000000000000000 ) ;
#29873 = CARTESIAN_POINT ( 'NONE',  ( 169.7287565553229456, -9.999999999999996447, -25.16025403784440329 ) ) ;
#29874 = CARTESIAN_POINT ( 'NONE',  ( 12.50736435846123484, 8.573956625762026107, -15.12430548898761806 ) ) ;
#29875 = LINE ( 'NONE', #20487, #24372 ) ;
#29876 = EDGE_LOOP ( 'NONE', ( #9550, #12844, #696, #9152 ) ) ;
#29877 = FACE_OUTER_BOUND ( 'NONE', #15912, .T. ) ;
#29878 = ORIENTED_EDGE ( 'NONE', *, *, #28278, .F. ) ;
#29879 = CARTESIAN_POINT ( 'NONE',  ( 9.870716668364401869, 16.61699007954640805, -16.53972800451630931 ) ) ;
#29880 = CARTESIAN_POINT ( 'NONE',  ( 17.26923406770577074, 6.766716122889627094, -15.27140832040383422 ) ) ;
#29881 = CARTESIAN_POINT ( 'NONE',  ( 163.6922820468853956, -1.999999999999972689, -32.39392330124607611 ) ) ;
#29882 = FACE_OUTER_BOUND ( 'NONE', #29084, .T. ) ;
#29884 = VERTEX_POINT ( 'NONE', #23646 ) ;
#29883 = CARTESIAN_POINT ( 'NONE',  ( 23.21730923944814506, -4.364887171357101359, -13.63095412955673247 ) ) ;
#29885 = ORIENTED_EDGE ( 'NONE', *, *, #26528, .T. ) ;
#29886 = DIRECTION ( 'NONE',  ( 0.5877852522924731371, 1.586114251531760728E-16, 0.8090169943749474513 ) ) ;
#29887 = CARTESIAN_POINT ( 'NONE',  ( 11.05541529015696156, 17.68942351190433726, -17.91624098666951070 ) ) ;
#29888 = EDGE_CURVE ( 'NONE', #7982, #18285, #2746, .T. ) ;
#29889 = CARTESIAN_POINT ( 'NONE',  ( 32.01580575020638975, -11.60503005433848500, -14.58926670671732673 ) ) ;
#29890 = DIRECTION ( 'NONE',  ( 0.3090169943749475623, 8.338696094058001131E-17, 0.9510565162951536422 ) ) ;
#29891 = CARTESIAN_POINT ( 'NONE',  ( 26.80628776457338347, -3.176708023846821494, -16.02594779711905559 ) ) ;
#29892 = CARTESIAN_POINT ( 'NONE',  ( 8.000000000000003553, 4.618802153517037823, -4.285468820183664818 ) ) ;
#29893 = CARTESIAN_POINT ( 'NONE',  ( 21.61496389699315657, -3.514534563429178249, -17.40323974765788506 ) ) ;
#29894 = ORIENTED_EDGE ( 'NONE', *, *, #6123, .F. ) ;
#29895 = DIRECTION ( 'NONE',  ( 0.3090169943749472292, 8.338696094057992503E-17, -0.9510565162951536422 ) ) ;
#29896 = FILL_AREA_STYLE_COLOUR ( '', #9290 ) ;
#29897 = CARTESIAN_POINT ( 'NONE',  ( 18.47844294452917424, 10.16049799425131361, -18.92511192449534718 ) ) ;
#29898 = CARTESIAN_POINT ( 'NONE',  ( 28.24905293252005123, -11.45655955306129314, -17.88756844200554141 ) ) ;
#29899 = EDGE_LOOP ( 'NONE', ( #9700, #7176, #10274, #628 ) ) ;
#29900 = ORIENTED_EDGE ( 'NONE', *, *, #11030, .F. ) ;
#29901 = LINE ( 'NONE', #23117, #23414 ) ;
#29902 = PRODUCT_DEFINITION_SHAPE ( 'NONE', 'NONE',  #30264 ) ;
#29903 = ORIENTED_EDGE ( 'NONE', *, *, #28694, .F. ) ;
#29904 = LINE ( 'NONE', #18534, #19654 ) ;
#29905 = CARTESIAN_POINT ( 'NONE',  ( 173.6922820468852535, -9.999999999999996447, -0.6060766987539614181 ) ) ;
#29906 = CARTESIAN_POINT ( 'NONE',  ( 163.6922820468853388, -1.999999999999972689, -15.07341522555727664 ) ) ;
#29907 = DIRECTION ( 'NONE',  ( 1.000000000000000000, 0.000000000000000000, 0.000000000000000000 ) ) ;
#29908 = AXIS2_PLACEMENT_3D ( 'NONE', #24169, #24316, #3411 ) ;
#29909 = LINE ( 'NONE', #27589, #24802 ) ;
#29910 = CARTESIAN_POINT ( 'NONE',  ( 25.51539342332723947, -8.447981945391376257, -12.99903862581394876 ) ) ;
#29911 = CARTESIAN_POINT ( 'NONE',  ( 20.41927524488895429, 4.553956414902842198, -14.69105443414393264 ) ) ;
#29912 = CARTESIAN_POINT ( 'NONE',  ( 35.81175537756147520, -19.87429062379433731, -21.40957262365663993 ) ) ;
#29913 = CARTESIAN_POINT ( 'NONE',  ( 141.1922820468854525, -4.999999999999980460, -30.91696583120935671 ) ) ;
#29914 = CARTESIAN_POINT ( 'NONE',  ( 12.49860086554322436, 8.570087612320898884, -15.13128986298120537 ) ) ;
#29915 = DIRECTION ( 'NONE',  ( 0.5877852522924731371, 1.586114251531760728E-16, 0.8090169943749474513 ) ) ;
#29916 = DIRECTION ( 'NONE',  ( -1.110223024625156540E-16, 0.000000000000000000, -1.000000000000000000 ) ) ;
#29917 = CARTESIAN_POINT ( 'NONE',  ( 9.668505437271095460, 16.22445557469016464, -17.88481252315560965 ) ) ;
#29919 = VERTEX_POINT ( 'NONE', #25627 ) ;
#29918 = CARTESIAN_POINT ( 'NONE',  ( 146.1922820468854525, -10.00000000000000178, -28.06379628232387446 ) ) ;
#29920 = VERTEX_POINT ( 'NONE', #5019 ) ;
#29921 = FACE_OUTER_BOUND ( 'NONE', #11208, .T. ) ;
#29922 = CARTESIAN_POINT ( 'NONE',  ( 10.33811693838771717, 18.38618951776012267, -17.98596209335946128 ) ) ;
#29923 = ADVANCED_FACE ( 'NONE', ( #28414 ), #4718, .T. ) ;
#29924 = VERTEX_POINT ( 'NONE', #16620 ) ;
#29925 = LINE ( 'NONE', #20537, #12475 ) ;
#29926 = CARTESIAN_POINT ( 'NONE',  ( 96.27478563531609268, -4.999999999999991118, 69.94772613865674771 ) ) ;
#29927 = EDGE_CURVE ( 'NONE', #14621, #6718, #6358, .T. ) ;
#29928 = AXIS2_PLACEMENT_3D ( 'NONE', #28261, #28411, #14005 ) ;
#29929 = CARTESIAN_POINT ( 'NONE',  ( 14.93287775521291394, 9.378568215907955974, -14.88591063491414168 ) ) ;
#29930 = ORIENTED_EDGE ( 'NONE', *, *, #22279, .F. ) ;
#29931 = CARTESIAN_POINT ( 'NONE',  ( 9.242255153701981030, 15.58643803978083753, -17.00107889682120899 ) ) ;
#29932 = CARTESIAN_POINT ( 'NONE',  ( 34.70640263809442416, -19.40099657226499019, -21.14569589167440000 ) ) ;
#29933 = CARTESIAN_POINT ( 'NONE',  ( 22.65699622776610411, 4.567421951779635947, -17.29570926971318556 ) ) ;
#29934 = CARTESIAN_POINT ( 'NONE',  ( 18.96102019896426683, 9.324696518442671334, -18.66317648627137515 ) ) ;
#29935 = VECTOR ( 'NONE', #26473, 1000.000000000000000 ) ;
#29936 = CARTESIAN_POINT ( 'NONE',  ( -2.644994884459112683, 7.710515798486376582, -4.917753204360280961 ) ) ;
#29937 = CARTESIAN_POINT ( 'NONE',  ( 27.86916612644401425, -2.348388412649441648, -16.97020329177912501 ) ) ;
#29938 = VERTEX_POINT ( 'NONE', #9739 ) ;
#29939 = CARTESIAN_POINT ( 'NONE',  ( 136.1922820468854241, -10.00000000000000533, -4.936203717676158398 ) ) ;
#29940 = VERTEX_POINT ( 'NONE', #19058 ) ;
#29941 = DIRECTION ( 'NONE',  ( -0.8090169943749474513, -2.183098979609982436E-16, 0.5877852522924731371 ) ) ;
#29942 = DIRECTION ( 'NONE',  ( 0.5877852522924731371, 0.000000000000000000, 0.8090169943749474513 ) ) ;
#29943 = ORIENTED_EDGE ( 'NONE', *, *, #11317, .T. ) ;
#29944 = CARTESIAN_POINT ( 'NONE',  ( 33.94960473074984009, -11.12362044852780407, -17.82291586202971700 ) ) ;
#29945 = CARTESIAN_POINT ( 'NONE',  ( 10.65857126575392400, 9.091031811597934720, -16.41538236262689310 ) ) ;
#29946 = VERTEX_POINT ( 'NONE', #7467 ) ;
#29947 = AXIS2_PLACEMENT_3D ( 'NONE', #19617, #417, #8018 ) ;
#29948 = CARTESIAN_POINT ( 'NONE',  ( 26.92971693216691165, -8.617903733377630715, -13.36642543767191427 ) ) ;
#29949 = CARTESIAN_POINT ( 'NONE',  ( -7.372574772901430151E-15, -9.237604307034054330, -5.000000000000000888 ) ) ;
#29950 = CARTESIAN_POINT ( 'NONE',  ( 11.12037835888041393, 13.47873794165536410, -17.06668569338069830 ) ) ;
#29951 = LINE ( 'NONE', #8819, #20931 ) ;
#29952 = CARTESIAN_POINT ( 'NONE',  ( 167.0152310637605240, -9.999999999999996447, -24.27857615940569502 ) ) ;
#29953 = EDGE_CURVE ( 'NONE', #29309, #6553, #14466, .T. ) ;
#29954 = EDGE_CURVE ( 'NONE', #9641, #27224, #26095, .T. ) ;
#29955 = EDGE_LOOP ( 'NONE', ( #9224, #22716, #21861, #10239, #14434 ) ) ;
#29956 = LINE ( 'NONE', #13843, #12941 ) ;
#29957 = ORIENTED_EDGE ( 'NONE', *, *, #15522, .F. ) ;
#29958 = EDGE_CURVE ( 'NONE', #19336, #2732, #24843, .T. ) ;
#29959 = LINE ( 'NONE', #6549, #29872 ) ;
#29960 = EDGE_LOOP ( 'NONE', ( #22470, #15370, #5543, #17888, #22 ) ) ;
#29961 = EDGE_CURVE ( 'NONE', #22805, #12978, #23928, .T. ) ;
#29962 = CARTESIAN_POINT ( 'NONE',  ( -1.310841663519413114, -1.387778780781445676E-16, 5.000000000000000888 ) ) ;
#29963 = EDGE_LOOP ( 'NONE', ( #23888, #20151, #434, #20852 ) ) ;
#29964 = CARTESIAN_POINT ( 'NONE',  ( 9.661883061612440926, 16.25482663361732705, -17.92015940598198753 ) ) ;
#29965 = CARTESIAN_POINT ( 'NONE',  ( 20.01442678821067034, -2.980627454636011198, -16.03144472681325183 ) ) ;
#29966 = CARTESIAN_POINT ( 'NONE',  ( 20.35037346166061312, -2.402462631129500092, -18.68063351227773694 ) ) ;
#29967 = CARTESIAN_POINT ( 'NONE',  ( 16.95656709563420250, 3.789241241613106048, -19.64973185778705655 ) ) ;
#29968 = DIRECTION ( 'NONE',  ( -1.000000000000000000, -0.000000000000000000, -0.000000000000000000 ) ) ;
#29969 = PLANE ( 'NONE',  #17632 ) ;
#29970 = CARTESIAN_POINT ( 'NONE',  ( 18.97268594440662426, -2.511067197207834667, -17.06021009607598415 ) ) ;
#29971 = VERTEX_POINT ( 'NONE', #25939 ) ;
#29972 = AXIS2_PLACEMENT_3D ( 'NONE', #13939, #13499, #2226 ) ;
#29973 = CARTESIAN_POINT ( 'NONE',  ( 168.6922820468853104, -9.999999999999998224, -6.413161187712876909 ) ) ;
#29974 = CARTESIAN_POINT ( 'NONE',  ( 106.6906127300029112, -4.999999999999988454, -77.51526748729723693 ) ) ;
#29975 = ADVANCED_FACE ( 'NONE', ( #11876 ), #12182, .T. ) ;
#29976 = CARTESIAN_POINT ( 'NONE',  ( 10.36219267574928260, 16.95587413069128857, -17.77286471925143019 ) ) ;
#29977 = CARTESIAN_POINT ( 'NONE',  ( 35.54502023521215648, -22.16846120802060938, -18.59538644662325524 ) ) ;
#29978 = CARTESIAN_POINT ( 'NONE',  ( 130.7287565553229456, -4.999999999999983125, -4.785595155761468433 ) ) ;
#29979 = EDGE_LOOP ( 'NONE', ( #4162, #9499, #20902, #20575 ) ) ;
#29980 = EDGE_LOOP ( 'NONE', ( #21073, #852, #19576, #25825, #5647, #15466, #24667, #13767 ) ) ;
#29981 = LINE ( 'NONE', #27378, #6113 ) ;
#29982 = CARTESIAN_POINT ( 'NONE',  ( 17.32695330507268494, 5.471673316493076200, -20.08600194542987794 ) ) ;
#29983 = CARTESIAN_POINT ( 'NONE',  ( 11.79482239888288042, 14.29840825880376265, -16.57005305382644877 ) ) ;
#29984 = CARTESIAN_POINT ( 'NONE',  ( 35.54859390953723874, -22.18451583373416014, -15.00000000000000000 ) ) ;
#29985 = VERTEX_POINT ( 'NONE', #9891 ) ;
#29986 = ORIENTED_EDGE ( 'NONE', *, *, #11689, .T. ) ;
#29987 = CARTESIAN_POINT ( 'NONE',  ( 9.914377700407460026, 16.41675502110963336, -16.50544604630902867 ) ) ;
#29988 = EDGE_CURVE ( 'NONE', #25448, #17086, #7316, .T. ) ;
#29989 = VECTOR ( 'NONE', #14762, 1000.000000000000000 ) ;
#29990 = CARTESIAN_POINT ( 'NONE',  ( 9.641350829061996919, 17.66889105593114806, -17.91548090047172437 ) ) ;
#29991 = CARTESIAN_POINT ( 'NONE',  ( 132.0152310637605524, -1.999999999999981348, -8.721423840594310306 ) ) ;
#29992 = CARTESIAN_POINT ( 'NONE',  ( 172.7287565553229456, -9.999999999999971578, 0.5000000000000029976 ) ) ;
#29993 = EDGE_CURVE ( 'NONE', #6774, #11681, #21501, .T. ) ;
#29994 = ADVANCED_FACE ( 'NONE', ( #23340 ), #28558, .T. ) ;
#29995 = VERTEX_POINT ( 'NONE', #3351 ) ;
#29996 = CARTESIAN_POINT ( 'NONE',  ( 168.6922820468853104, -1.999999999999971800, -9.266330736598359152 ) ) ;
#29997 = EDGE_CURVE ( 'NONE', #6014, #4559, #19803, .T. ) ;
#29998 = ORIENTED_EDGE ( 'NONE', *, *, #20579, .T. ) ;
#29999 = CARTESIAN_POINT ( 'NONE',  ( 12.86835069890237548, 9.516077773083457814, -16.11535690708815594 ) ) ;
#30000 = CARTESIAN_POINT ( 'NONE',  ( 35.88208498122789791, -19.19024427843809733, -20.38849413606966010 ) ) ;
#30001 = CARTESIAN_POINT ( 'NONE',  ( 25.04992766293576878, -3.547109489677171101, -13.67097983722207033 ) ) ;
#30002 = DIRECTION ( 'NONE',  ( -2.698458740408365879E-16, 1.000000000000000000, 0.000000000000000000 ) ) ;
#30003 = CARTESIAN_POINT ( 'NONE',  ( -19.99999999999998934, 60.00000000000000711, 29.99999999999999289 ) ) ;
#30004 = CARTESIAN_POINT ( 'NONE',  ( 26.83671086236671144, -5.482767762337403816, -13.01846673106422436 ) ) ;
#30005 = CARTESIAN_POINT ( 'NONE',  ( 20.82548126942529976, -5.669333895406754031, -14.77195412306030420 ) ) ;
#30006 = EDGE_LOOP ( 'NONE', ( #9748, #27112, #8125, #24218 ) ) ;
#30007 = PLANE ( 'NONE',  #29415 ) ;
#30008 = CIRCLE ( 'NONE', #5582, 4.000000000000003553 ) ;
#30009 = FACE_OUTER_BOUND ( 'NONE', #29963, .T. ) ;
#30010 = CARTESIAN_POINT ( 'NONE',  ( 168.6922820468853104, -1.999999999999971356, -6.413161187712876909 ) ) ;
#30011 = CARTESIAN_POINT ( 'NONE',  ( 137.0152310637606092, -1.999999999999979572, -15.61832212156129351 ) ) ;
#30012 = UNCERTAINTY_MEASURE_WITH_UNIT (LENGTH_MEASURE( 1.000000000000000082E-05 ), #3163, 'distance_accuracy_value', 'NONE');
#30013 = CARTESIAN_POINT ( 'NONE',  ( 10.33811693838771717, 18.38618951776012267, -21.33333333332589632 ) ) ;
#30014 = CARTESIAN_POINT ( 'NONE',  ( 167.0152310637605524, -1.999999999999970468, -32.93883019725009120 ) ) ;
#30015 = ORIENTED_EDGE ( 'NONE', *, *, #23954, .F. ) ;
#30016 = DIRECTION ( 'NONE',  ( 1.000000000000000000, 2.698458740408365879E-16, -1.110223024625156540E-16 ) ) ;
#30017 = ORIENTED_EDGE ( 'NONE', *, *, #5192, .F. ) ;
#30018 = CARTESIAN_POINT ( 'NONE',  ( 10.55189716074911921, 7.593251366112849787, 4.999999999999998224 ) ) ;
#30019 = ADVANCED_FACE ( 'NONE', ( #3054 ), #7611, .T. ) ;
#30020 = EDGE_CURVE ( 'NONE', #21693, #23660, #7912, .T. ) ;
#30021 = CARTESIAN_POINT ( 'NONE',  ( 18.26355027798676645, 7.143056880744947712, -15.77244846760033958 ) ) ;
#30022 = CARTESIAN_POINT ( 'NONE',  ( 5.200000000000002842, 3.306546357697854719E-16, 2.700000000000001066 ) ) ;
#30023 = DIRECTION ( 'NONE',  ( -1.000000000000000000, 0.000000000000000000, -0.000000000000000000 ) ) ;
#30024 = ADVANCED_FACE ( 'NONE', ( #15220, #19352 ), #5329, .T. ) ;
#30026 = ORIENTED_EDGE ( 'NONE', *, *, #20883, .F. ) ;
#30025 = CARTESIAN_POINT ( 'NONE',  ( 21.57856661146780652, -4.666631351218505586, -18.28211233923166645 ) ) ;
#30027 = VERTEX_POINT ( 'NONE', #29164 ) ;
#30028 = CARTESIAN_POINT ( 'NONE',  ( 172.0152310637604671, -4.999999999999970690, -1.909752701132033294E-14 ) ) ;
#30029 = EDGE_CURVE ( 'NONE', #20364, #24609, #3642, .T. ) ;
#30030 = CARTESIAN_POINT ( 'NONE',  ( 12.24532799939971284, 9.516186676127107447, -15.33315318048745013 ) ) ;
#30031 = ORIENTED_EDGE ( 'NONE', *, *, #29168, .T. ) ;
#30032 = CARTESIAN_POINT ( 'NONE',  ( 34.54007435814109783, -17.65377171698271752, -20.05309729467257540 ) ) ;
#30033 = CARTESIAN_POINT ( 'NONE',  ( 15.22033579473957410, 7.355362781181614018, -19.64495939069069763 ) ) ;
#30034 = ORIENTED_EDGE ( 'NONE', *, *, #2491, .F. ) ;
#30035 = VECTOR ( 'NONE', #26029, 1000.000000000000000 ) ;
#30036 = PLANE ( 'NONE',  #25227 ) ;
#30037 = CARTESIAN_POINT ( 'NONE',  ( 20.30498772102510685, -2.023023832184298154, -16.94527736422809028 ) ) ;
#30038 = ORIENTED_EDGE ( 'NONE', *, *, #6678, .F. ) ;
#30039 = CARTESIAN_POINT ( 'NONE',  ( 149.7287565553230024, -10.00000000000000178, -16.50000000000000355 ) ) ;
#30040 =( NAMED_UNIT ( * ) SI_UNIT ( $, .STERADIAN. ) SOLID_ANGLE_UNIT ( ) );
#30041 = CARTESIAN_POINT ( 'NONE',  ( 17.46151185945609186, 6.859213057953727599, -13.86392132274949418 ) ) ;
#30042 = CARTESIAN_POINT ( 'NONE',  ( 28.79879967665997142, -10.96283228269853893, -18.01937015232834938 ) ) ;
#30043 = VERTEX_POINT ( 'NONE', #17515 ) ;
#30044 = VECTOR ( 'NONE', #5453, 1000.000000000000000 ) ;
#30045 = DIRECTION ( 'NONE',  ( 0.5877852522924731371, 1.586114251531760728E-16, 0.8090169943749474513 ) ) ;
#30046 = CARTESIAN_POINT ( 'NONE',  ( 162.0152310637604103, -4.999999999999974243, -0.06116980274991495881 ) ) ;
#30047 = EDGE_CURVE ( 'NONE', #6624, #24955, #29326, .T. ) ;
#30048 = DIRECTION ( 'NONE',  ( -0.9510565162951536422, -2.566386769018988323E-16, 0.3090169943749475623 ) ) ;
#30049 = DIRECTION ( 'NONE',  ( 0.9510565162951536422, 2.566386769018988816E-16, 0.3090169943749472292 ) ) ;
#30050 = FACE_OUTER_BOUND ( 'NONE', #17501, .T. ) ;
#30051 = CIRCLE ( 'NONE', #781, 2.100000000000000977 ) ;
#30052 = CARTESIAN_POINT ( 'NONE',  ( 139.7287565553230309, -1.999999999999978684, -7.839745962155603820 ) ) ;
#30053 = CARTESIAN_POINT ( 'NONE',  ( 18.06018518654990856, -2.098401534709970928, -17.02619504079518364 ) ) ;
#30054 = CARTESIAN_POINT ( 'NONE',  ( 21.13650371987585075, 4.769999862021419901, -15.38713752973847448 ) ) ;
#30055 = CARTESIAN_POINT ( 'NONE',  ( 32.84381624265927968, -11.41053889131397980, -20.36336433681493929 ) ) ;
#30056 = CARTESIAN_POINT ( 'NONE',  ( 11.47219014545126647, 9.272428573238919114, -15.86119603109536058 ) ) ;
#30057 = DIRECTION ( 'NONE',  ( 0.5877852522924731371, 1.586114251531760728E-16, 0.8090169943749474513 ) ) ;
#30058 = LINE ( 'NONE', #1789, #25149 ) ;
#30059 = CARTESIAN_POINT ( 'NONE',  ( 9.927226272117462003, 15.03792884684924402, -17.77782235690405344 ) ) ;
#30060 = CARTESIAN_POINT ( 'NONE',  ( 159.5152310637604671, -4.999999999999974243, -13.05155085951651195 ) ) ;
#30061 = ORIENTED_EDGE ( 'NONE', *, *, #8833, .T. ) ;
#30062 = DIRECTION ( 'NONE',  ( 1.000000000000000000, 0.000000000000000000, 0.000000000000000000 ) ) ;
#30063 = ADVANCED_FACE ( 'NONE', ( #1362 ), #26870, .F. ) ;
#30064 = CARTESIAN_POINT ( 'NONE',  ( 12.47535353872619446, 8.560407331872438519, -15.14977315560688176 ) ) ;
#30065 = VECTOR ( 'NONE', #15040, 1000.000000000000000 ) ;
#30066 = ORIENTED_EDGE ( 'NONE', *, *, #27896, .F. ) ;
#30067 = DIRECTION ( 'NONE',  ( -0.5877852522924731371, -1.586114251531760235E-16, 0.8090169943749474513 ) ) ;
#30068 = CARTESIAN_POINT ( 'NONE',  ( 131.1922820468854241, -1.999999999999982236, -22.25671179336495697 ) ) ;
#30069 = AXIS2_PLACEMENT_3D ( 'NONE', #17497, #3475, #15350 ) ;
#30070 = CARTESIAN_POINT ( 'NONE',  ( 15.19603151210977821, 9.502094893032342782, -14.87270315361914896 ) ) ;
#30071 = ORIENTED_EDGE ( 'NONE', *, *, #23918, .F. ) ;
#30072 = ORIENTED_EDGE ( 'NONE', *, *, #14851, .T. ) ;
#30073 = CARTESIAN_POINT ( 'NONE',  ( 9.112705230111354027, 16.18057050314154210, -17.05465234812585607 ) ) ;
#30074 = CARTESIAN_POINT ( 'NONE',  ( 32.12153525177792091, -10.97127362787143312, -16.88978156643115724 ) ) ;
#30075 = CARTESIAN_POINT ( 'NONE',  ( 16.77192278198516107, 3.819237988068143075, -20.73389043596634806 ) ) ;
#30076 = VECTOR ( 'NONE', #9871, 1000.000000000000000 ) ;
#30077 = CARTESIAN_POINT ( 'NONE',  ( 19.63213555404020383, 6.204410169219986670, -18.27402551702938638 ) ) ;
#30078 = VECTOR ( 'NONE', #4806, 999.9999999999998863 ) ;
#30079 = FACE_OUTER_BOUND ( 'NONE', #10976, .T. ) ;
#30080 = CARTESIAN_POINT ( 'NONE',  ( 22.33422182767193576, -8.475443503041637072, -15.36134680393336538 ) ) ;
#30081 = VECTOR ( 'NONE', #18992, 1000.000000000000000 ) ;
#30082 = VERTEX_POINT ( 'NONE', #1067 ) ;
#30083 = DIRECTION ( 'NONE',  ( 0.3090169943749475623, 8.338696094058001131E-17, 0.9510565162951536422 ) ) ;
#30084 = EDGE_CURVE ( 'NONE', #24609, #13066, #24254, .T. ) ;
#30086 = ORIENTED_EDGE ( 'NONE', *, *, #17750, .F. ) ;
#30085 = LINE ( 'NONE', #15822, #13616 ) ;
#30087 = VERTEX_POINT ( 'NONE', #22104 ) ;
#30088 = CARTESIAN_POINT ( 'NONE',  ( 143.6922820468854525, -10.00000000000000355, -23.73366926340167282 ) ) ;
#30089 = AXIS2_PLACEMENT_3D ( 'NONE', #15015, #22055, #17461 ) ;
#30090 = DIRECTION ( 'NONE',  ( -0.000000000000000000, -0.000000000000000000, 1.000000000000000000 ) ) ;
#30091 = CARTESIAN_POINT ( 'NONE',  ( 32.96976325559394638, -10.97479806523316448, -15.05356414682637833 ) ) ;
#30092 = CIRCLE ( 'NONE', #26145, 5.000000000000000888 ) ;
#30093 = CARTESIAN_POINT ( 'NONE',  ( 10.68417091768239047, 8.977850322645869241, -16.40447401652228621 ) ) ;
#30094 = AXIS2_PLACEMENT_3D ( 'NONE', #29421, #19735, #8588 ) ;
#30095 = CARTESIAN_POINT ( 'NONE',  ( 27.01132674553606350, -11.00696853675122711, -18.49859303458091730 ) ) ;
#30096 = CARTESIAN_POINT ( 'NONE',  ( 161.1922820468853388, -4.999999999999974243, -10.74328820663507678 ) ) ;
#30097 = CARTESIAN_POINT ( 'NONE',  ( 10.36007019289729847, 16.96560810760319882, -17.82599398985513872 ) ) ;
#30098 = CARTESIAN_POINT ( 'NONE',  ( 176.1922820468853104, -9.999999999999994671, -22.25671179336496053 ) ) ;
#30099 = DIRECTION ( 'NONE',  ( -0.5877852522924731371, 0.000000000000000000, 0.8090169943749474513 ) ) ;
#30100 = ORIENTED_EDGE ( 'NONE', *, *, #10605, .T. ) ;
#30101 = VERTEX_POINT ( 'NONE', #26400 ) ;
#30102 = CARTESIAN_POINT ( 'NONE',  ( -13.00000000000000178, -2.870178842070716726E-15, -23.00000000000000000 ) ) ;
#30103 = CARTESIAN_POINT ( 'NONE',  ( 0.000000000000000000, 0.000000000000000000, -4.974599999999998801 ) ) ;
#30104 = EDGE_LOOP ( 'NONE', ( #18263, #9292, #21146, #5272, #20603 ) ) ;
#30105 = CARTESIAN_POINT ( 'NONE',  ( 169.5152310637604387, -9.999999999999996447, -13.05155085951651195 ) ) ;
#30106 = VERTEX_POINT ( 'NONE', #26710 ) ;
#30107 = CARTESIAN_POINT ( 'NONE',  ( 9.667859086210386366, 16.22741982304516739, -17.88507982571460531 ) ) ;
#30108 = CARTESIAN_POINT ( 'NONE',  ( 22.53049847760648561, -4.001888697258268124, -18.07502562731026075 ) ) ;
#30109 = CARTESIAN_POINT ( 'NONE',  ( 24.39898194048076974, -1.181968365584514791, -14.84216225329429051 ) ) ;
#30110 = ORIENTED_EDGE ( 'NONE', *, *, #22315, .F. ) ;
#30111 = CARTESIAN_POINT ( 'NONE',  ( 20.05507840940144959, 2.642024363331392234, -19.51255487852252912 ) ) ;
#30112 = AXIS2_PLACEMENT_3D ( 'NONE', #20171, #14980, #19870 ) ;
#30113 = DIRECTION ( 'NONE',  ( 0.000000000000000000, 1.000000000000000000, -1.471414886128461471E-15 ) ) ;
#30114 = CARTESIAN_POINT ( 'NONE',  ( 2.500000000000000444, 1.178949249685215417, 2.041999999999998483 ) ) ;
#30115 = VERTEX_POINT ( 'NONE', #1210 ) ;
#30116 = VECTOR ( 'NONE', #16679, 1000.000000000000000 ) ;
#30117 = CARTESIAN_POINT ( 'NONE',  ( 24.14158683625483803, -3.940216521628096658, -13.50644477367014673 ) ) ;
#30118 = AXIS2_PLACEMENT_3D ( 'NONE', #15710, #25039, #8237 ) ;
#30119 =( NAMED_UNIT ( * ) SI_UNIT ( $, .STERADIAN. ) SOLID_ANGLE_UNIT ( ) );
#30120 = ADVANCED_FACE ( 'NONE', ( #26245 ), #26549, .T. ) ;
#30121 = CYLINDRICAL_SURFACE ( 'NONE', #3053, 5.000000000000000000 ) ;
#30122 = EDGE_CURVE ( 'NONE', #2975, #12094, #29017, .T. ) ;
#30123 = DIRECTION ( 'NONE',  ( 1.110223024625156540E-16, 2.995891024602366092E-32, 1.000000000000000000 ) ) ;
#30124 = EDGE_CURVE ( 'NONE', #1065, #14964, #19202, .T. ) ;
#30125 = EDGE_CURVE ( 'NONE', #23706, #5568, #741, .T. ) ;
#30126 = CARTESIAN_POINT ( 'NONE',  ( 10.35873811938078504, 16.97171716655003593, -17.89325570535168453 ) ) ;
#30127 = CARTESIAN_POINT ( 'NONE',  ( 35.54859569580823830, -22.18452385850428499, -18.27063337037174762 ) ) ;
#30128 = DIRECTION ( 'NONE',  ( 0.9510565162951535312, 2.566386769018988816E-16, -0.3090169943749475623 ) ) ;
#30129 = VERTEX_POINT ( 'NONE', #8053 ) ;
#30130 = ORIENTED_EDGE ( 'NONE', *, *, #3862, .T. ) ;
#30131 = CARTESIAN_POINT ( 'NONE',  ( 6.464122205792598663, -5.000000000000015987, 19.89452249505685799 ) ) ;
#30132 = VECTOR ( 'NONE', #18812, 1000.000000000000000 ) ;
#30133 = CARTESIAN_POINT ( 'NONE',  ( 14.79111372287554715, 6.954724682967856175, -19.27298399620107361 ) ) ;
#30134 = CARTESIAN_POINT ( 'NONE',  ( 11.06231504941914423, 17.65778033641372957, -17.63750823492871334 ) ) ;
#30135 = CARTESIAN_POINT ( 'NONE',  ( 35.18065281855160720, -20.53155141575438591, -20.22037173032050461 ) ) ;
#30136 = ORIENTED_EDGE ( 'NONE', *, *, #1515, .T. ) ;
#30137 = ORIENTED_EDGE ( 'NONE', *, *, #11412, .T. ) ;
#30138 = VECTOR ( 'NONE', #7781, 1000.000000000000000 ) ;
#30139 = CARTESIAN_POINT ( 'NONE',  ( 9.641352920869014298, 17.66888146263751125, -17.91030124961049097 ) ) ;
#30140 = CARTESIAN_POINT ( 'NONE',  ( 12.89209817343266984, 7.685947621549766851, -14.81766584744191739 ) ) ;
#30141 = LINE ( 'NONE', #11749, #19040 ) ;
#30142 = DIRECTION ( 'NONE',  ( 1.000000000000000000, 4.440892098500622217E-16, 0.000000000000000000 ) ) ;
#30143 = ORIENTED_EDGE ( 'NONE', *, *, #15891, .T. ) ;
#30144 = CARTESIAN_POINT ( 'NONE',  ( 157.0152310637604671, -10.00000000000000000, -8.721423840594312082 ) ) ;
#30145 = ORIENTED_EDGE ( 'NONE', *, *, #7201, .T. ) ;
#30146 = CARTESIAN_POINT ( 'NONE',  ( 10.48009811366078381, 16.41514476298091907, -17.33146409796769660 ) ) ;
#30147 = CARTESIAN_POINT ( 'NONE',  ( 34.27125395597954594, -11.98684039141630819, -19.88226891060491752 ) ) ;
#30148 = CARTESIAN_POINT ( 'NONE',  ( 23.22413189157496305, -7.367447486509826504, -15.63851824576001981 ) ) ;
#30149 = ORIENTED_EDGE ( 'NONE', *, *, #295, .F. ) ;
#30150 = ORIENTED_EDGE ( 'NONE', *, *, #15650, .T. ) ;
#30151 = CARTESIAN_POINT ( 'NONE',  ( 141.1922820468854525, -1.999999999999978462, -28.06379628232387446 ) ) ;
#30152 = LINE ( 'NONE', #6906, #18621 ) ;
#30153 = DIRECTION ( 'NONE',  ( 0.000000000000000000, 0.000000000000000000, 1.000000000000000000 ) ) ;
#30154 = CARTESIAN_POINT ( 'NONE',  ( 18.96102019896426683, 9.324696518442671334, -18.66317648627137515 ) ) ;
#30155 = CARTESIAN_POINT ( 'NONE',  ( 25.27624414898354388, -7.528478751523516088, -13.47981680254768655 ) ) ;
#30156 = VECTOR ( 'NONE', #2961, 1000.000000000000000 ) ;
#30157 = ORIENTED_EDGE ( 'NONE', *, *, #12445, .T. ) ;
#30158 = ORIENTED_EDGE ( 'NONE', *, *, #27098, .F. ) ;
#30159 = LINE ( 'NONE', #15745, #26950 ) ;
#30160 = ADVANCED_FACE ( 'NONE', ( #5479 ), #14761, .T. ) ;
#30161 = VECTOR ( 'NONE', #13042, 1000.000000000000000 ) ;
#30162 = ADVANCED_FACE ( 'NONE', ( #902 ), #20255, .T. ) ;
#30163 = EDGE_CURVE ( 'NONE', #21141, #28787, #15372, .T. ) ;
#30164 = EDGE_CURVE ( 'NONE', #8350, #28740, #10750, .T. ) ;
#30165 = DIRECTION ( 'NONE',  ( -1.000000000000000000, 0.000000000000000000, 0.000000000000000000 ) ) ;
#30166 = CARTESIAN_POINT ( 'NONE',  ( 143.6922820468854525, -10.00000000000000355, -35.24709285013155835 ) ) ;
#30167 = LINE ( 'NONE', #47, #17776 ) ;
#30168 = CARTESIAN_POINT ( 'NONE',  ( 10.33811811146757265, 18.38618413786636552, -17.91101973220562371 ) ) ;
#30169 = LINE ( 'NONE', #9330, #18017 ) ;
#30170 = ORIENTED_EDGE ( 'NONE', *, *, #7321, .F. ) ;
#30171 = CARTESIAN_POINT ( 'NONE',  ( 153.6922820468853388, -4.999999999999976019, -0.6060766987539614181 ) ) ;
#30172 = ORIENTED_EDGE ( 'NONE', *, *, #13009, .T. ) ;
#30173 = CARTESIAN_POINT ( 'NONE',  ( 11.46269231744662420, 9.315986823159681407, -15.86512371708112212 ) ) ;
#30174 = ORIENTED_EDGE ( 'NONE', *, *, #9367, .F. ) ;
#30175 = CARTESIAN_POINT ( 'NONE',  ( 17.51631511252498186, 5.448942031446791567, -19.07752241466814880 ) ) ;
#30176 = CARTESIAN_POINT ( 'NONE',  ( 0.000000000000000000, 0.000000000000000000, 2.550000000000000266 ) ) ;
#30177 = DIRECTION ( 'NONE',  ( -0.5877852522924731371, -1.586114251531760728E-16, -0.8090169943749474513 ) ) ;
#30179 = VERTEX_POINT ( 'NONE', #24861 ) ;
#30178 = CARTESIAN_POINT ( 'NONE',  ( 174.5152310637604103, -1.999999999999970024, -2.627941064794695691 ) ) ;
#30180 = EDGE_LOOP ( 'NONE', ( #12575, #26278, #9250, #29252 ) ) ;
#30181 = DIRECTION ( 'NONE',  ( 0.000000000000000000, -1.000000000000000000, 0.000000000000000000 ) ) ;
#30182 = CARTESIAN_POINT ( 'NONE',  ( 12.24853674868645292, 9.517605834602926862, -15.33059566259575668 ) ) ;
#30183 = AXIS2_PLACEMENT_3D ( 'NONE', #2486, #13893, #11906 ) ;
#30184 = CARTESIAN_POINT ( 'NONE',  ( 34.93238815599637803, -19.41622979634004764, -20.17168434421570922 ) ) ;
#30185 = DIRECTION ( 'NONE',  ( 0.5840962589317576503, -0.8116843969807016057, 0.000000000000000000 ) ) ;
#30186 = FACE_OUTER_BOUND ( 'NONE', #9755, .T. ) ;
#30187 = CARTESIAN_POINT ( 'NONE',  ( 21.64008331710702038, -0.7226702609205537531, -18.85644019536628946 ) ) ;
#30188 = VERTEX_POINT ( 'NONE', #3798 ) ;
#30189 = DIRECTION ( 'NONE',  ( -1.000000000000000000, 0.000000000000000000, -0.000000000000000000 ) ) ;
#30190 = EDGE_CURVE ( 'NONE', #1623, #13813, #4799, .T. ) ;
#30191 = CARTESIAN_POINT ( 'NONE',  ( 22.47820520476076567, 2.340993144345510313, -15.49451772223075707 ) ) ;
#30192 = CARTESIAN_POINT ( 'NONE',  ( 27.79808892257030806, -9.771933472778439267, -13.29678235002263165 ) ) ;
#30193 = VERTEX_POINT ( 'NONE', #22412 ) ;
#30194 = EDGE_CURVE ( 'NONE', #11751, #16627, #8656, .T. ) ;
#30195 = VECTOR ( 'NONE', #19242, 1000.000000000000000 ) ;
#30196 = EDGE_CURVE ( 'NONE', #9083, #9595, #15824, .T. ) ;
#30197 = DIRECTION ( 'NONE',  ( -2.698458740408365879E-16, 1.000000000000000000, 0.000000000000000000 ) ) ;
#30198 = ADVANCED_FACE ( 'NONE', ( #15679 ), #10949, .T. ) ;
#30199 = CARTESIAN_POINT ( 'NONE',  ( 0.000000000000000000, 0.000000000000000000, -2.450000000000000178 ) ) ;
#30200 = VECTOR ( 'NONE', #1389, 1000.000000000000000 ) ;
#30201 = DIRECTION ( 'NONE',  ( -0.5877852522924731371, 0.000000000000000000, 0.8090169943749474513 ) ) ;
#30202 = CARTESIAN_POINT ( 'NONE',  ( 9.917712295358372288, 16.40146214360271770, -16.50402730409559027 ) ) ;
#30203 = AXIS2_PLACEMENT_3D ( 'NONE', #9122, #14303, #14158 ) ;
#30204 = CARTESIAN_POINT ( 'NONE',  ( 21.41414477019618090, -0.8106431452899078849, -12.56463806509592018 ) ) ;
#30205 = CARTESIAN_POINT ( 'NONE',  ( 14.50439321891314925, 5.533609182599570353, -15.17065254761420512 ) ) ;
#30206 = CARTESIAN_POINT ( 'NONE',  ( 31.83585693452864973, -10.27807049784803972, -18.08404909334234745 ) ) ;
#30207 = VECTOR ( 'NONE', #23649, 1000.000000000000000 ) ;
#30208 = CARTESIAN_POINT ( 'NONE',  ( 153.6922820468853388, -4.999999999999976019, -15.07341522555727309 ) ) ;
#30209 = CARTESIAN_POINT ( 'NONE',  ( 144.7287565553230309, -10.00000000000000355, -16.50000000000000355 ) ) ;
#30210 = DIRECTION ( 'NONE',  ( -0.5877852522924731371, 0.000000000000000000, 0.8090169943749474513 ) ) ;
#30211 = CARTESIAN_POINT ( 'NONE',  ( 17.85084670134855145, 5.929878015568476712, -20.08862479909851828 ) ) ;
#30212 = ORIENTED_EDGE ( 'NONE', *, *, #9472, .T. ) ;
#30213 = PLANE ( 'NONE',  #19778 ) ;
#30214 = CARTESIAN_POINT ( 'NONE',  ( 12.93612603019711571, 8.763434079353435990, -14.78257486846209545 ) ) ;
#30215 = VERTEX_POINT ( 'NONE', #4096 ) ;
#30216 = DIRECTION ( 'NONE',  ( -0.5877852522924731371, -1.586114251531760728E-16, -0.8090169943749474513 ) ) ;
#30217 = LINE ( 'NONE', #25570, #23964 ) ;
#30218 = CARTESIAN_POINT ( 'NONE',  ( 14.24706144987486667, 6.238427219560604087, -16.72753349211556184 ) ) ;
#30219 = ORIENTED_EDGE ( 'NONE', *, *, #8836, .T. ) ;
#30220 = CARTESIAN_POINT ( 'NONE',  ( 34.52807818452484412, -18.59987926346575549, -21.09179268733712576 ) ) ;
#30221 = ORIENTED_EDGE ( 'NONE', *, *, #22240, .F. ) ;
#30222 = EDGE_CURVE ( 'NONE', #19874, #8637, #13088, .T. ) ;
#30223 = CIRCLE ( 'NONE', #18457, 2.500000000000001332 ) ;
#30224 = CARTESIAN_POINT ( 'NONE',  ( 19.88777865313588222, 4.107626486979258473, -13.29018489620430721 ) ) ;
#30225 = CARTESIAN_POINT ( 'NONE',  ( 18.83884422780463552, 9.149888288241003309, -18.99120665306858768 ) ) ;
#30226 = AXIS2_PLACEMENT_3D ( 'NONE', #22174, #22634, #6003 ) ;
#30227 = DIRECTION ( 'NONE',  ( -2.908569913943825554E-16, 1.000000000000000000, 0.000000000000000000 ) ) ;
#30228 = CARTESIAN_POINT ( 'NONE',  ( 22.29950228926167100, 0.3472756386405770335, -13.33132414558515677 ) ) ;
#30229 = VECTOR ( 'NONE', #22217, 1000.000000000000000 ) ;
#30230 = ADVANCED_FACE ( 'NONE', ( #25011 ), #7093, .T. ) ;
#30231 = EDGE_LOOP ( 'NONE', ( #1476, #24888, #24420, #12313, #26829 ) ) ;
#30232 = EDGE_CURVE ( 'NONE', #28625, #8203, #29195, .T. ) ;
#30233 = PLANE ( 'NONE',  #26982 ) ;
#30234 = EDGE_CURVE ( 'NONE', #15731, #26001, #25715, .T. ) ;
#30236 = ORIENTED_EDGE ( 'NONE', *, *, #10564, .F. ) ;
#30235 = PLANE ( 'NONE',  #14088 ) ;
#30237 = DIRECTION ( 'NONE',  ( -1.000000000000000000, -4.440892098500622217E-16, -0.000000000000000000 ) ) ;
#30238 = LINE ( 'NONE', #23020, #25836 ) ;
#30239 = CARTESIAN_POINT ( 'NONE',  ( 34.58206770820681442, -12.34995000336197890, -18.95321163875382453 ) ) ;
#30240 = VECTOR ( 'NONE', #27407, 1000.000000000000000 ) ;
#30241 = CARTESIAN_POINT ( 'NONE',  ( 12.73046782819888989, 7.614823354231524455, -14.94646497050939793 ) ) ;
#30242 = ORIENTED_EDGE ( 'NONE', *, *, #13412, .T. ) ;
#30243 = CARTESIAN_POINT ( 'NONE',  ( 2.500000000000000444, -1.178949249685215417, 2.042000000000002036 ) ) ;
#30244 = LINE ( 'NONE', #25594, #167 ) ;
#30245 = CARTESIAN_POINT ( 'NONE',  ( 10.40163623209820365, 16.77498095339038287, -17.46874319472340176 ) ) ;
#30246 = DIRECTION ( 'NONE',  ( -1.000000000000000000, 0.000000000000000000, -0.000000000000000000 ) ) ;
#30247 = AXIS2_PLACEMENT_3D ( 'NONE', #8362, #17664, #29016 ) ;
#30248 = DIRECTION ( 'NONE',  ( -2.698458740408365879E-16, 1.000000000000000000, 0.000000000000000000 ) ) ;
#30249 = VERTEX_POINT ( 'NONE', #11102 ) ;
#30250 = DIRECTION ( 'NONE',  ( -0.9510565162951536422, 0.000000000000000000, -0.3090169943749472292 ) ) ;
#30251 = VERTEX_POINT ( 'NONE', #17668 ) ;
#30252 = DIRECTION ( 'NONE',  ( -0.5877852522924731371, 0.000000000000000000, 0.8090169943749474513 ) ) ;
#30253 = EDGE_LOOP ( 'NONE', ( #9958, #9918, #26261, #9471 ) ) ;
#30254 = CARTESIAN_POINT ( 'NONE',  ( 130.7287565553229456, -9.999999999999982236, 3.500000000000003109 ) ) ;
#30255 = ORIENTED_EDGE ( 'NONE', *, *, #26253, .F. ) ;
#30256 = CARTESIAN_POINT ( 'NONE',  ( 9.927226272117462003, 15.03792884684924402, -17.77782235690405344 ) ) ;
#30257 = EDGE_CURVE ( 'NONE', #30188, #8805, #29798, .T. ) ;
#30258 = CARTESIAN_POINT ( 'NONE',  ( 20.12919692000023986, -2.949910412001375715, -15.69023992059449846 ) ) ;
#30259 = CARTESIAN_POINT ( 'NONE',  ( 23.86816030614728135, 2.079196616232401595, -15.13732202275373062 ) ) ;
#30260 = VERTEX_POINT ( 'NONE', #27479 ) ;
#30261 = CARTESIAN_POINT ( 'NONE',  ( 19.47744964272635926, 1.166342761889149982, -14.46873920536258495 ) ) ;
#30262 =( NAMED_UNIT ( * ) PLANE_ANGLE_UNIT ( ) SI_UNIT ( $, .RADIAN. ) );
#30263 = NEXT_ASSEMBLY_USAGE_OCCURRENCE ( 'NAUO1', ' ', ' ', #580, #15091, $ ) ;
#30264 = NEXT_ASSEMBLY_USAGE_OCCURRENCE ( 'NAUO2', ' ', ' ', #580, #26898, $ ) ;
#30265 = NEXT_ASSEMBLY_USAGE_OCCURRENCE ( 'NAUO3', ' ', ' ', #580, #11917, $ ) ;
#30266 = NEXT_ASSEMBLY_USAGE_OCCURRENCE ( 'NAUO4', ' ', ' ', #580, #735, $ ) ;
#30267 = NEXT_ASSEMBLY_USAGE_OCCURRENCE ( 'NAUO5', ' ', ' ', #580, #9305, $ ) ;
#30268 = NEXT_ASSEMBLY_USAGE_OCCURRENCE ( 'NAUO6', ' ', ' ', #580, #28218, $ ) ;
#30269 = NEXT_ASSEMBLY_USAGE_OCCURRENCE ( 'NAUO7', ' ', ' ', #580, #6153, $ ) ;
#30270 = NEXT_ASSEMBLY_USAGE_OCCURRENCE ( 'NAUO8', ' ', ' ', #580, #27455, $ ) ;
#30271 = NEXT_ASSEMBLY_USAGE_OCCURRENCE ( 'NAUO9', ' ', ' ', #580, #4667, $ ) ;
#30272 = NEXT_ASSEMBLY_USAGE_OCCURRENCE ( 'NAUO10', ' ', ' ', #580, #7839, $ ) ;
#30273 = NEXT_ASSEMBLY_USAGE_OCCURRENCE ( 'NAUO11', ' ', ' ', #580, #7839, $ ) ;
ENDSEC;
END-ISO-10303-21;
